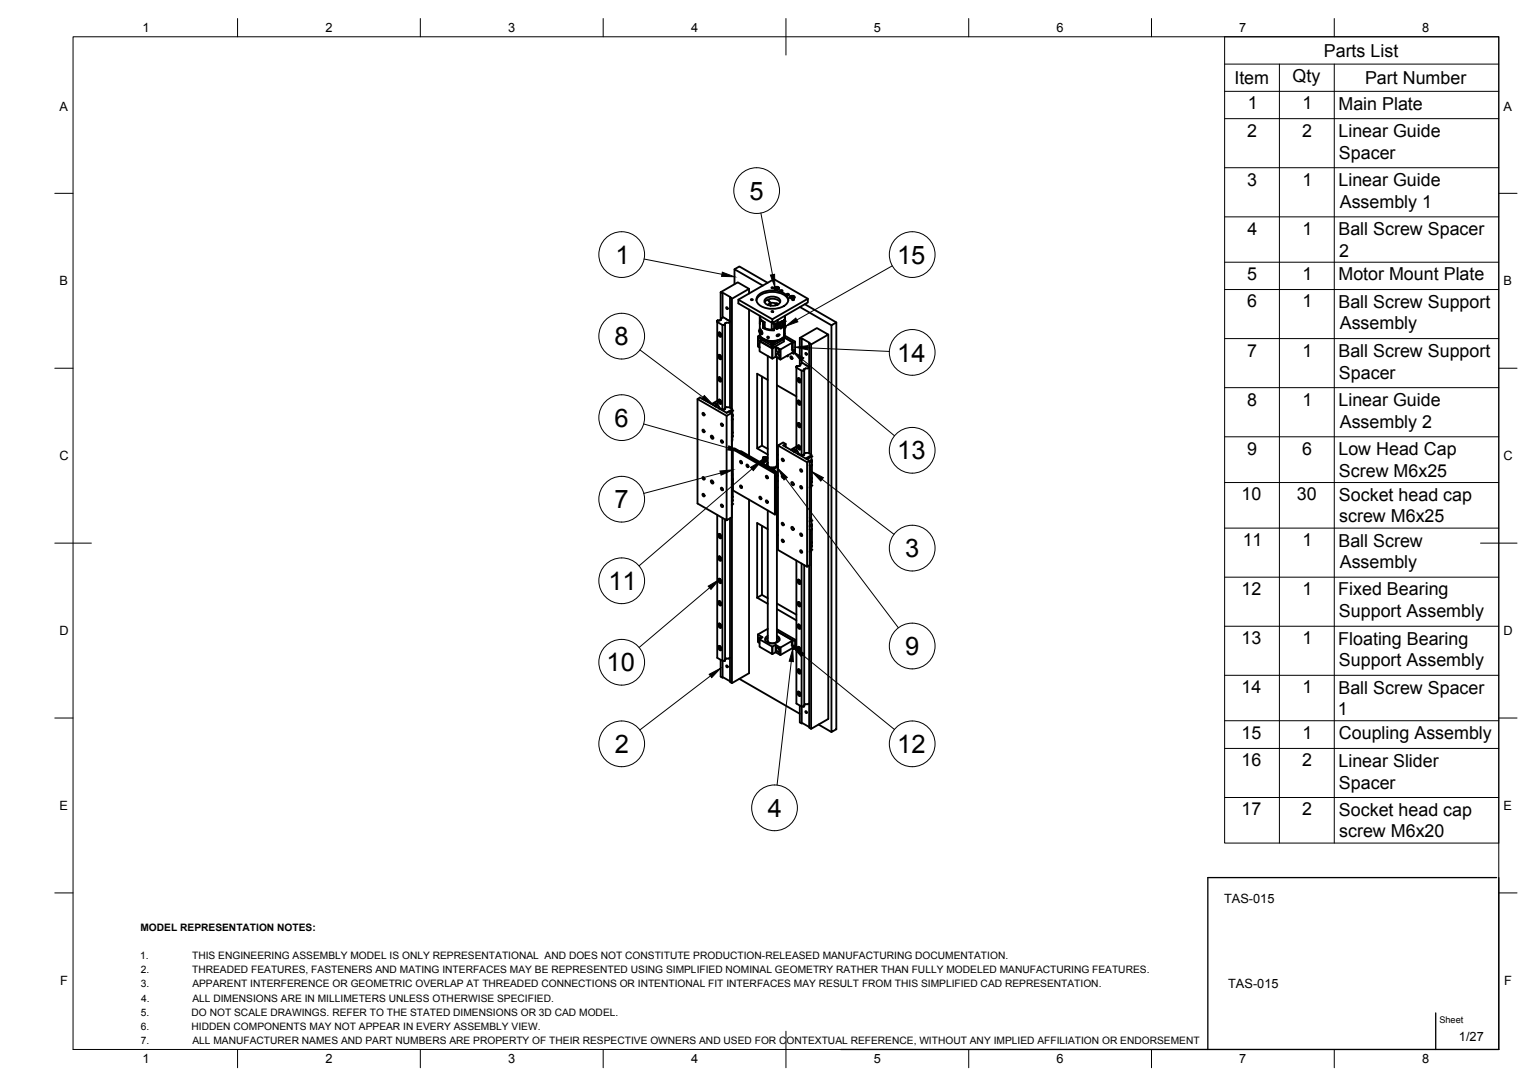
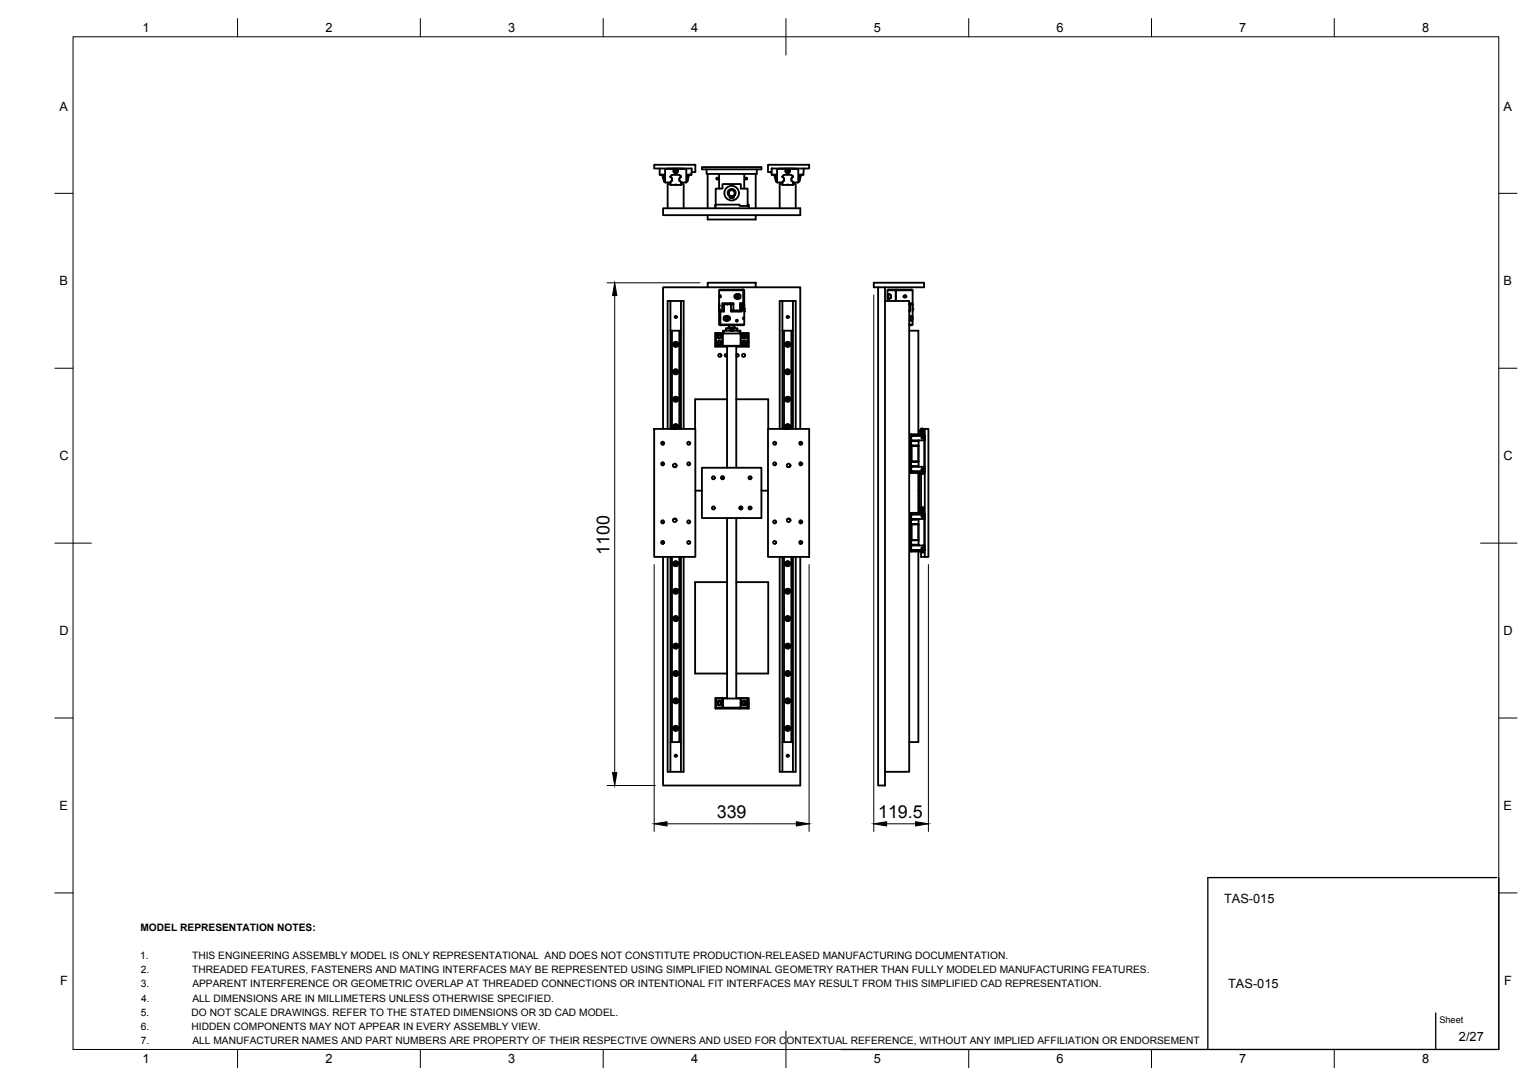
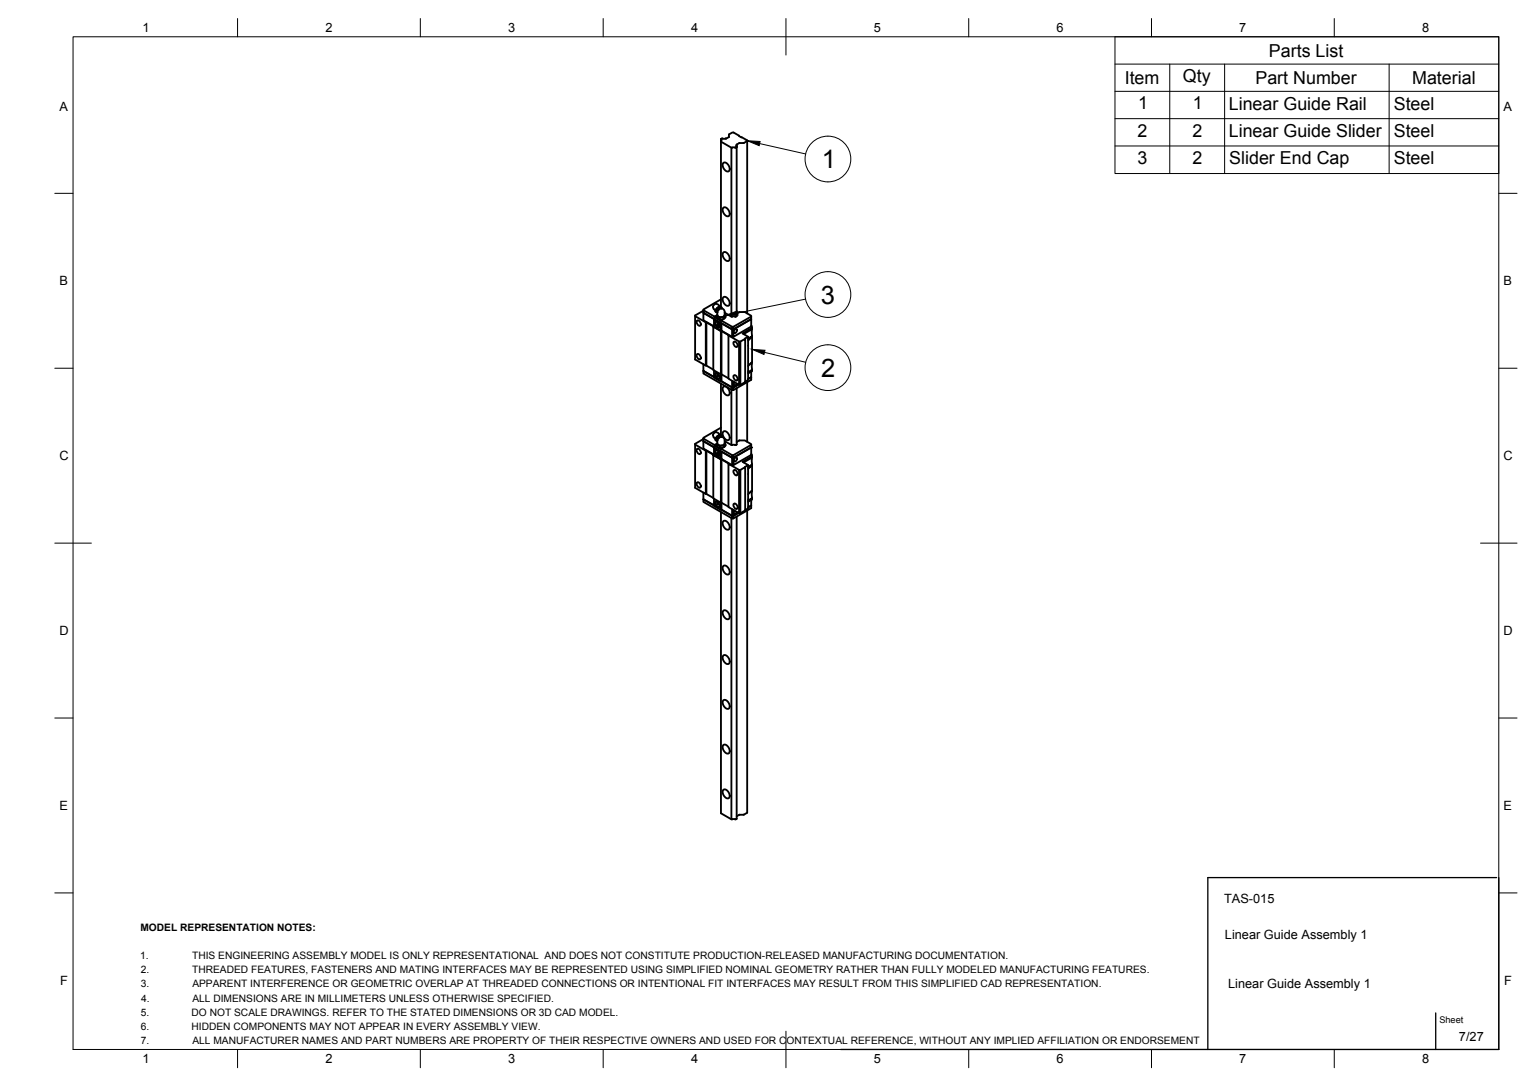
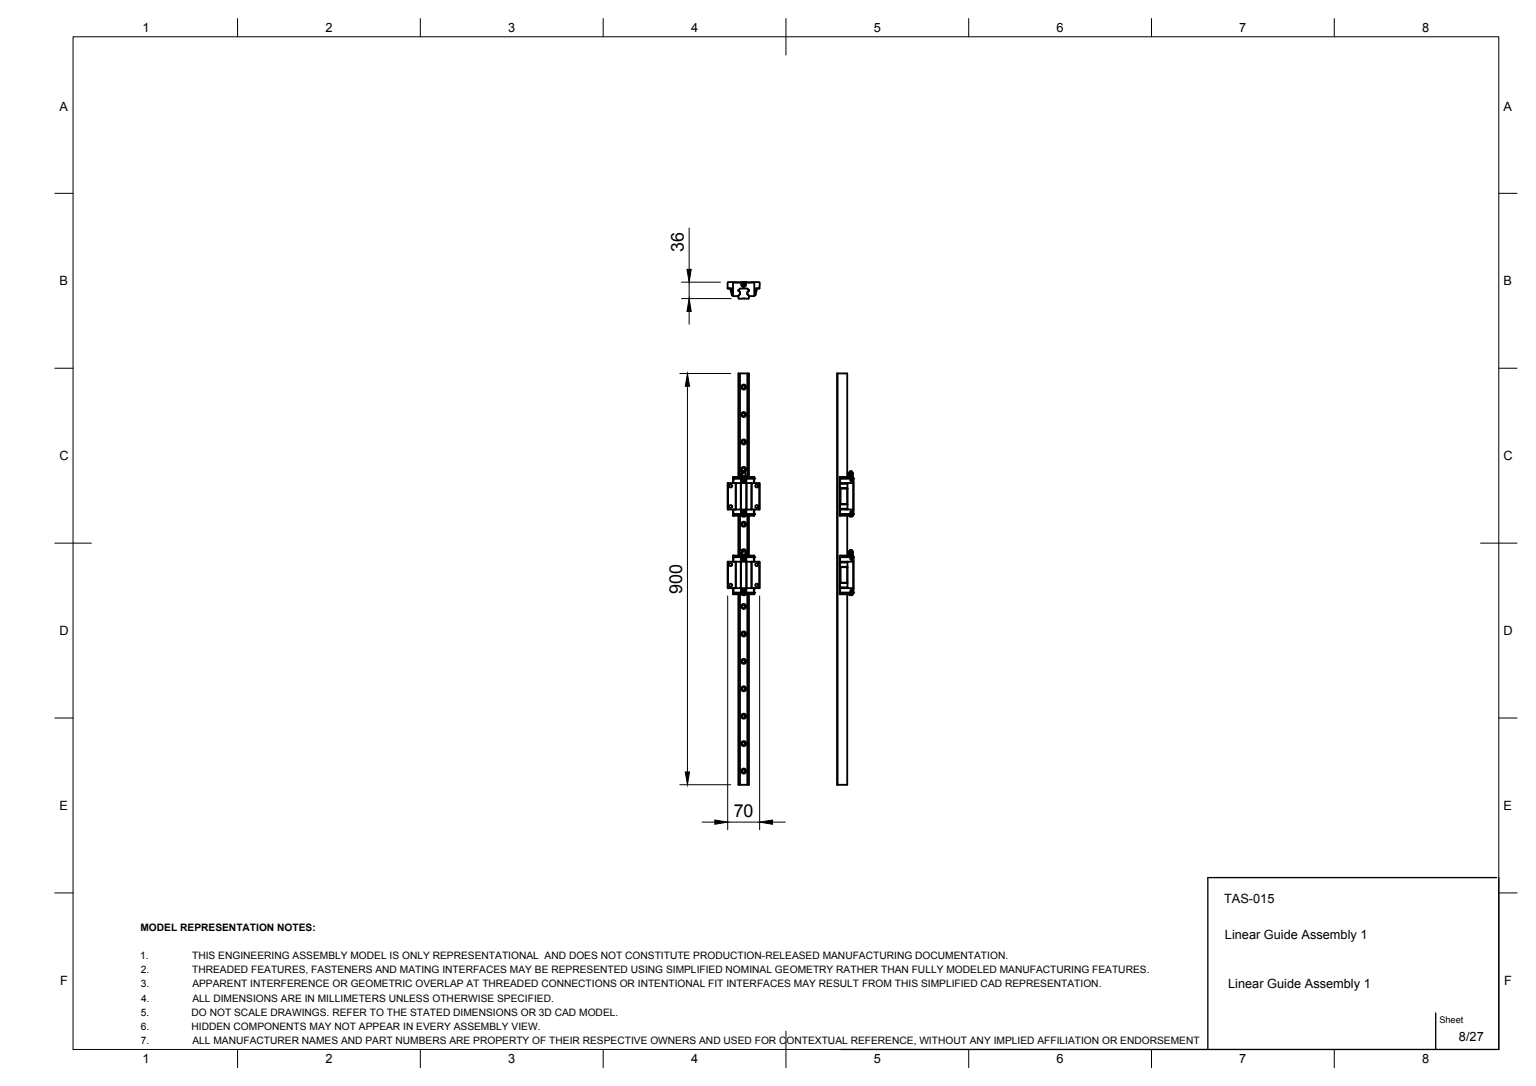
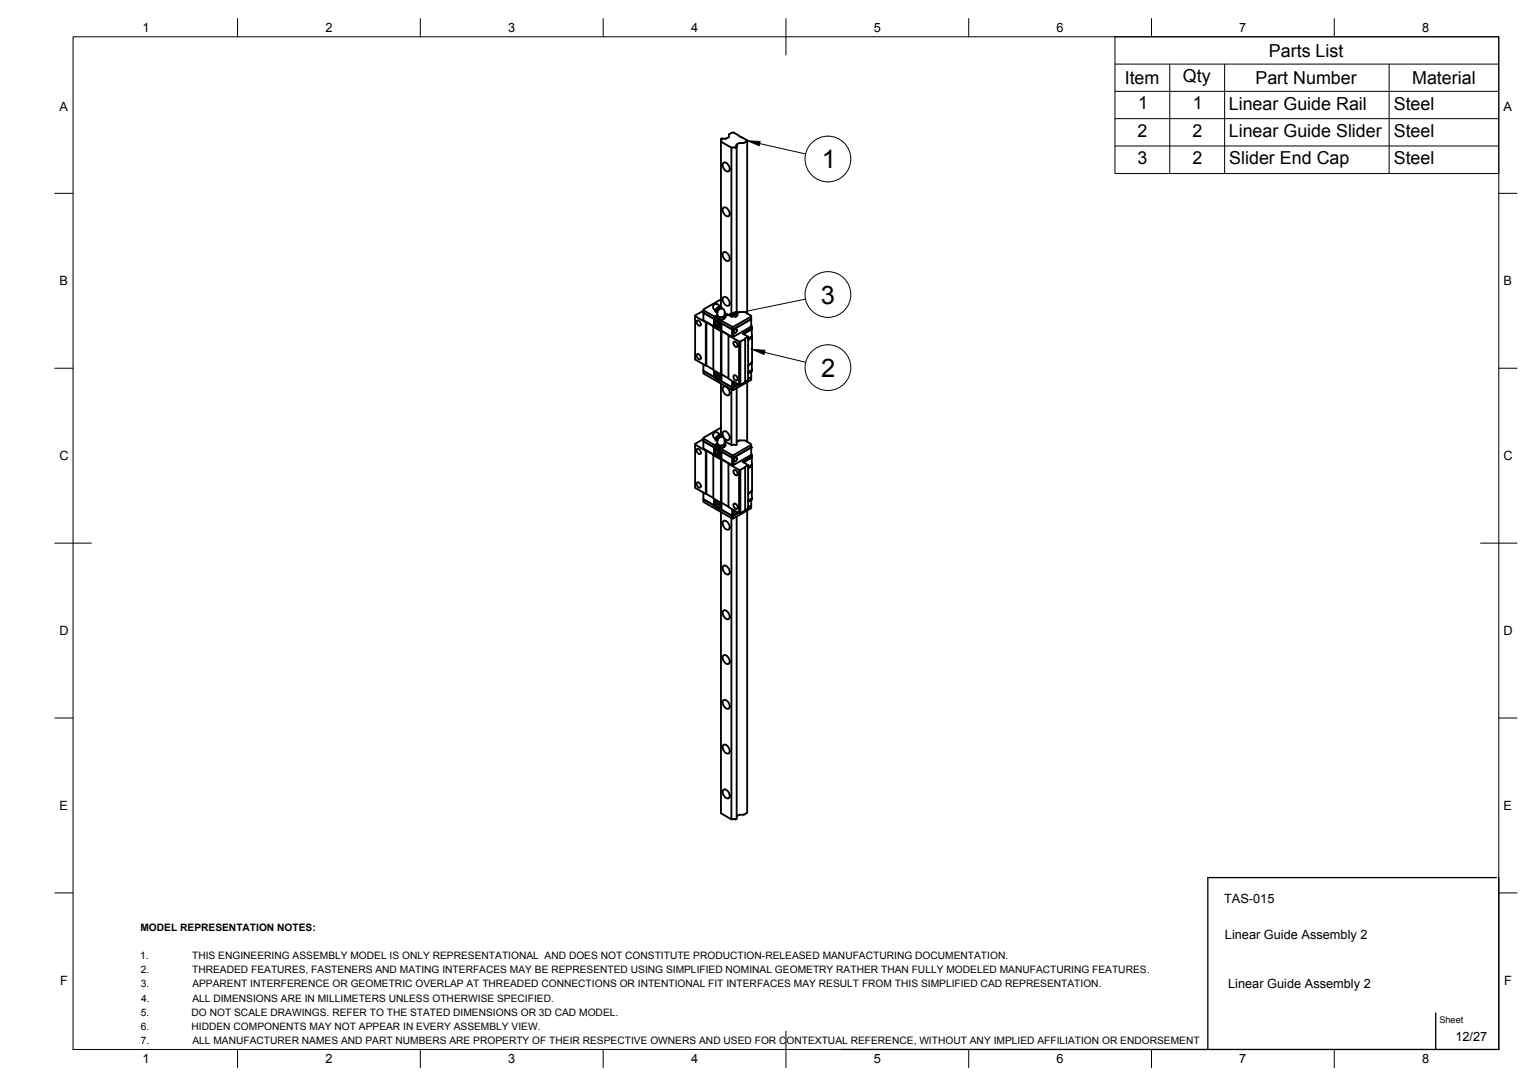
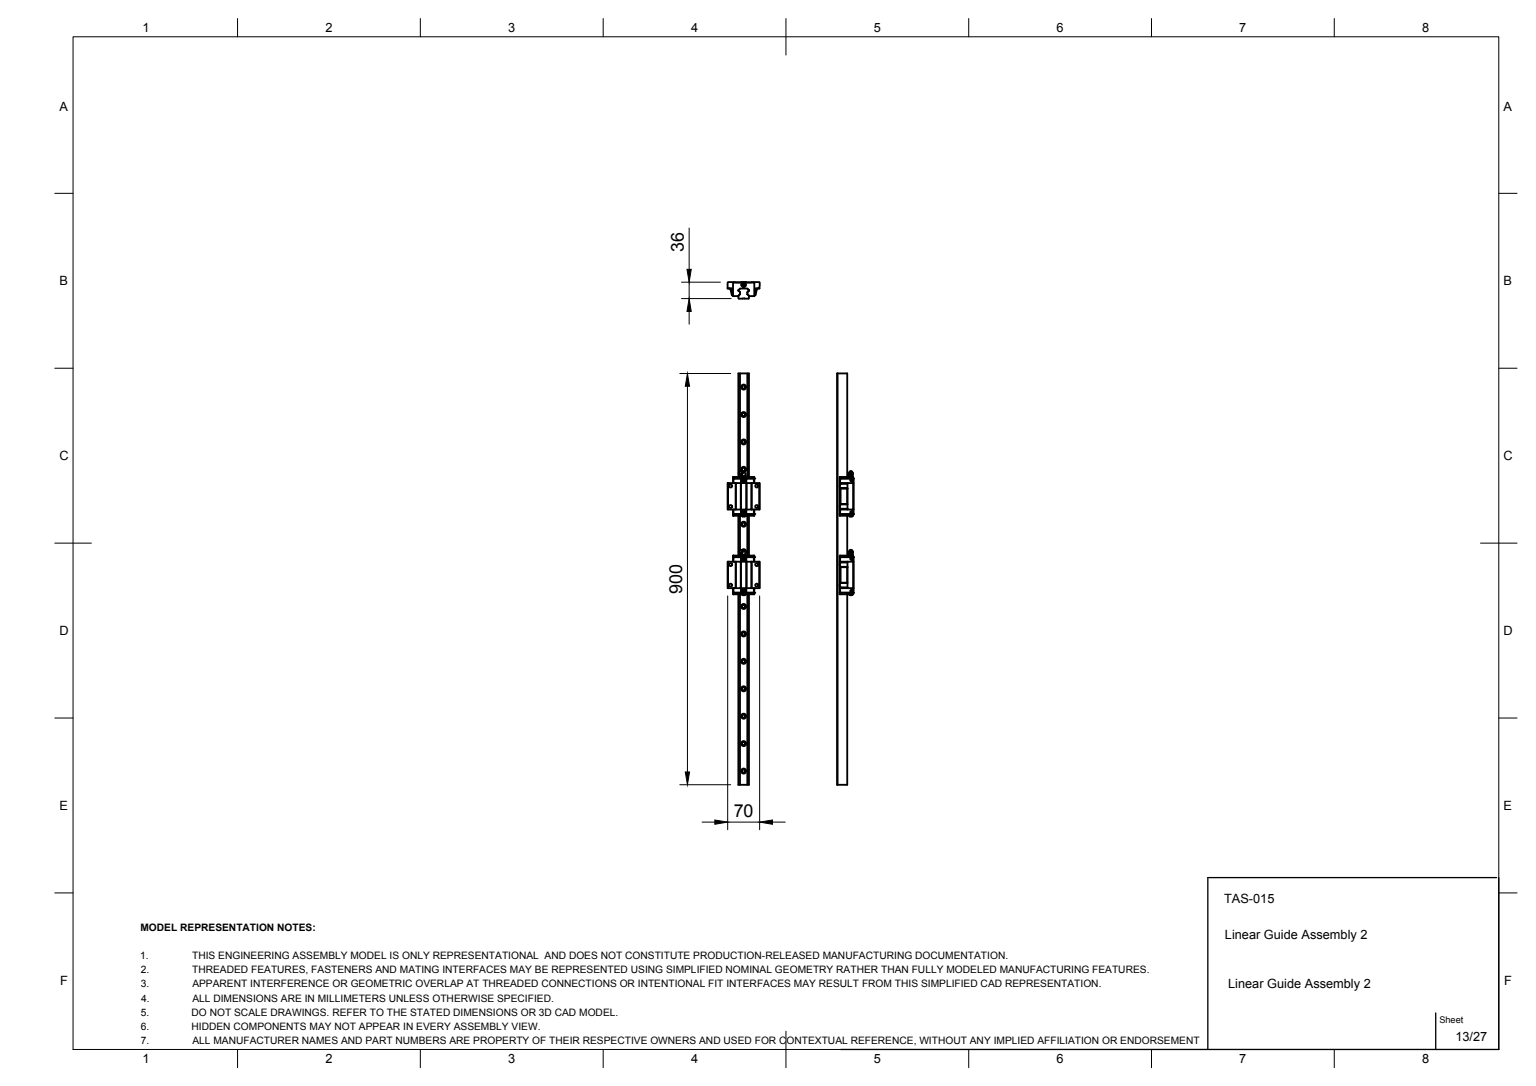
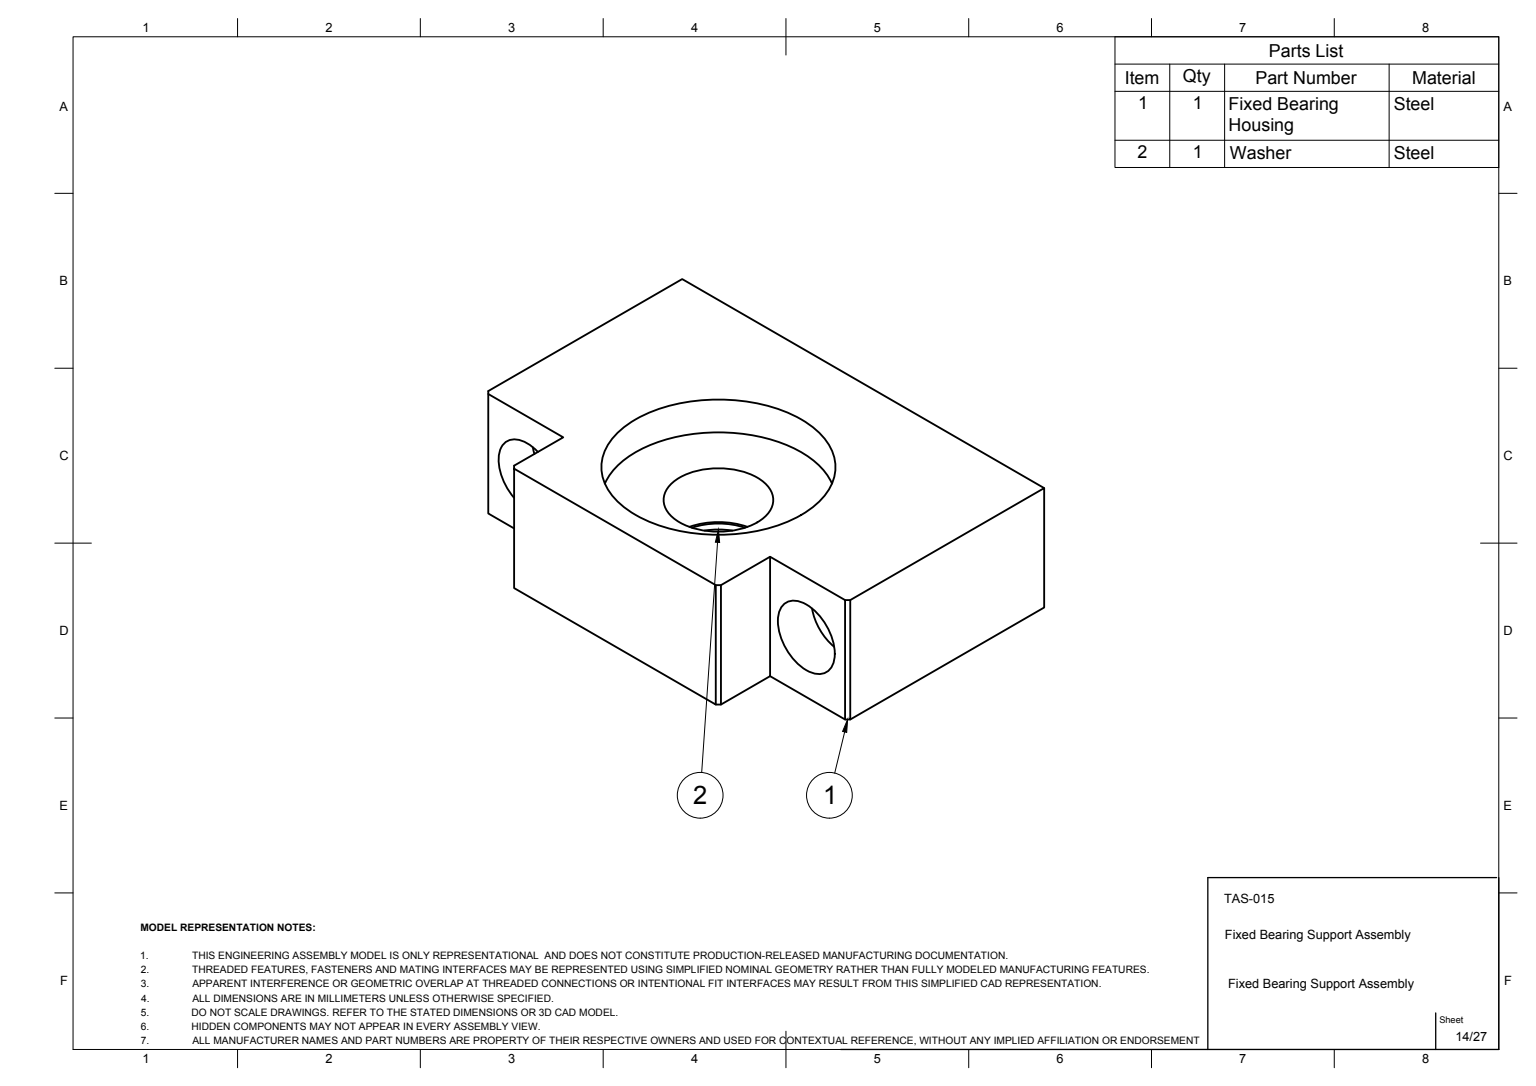
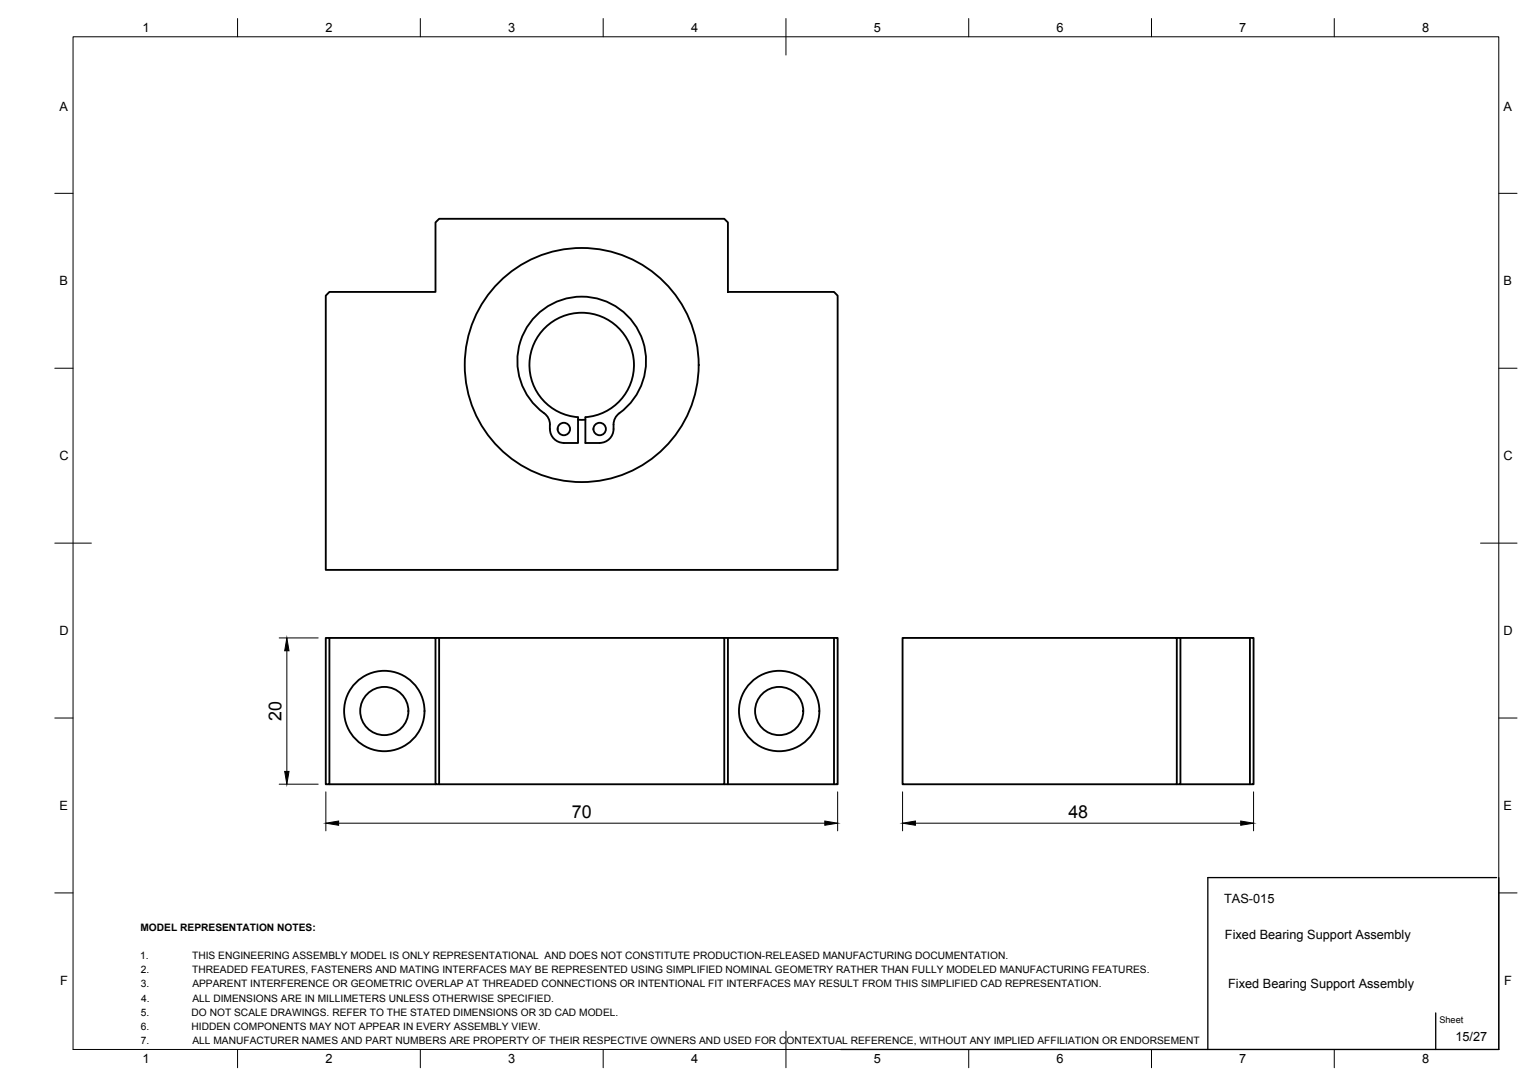
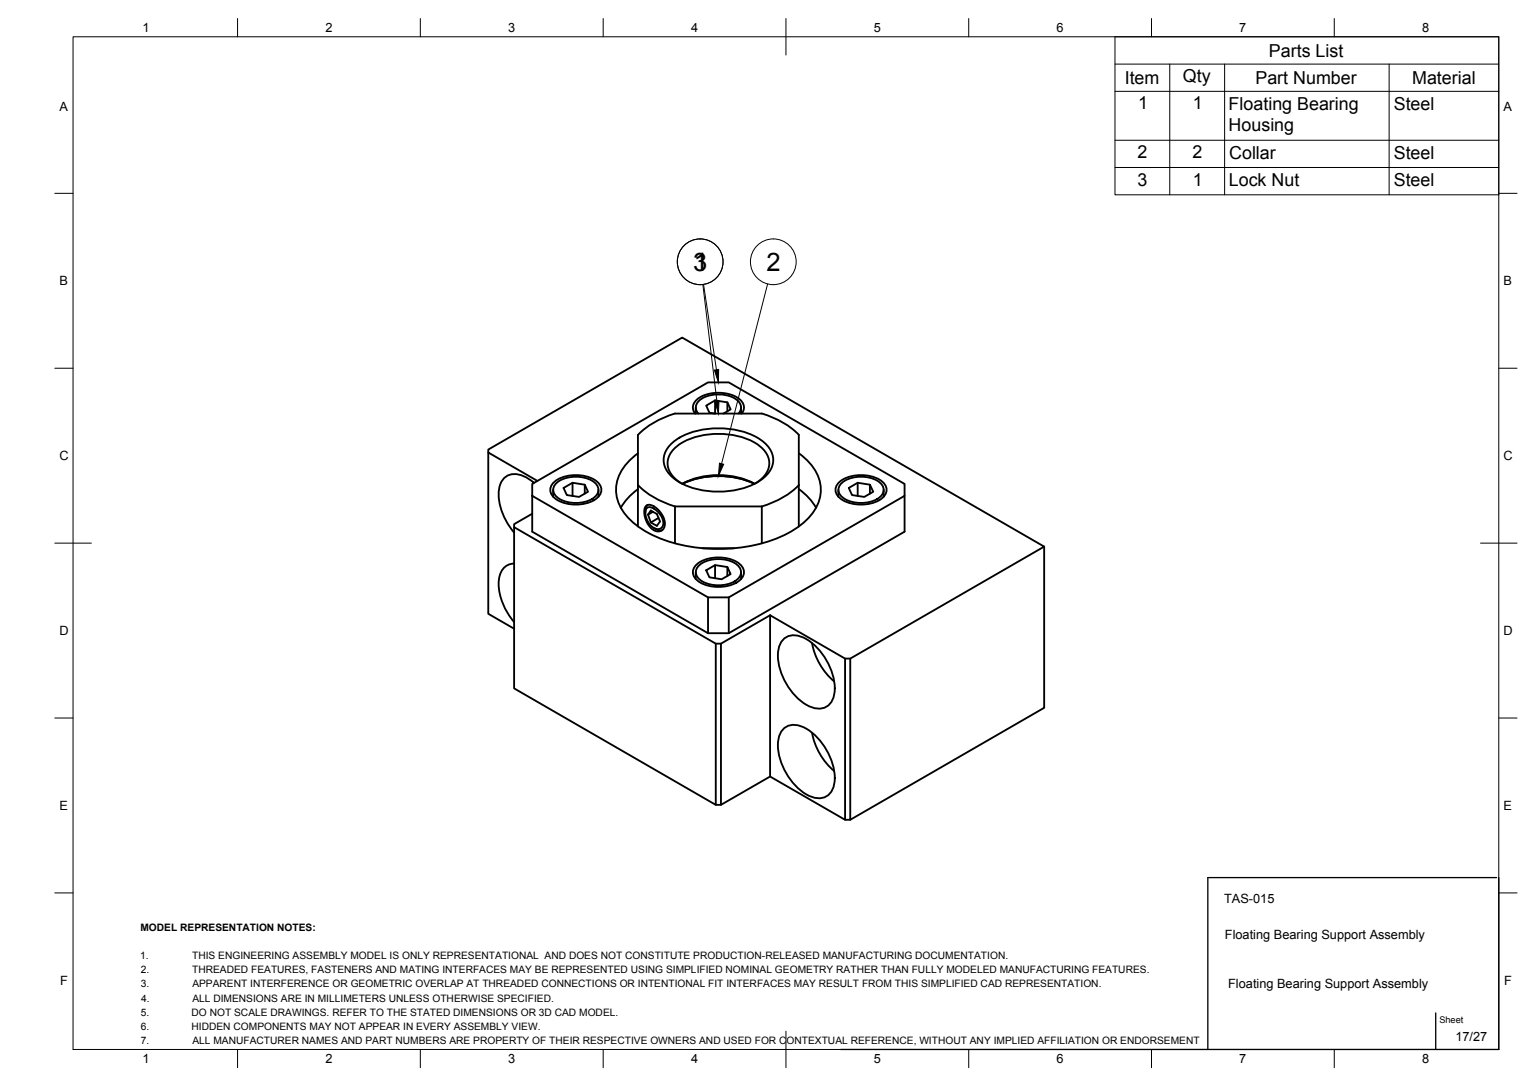
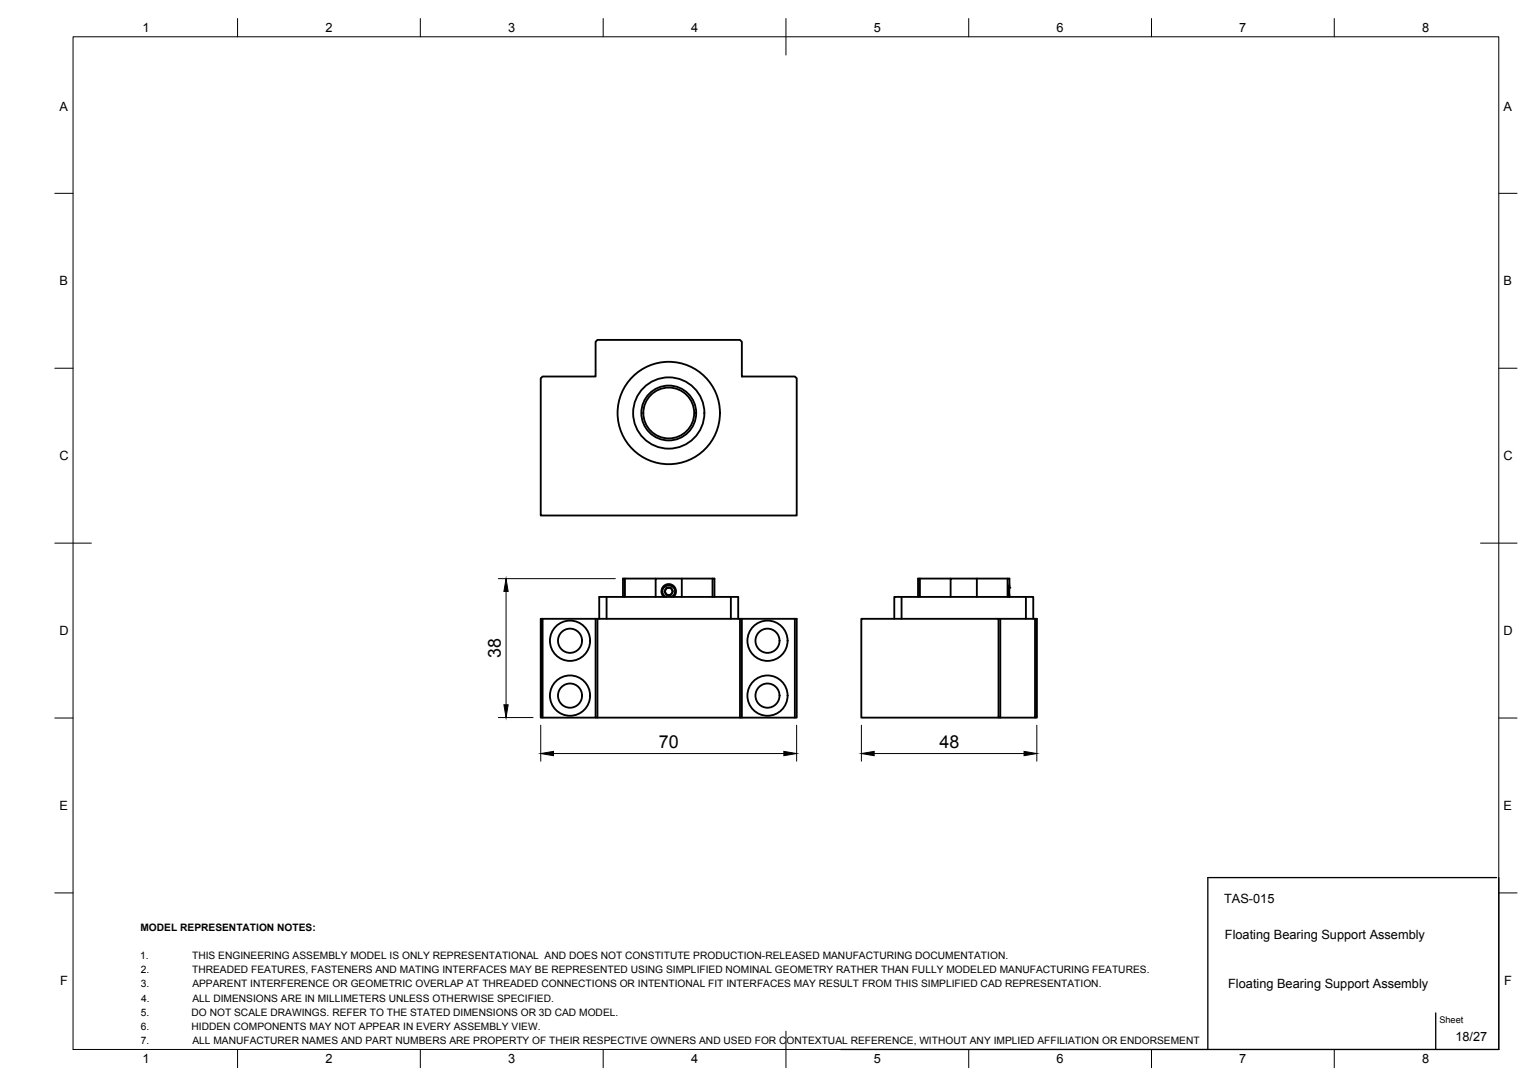
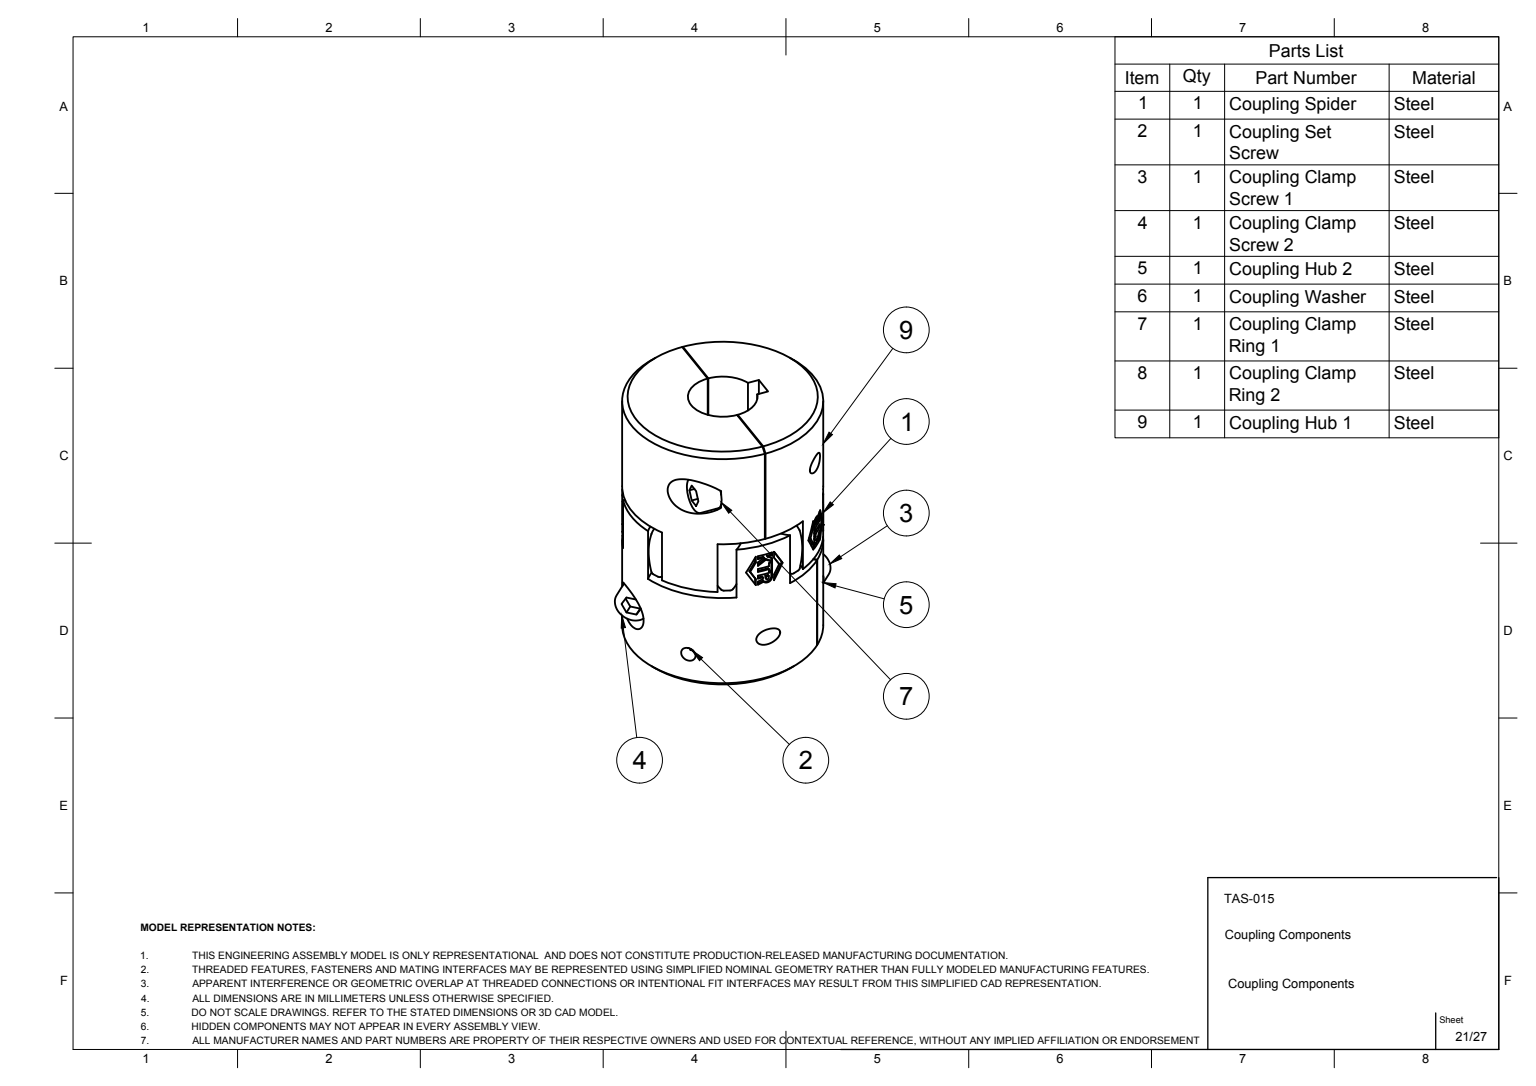
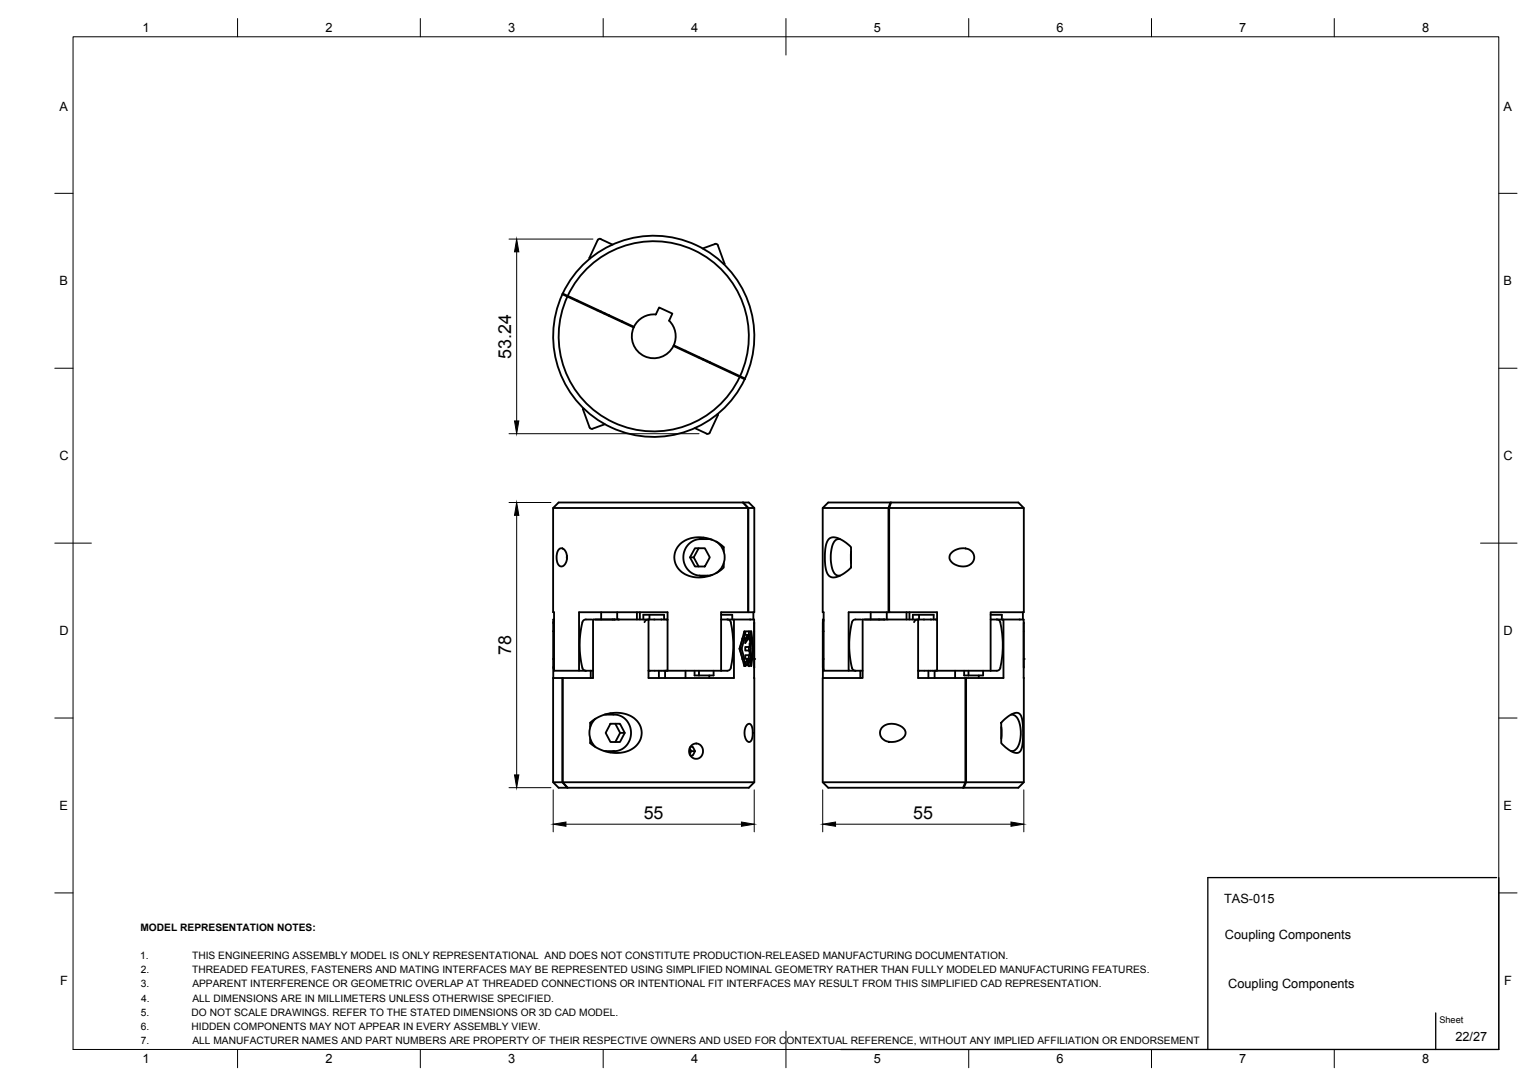
ISO-10303-21;
HEADER;
/* Generated by software containing ST-Developer
 * from STEP Tools, Inc. (www.steptools.com) 
 */

FILE_DESCRIPTION(
/* description */ ('STEP AP214'),
/* implementation_level */ '2;1');

FILE_NAME(
/* name */ 'TAS-015.step',
/* time_stamp */ '2026-11-15T14:49:54-08:00',
/* author */ (''),
/* organization */ (''),
/* preprocessor_version */ 'ST-DEVELOPER v20.2',
/* originating_system */ 'Autodesk Translation Framework v15.17.0.0',
/* authorisation */ '');

FILE_SCHEMA (('AUTOMOTIVE_DESIGN { 1 0 10303 214 3 1 1 }'));
ENDSEC;

DATA;
#10=MECHANICAL_DESIGN_GEOMETRIC_PRESENTATION_REPRESENTATION('',(#1098,#1099,
#1100,#1101,#1102,#1103,#1104,#1105,#1106,#1107,#1108,#1109,#1110,#1111,
#1112,#1113,#1114,#1115,#1116,#1117,#1118,#1119,#1120,#1121,#1122,#1123,
#1124,#1125,#1126,#1127,#1128,#1129,#1130,#1131,#1132),#66721);
#11=B_SPLINE_SURFACE_WITH_KNOTS('',3,3,((#41982,#41983,#41984,#41985,#41986),
(#41987,#41988,#41989,#41990,#41991),(#41992,#41993,#41994,#41995,#41996),
(#41997,#41998,#41999,#42000,#42001),(#42002,#42003,#42004,#42005,#42006),
(#42007,#42008,#42009,#42010,#42011),(#42012,#42013,#42014,#42015,#42016)),
 .UNSPECIFIED.,.F.,.F.,.F.,(4,1,1,1,4),(4,1,4),(0.02704890409976,0.25,0.5,
0.75,0.9277040914243),(0.6266253876044,7.194455259721,13.76279800701),
 .UNSPECIFIED.);
#12=B_SPLINE_SURFACE_WITH_KNOTS('',3,3,((#43036,#43037,#43038,#43039,#43040),
(#43041,#43042,#43043,#43044,#43045),(#43046,#43047,#43048,#43049,#43050),
(#43051,#43052,#43053,#43054,#43055)),.UNSPECIFIED.,.F.,.F.,.F.,(4,4),(4,
1,4),(0.07560247213886,0.9246170074165),(0.97123707704753,7.194455259721,
13.4176757847934),.UNSPECIFIED.);
#13=B_SPLINE_SURFACE_WITH_KNOTS('',3,3,((#43854,#43855,#43856,#43857,#43858),
(#43859,#43860,#43861,#43862,#43863),(#43864,#43865,#43866,#43867,#43868),
(#43869,#43870,#43871,#43872,#43873),(#43874,#43875,#43876,#43877,#43878),
(#43879,#43880,#43881,#43882,#43883),(#43884,#43885,#43886,#43887,#43888)),
 .UNSPECIFIED.,.F.,.F.,.F.,(4,1,1,1,4),(4,1,4),(0.07229619653719,0.25,0.5,
0.75,0.9729510902578),(0.6266257504199,7.194455259721,13.76275812373),
 .UNSPECIFIED.);
#14=B_SPLINE_SURFACE_WITH_KNOTS('',3,3,((#44879,#44880,#44881,#44882,#44883),
(#44884,#44885,#44886,#44887,#44888),(#44889,#44890,#44891,#44892,#44893),
(#44894,#44895,#44896,#44897,#44898),(#44899,#44900,#44901,#44902,#44903),
(#44904,#44905,#44906,#44907,#44908),(#44909,#44910,#44911,#44912,#44913)),
 .UNSPECIFIED.,.F.,.F.,.F.,(4,1,1,1,4),(4,1,4),(0.02704960022791,0.25,0.5,
0.75,0.9276685882704),(0.6266253876465,7.194455259721,13.76279800699),
 .UNSPECIFIED.);
#15=B_SPLINE_SURFACE_WITH_KNOTS('',3,3,((#45852,#45853,#45854,#45855,#45856),
(#45857,#45858,#45859,#45860,#45861),(#45862,#45863,#45864,#45865,#45866),
(#45867,#45868,#45869,#45870,#45871)),.UNSPECIFIED.,.F.,.F.,.F.,(4,4),(4,
1,4),(0.07560247213886,0.9246170074164),(0.971237077045854,7.194455259721,
13.4176757847952),.UNSPECIFIED.);
#16=B_SPLINE_SURFACE_WITH_KNOTS('',3,3,((#46672,#46673,#46674,#46675,#46676),
(#46677,#46678,#46679,#46680,#46681),(#46682,#46683,#46684,#46685,#46686),
(#46687,#46688,#46689,#46690,#46691),(#46692,#46693,#46694,#46695,#46696),
(#46697,#46698,#46699,#46700,#46701),(#46702,#46703,#46704,#46705,#46706)),
 .UNSPECIFIED.,.F.,.F.,.F.,(4,1,1,1,4),(4,1,4),(0.07233141172687,0.25,0.5,
0.75,0.972950399776),(0.6266257504498,7.194455259721,13.76275812375),
 .UNSPECIFIED.);
#17=B_SPLINE_SURFACE_WITH_KNOTS('',3,3,((#47663,#47664,#47665,#47666,#47667),
(#47668,#47669,#47670,#47671,#47672),(#47673,#47674,#47675,#47676,#47677),
(#47678,#47679,#47680,#47681,#47682),(#47683,#47684,#47685,#47686,#47687),
(#47688,#47689,#47690,#47691,#47692),(#47693,#47694,#47695,#47696,#47697)),
 .UNSPECIFIED.,.F.,.F.,.F.,(4,1,1,1,4),(4,1,4),(0.02704894056375,0.25,0.5,
0.75,0.9277022317281),(0.6266253876037,7.194455259721,13.76279800701),
 .UNSPECIFIED.);
#18=B_SPLINE_SURFACE_WITH_KNOTS('',3,3,((#48705,#48706,#48707,#48708,#48709),
(#48710,#48711,#48712,#48713,#48714),(#48715,#48716,#48717,#48718,#48719),
(#48720,#48721,#48722,#48723,#48724)),.UNSPECIFIED.,.F.,.F.,.F.,(4,4),(4,
1,4),(0.07561105541477,0.9246169072522),(0.971199375698935,7.194455259721,
13.4177134902227),.UNSPECIFIED.);
#19=B_SPLINE_SURFACE_WITH_KNOTS('',3,3,((#49555,#49556,#49557,#49558,#49559),
(#49560,#49561,#49562,#49563,#49564),(#49565,#49566,#49567,#49568,#49569),
(#49570,#49571,#49572,#49573,#49574),(#49575,#49576,#49577,#49578,#49579),
(#49580,#49581,#49582,#49583,#49584),(#49585,#49586,#49587,#49588,#49589)),
 .UNSPECIFIED.,.F.,.F.,.F.,(4,1,1,1,4),(4,1,4),(0.07233141172959,0.25,0.5,
0.75,0.9729503997759),(0.6266257504616,7.194455259721,13.76275812376),
 .UNSPECIFIED.);
#20=B_SPLINE_SURFACE_WITH_KNOTS('',3,3,((#50503,#50504,#50505,#50506,#50507),
(#50508,#50509,#50510,#50511,#50512),(#50513,#50514,#50515,#50516,#50517),
(#50518,#50519,#50520,#50521,#50522),(#50523,#50524,#50525,#50526,#50527),
(#50528,#50529,#50530,#50531,#50532),(#50533,#50534,#50535,#50536,#50537)),
 .UNSPECIFIED.,.F.,.F.,.F.,(4,1,1,1,4),(4,1,4),(0.0270489040004,0.25,0.5,
0.75,0.9277040964915),(0.6266253875094,7.194455259721,13.76279800735),
 .UNSPECIFIED.);
#21=B_SPLINE_SURFACE_WITH_KNOTS('',3,3,((#51508,#51509,#51510,#51511,#51512),
(#51513,#51514,#51515,#51516,#51517),(#51518,#51519,#51520,#51521,#51522),
(#51523,#51524,#51525,#51526,#51527)),.UNSPECIFIED.,.F.,.F.,.F.,(4,4),(4,
1,4),(0.07561105541523,0.9246169072518),(0.971199375716696,7.194455259721,
13.4177134861273),.UNSPECIFIED.);
#22=B_SPLINE_SURFACE_WITH_KNOTS('',3,3,((#52356,#52357,#52358,#52359,#52360),
(#52361,#52362,#52363,#52364,#52365),(#52366,#52367,#52368,#52369,#52370),
(#52371,#52372,#52373,#52374,#52375),(#52376,#52377,#52378,#52379,#52380),
(#52381,#52382,#52383,#52384,#52385),(#52386,#52387,#52388,#52389,#52390)),
 .UNSPECIFIED.,.F.,.F.,.F.,(4,1,1,1,4),(4,1,4),(0.07229571648343,0.25,0.5,
0.75,0.9729510996705),(0.6266257503296,7.194455259721,13.76275812362),
 .UNSPECIFIED.);
#23=B_SPLINE_SURFACE_WITH_KNOTS('',3,3,((#53369,#53370,#53371,#53372,#53373),
(#53374,#53375,#53376,#53377,#53378),(#53379,#53380,#53381,#53382,#53383),
(#53384,#53385,#53386,#53387,#53388),(#53389,#53390,#53391,#53392,#53393),
(#53394,#53395,#53396,#53397,#53398),(#53399,#53400,#53401,#53402,#53403)),
 .UNSPECIFIED.,.F.,.F.,.F.,(4,1,1,1,4),(4,1,4),(0.02704960022791,0.25,0.5,
0.75,0.9276685882704),(0.6266253875523,7.194455259721,13.76279800732),
 .UNSPECIFIED.);
#24=B_SPLINE_SURFACE_WITH_KNOTS('',3,3,((#54369,#54370,#54371,#54372,#54373),
(#54374,#54375,#54376,#54377,#54378),(#54379,#54380,#54381,#54382,#54383),
(#54384,#54385,#54386,#54387,#54388)),.UNSPECIFIED.,.F.,.F.,.F.,(4,4),(4,
1,4),(0.07561112179917,0.9246168071327),(0.971161649229297,7.194455259721,
13.4177512126147),.UNSPECIFIED.);
#25=B_SPLINE_SURFACE_WITH_KNOTS('',3,3,((#55289,#55290,#55291,#55292,#55293),
(#55294,#55295,#55296,#55297,#55298),(#55299,#55300,#55301,#55302,#55303),
(#55304,#55305,#55306,#55307,#55308),(#55309,#55310,#55311,#55312,#55313),
(#55314,#55315,#55316,#55317,#55318),(#55319,#55320,#55321,#55322,#55323)),
 .UNSPECIFIED.,.F.,.F.,.F.,(4,1,1,1,4),(4,1,4),(0.07230494309637,0.25,0.5,
0.75,0.9729509187597),(0.626625750321,7.194455259721,13.76275812361),
 .UNSPECIFIED.);
#26=B_SPLINE_SURFACE_WITH_KNOTS('',3,3,((#56290,#56291,#56292,#56293,#56294),
(#56295,#56296,#56297,#56298,#56299),(#56300,#56301,#56302,#56303,#56304),
(#56305,#56306,#56307,#56308,#56309),(#56310,#56311,#56312,#56313,#56314),
(#56315,#56316,#56317,#56318,#56319),(#56320,#56321,#56322,#56323,#56324)),
 .UNSPECIFIED.,.F.,.F.,.F.,(4,1,1,1,4),(4,1,4),(0.02704894454492,0.25,0.5,
0.75,0.927702028685),(0.6266253875099,7.194455259721,13.76279800735),
 .UNSPECIFIED.);
#27=B_SPLINE_SURFACE_WITH_KNOTS('',3,3,((#57264,#57265,#57266,#57267,#57268),
(#57269,#57270,#57271,#57272,#57273),(#57274,#57275,#57276,#57277,#57278),
(#57279,#57280,#57281,#57282,#57283)),.UNSPECIFIED.,.F.,.F.,.F.,(4,4),(4,
1,4),(0.07561112179916,0.9246168071327),(0.971161649224581,7.194455259721,
13.4177512126194),.UNSPECIFIED.);
#28=B_SPLINE_SURFACE_WITH_KNOTS('',3,3,((#58109,#58110,#58111,#58112,#58113),
(#58114,#58115,#58116,#58117,#58118),(#58119,#58120,#58121,#58122,#58123),
(#58124,#58125,#58126,#58127,#58128),(#58129,#58130,#58131,#58132,#58133),
(#58134,#58135,#58136,#58137,#58138),(#58139,#58140,#58141,#58142,#58143)),
 .UNSPECIFIED.,.F.,.F.,.F.,(4,1,1,1,4),(4,1,4),(0.07233141172959,0.25,0.5,
0.75,0.9729503997759),(0.6266257503696,7.194455259721,13.76275812364),
 .UNSPECIFIED.);
#29=B_SPLINE_SURFACE_WITH_KNOTS('',3,3,((#58957,#58958,#58959,#58960,#58961),
(#58962,#58963,#58964,#58965,#58966),(#58967,#58968,#58969,#58970,#58971),
(#58972,#58973,#58974,#58975,#58976),(#58977,#58978,#58979,#58980,#58981),
(#58982,#58983,#58984,#58985,#58986),(#58987,#58988,#58989,#58990,#58991)),
 .UNSPECIFIED.,.F.,.F.,.F.,(4,1,1,1,4),(4,1,4),(0.02704893649799,0.25,0.5,
0.75,0.9277024390857),(0.6266253876044,7.194455259721,13.76279800701),
 .UNSPECIFIED.);
#30=B_SPLINE_SURFACE_WITH_KNOTS('',3,3,((#59443,#59444,#59445,#59446,#59447),
(#59448,#59449,#59450,#59451,#59452),(#59453,#59454,#59455,#59456,#59457),
(#59458,#59459,#59460,#59461,#59462)),.UNSPECIFIED.,.F.,.F.,.F.,(4,4),(4,
1,4),(0.07560233772369,0.9246171082587),(0.971274990731998,7.194455259721,
13.4176378711108),.UNSPECIFIED.);
#31=B_SPLINE_SURFACE_WITH_KNOTS('',3,3,((#60261,#60262,#60263,#60264,#60265),
(#60266,#60267,#60268,#60269,#60270),(#60271,#60272,#60273,#60274,#60275),
(#60276,#60277,#60278,#60279,#60280),(#60281,#60282,#60283,#60284,#60285),
(#60286,#60287,#60288,#60289,#60290),(#60291,#60292,#60293,#60294,#60295)),
 .UNSPECIFIED.,.F.,.F.,.F.,(4,1,1,1,4),(4,1,4),(0.07233141172722,0.25,0.5,
0.75,0.9729503997759),(0.6266257504058,7.194455259721,13.76275812373),
 .UNSPECIFIED.);
#32=B_SPLINE_SURFACE_WITH_KNOTS('',3,3,((#61841,#61842,#61843,#61844,#61845),
(#61846,#61847,#61848,#61849,#61850),(#61851,#61852,#61853,#61854,#61855),
(#61856,#61857,#61858,#61859,#61860),(#61861,#61862,#61863,#61864,#61865),
(#61866,#61867,#61868,#61869,#61870),(#61871,#61872,#61873,#61874,#61875)),
 .UNSPECIFIED.,.F.,.F.,.F.,(4,1,1,1,4),(4,1,4),(0.02704957693913,0.25,0.5,
0.75,0.9276697760189),(0.6266253874895,7.194455259721,13.76279800736),
 .UNSPECIFIED.);
#33=B_SPLINE_SURFACE_WITH_KNOTS('',3,3,((#62817,#62818,#62819,#62820,#62821),
(#62822,#62823,#62824,#62825,#62826),(#62827,#62828,#62829,#62830,#62831),
(#62832,#62833,#62834,#62835,#62836)),.UNSPECIFIED.,.F.,.F.,.F.,(4,4),(4,
1,4),(0.07561118765193,0.9246167076829),(0.971124132828661,7.194455259721,
13.4177887331011),.UNSPECIFIED.);
#34=B_SPLINE_SURFACE_WITH_KNOTS('',3,3,((#63659,#63660,#63661,#63662,#63663),
(#63664,#63665,#63666,#63667,#63668),(#63669,#63670,#63671,#63672,#63673),
(#63674,#63675,#63676,#63677,#63678),(#63679,#63680,#63681,#63682,#63683),
(#63684,#63685,#63686,#63687,#63688),(#63689,#63690,#63691,#63692,#63693)),
 .UNSPECIFIED.,.F.,.F.,.F.,(4,1,1,1,4),(4,1,4),(0.07233021543657,0.25,0.5,
0.75,0.9729504232322),(0.6266257503101,7.194455259721,13.7627581236),
 .UNSPECIFIED.);
#35=SPHERICAL_SURFACE('',#27201,1.2);
#36=SPHERICAL_SURFACE('',#27220,4.);
#37=SPHERICAL_SURFACE('',#27729,1.000000122615);
#38=SPHERICAL_SURFACE('',#27733,1.000005019194);
#39=SPHERICAL_SURFACE('',#27736,1.000005006638);
#40=SPHERICAL_SURFACE('',#27742,1.000000000939);
#41=SPHERICAL_SURFACE('',#27750,1.000000122615);
#42=SPHERICAL_SURFACE('',#27755,1.000005019194);
#43=SPHERICAL_SURFACE('',#27758,1.000005006638);
#44=SPHERICAL_SURFACE('',#27764,1.000000000939);
#45=SPHERICAL_SURFACE('',#27772,1.000000122615);
#46=SPHERICAL_SURFACE('',#27776,1.000005019194);
#47=SPHERICAL_SURFACE('',#27779,1.000005006638);
#48=SPHERICAL_SURFACE('',#27785,1.000000000939);
#49=SPHERICAL_SURFACE('',#27794,1.000000122615);
#50=SPHERICAL_SURFACE('',#27798,1.0000050192);
#51=SPHERICAL_SURFACE('',#27802,1.000005006635);
#52=SPHERICAL_SURFACE('',#27808,1.000000000939);
#53=SPHERICAL_SURFACE('',#27816,1.000000122616);
#54=SPHERICAL_SURFACE('',#27821,1.0000050192);
#55=SPHERICAL_SURFACE('',#27824,1.000005006635);
#56=SPHERICAL_SURFACE('',#27830,1.000000000939);
#57=SPHERICAL_SURFACE('',#27837,1.000000122616);
#58=SPHERICAL_SURFACE('',#27841,1.0000050192);
#59=SPHERICAL_SURFACE('',#27845,1.000005006635);
#60=SPHERICAL_SURFACE('',#27851,1.000000000939);
#61=SPHERICAL_SURFACE('',#27857,1.000000122614);
#62=SPHERICAL_SURFACE('',#27865,1.00000000094);
#63=SPHERICAL_SURFACE('',#27870,1.000005006638);
#64=SPHERICAL_SURFACE('',#27874,1.000005019194);
#65=SPHERICAL_SURFACE('',#27882,1.000000122616);
#66=SPHERICAL_SURFACE('',#27887,1.0000050192);
#67=SPHERICAL_SURFACE('',#27890,1.000005006635);
#68=SPHERICAL_SURFACE('',#27896,1.000000000939);
#69=TOROIDAL_SURFACE('',#27193,4.25,1.21);
#70=TOROIDAL_SURFACE('',#27280,6.20000000000003,0.199999999999989);
#71=TOROIDAL_SURFACE('',#27288,7.7000000000001,0.199999999999989);
#72=TOROIDAL_SURFACE('',#27299,7.7,0.200000000000001);
#73=TOROIDAL_SURFACE('',#27366,17.5,0.5);
#74=TOROIDAL_SURFACE('',#27372,28.,1.);
#75=TOROIDAL_SURFACE('',#27374,28.,1.);
#76=TOROIDAL_SURFACE('',#27380,28.,1.);
#77=TOROIDAL_SURFACE('',#27382,28.,1.);
#78=TOROIDAL_SURFACE('',#27963,4.3999999999,0.6);
#79=TOROIDAL_SURFACE('',#27985,4.3999999999,0.6);
#80=TOROIDAL_SURFACE('',#28228,4.3999999999,0.6);
#81=TOROIDAL_SURFACE('',#28250,4.3999999999,0.6);
#82=(
BOUNDED_CURVE()
B_SPLINE_CURVE(2,(#37654,#37655,#37656),.UNSPECIFIED.,.F.,.F.)
B_SPLINE_CURVE_WITH_KNOTS((3,3),(-1.29356557390797,0.),.UNSPECIFIED.)
CURVE()
GEOMETRIC_REPRESENTATION_ITEM()
RATIONAL_B_SPLINE_CURVE((0.954658532851732,0.77704632554749,1.))
REPRESENTATION_ITEM('')
);
#83=(
BOUNDED_CURVE()
B_SPLINE_CURVE(2,(#39567,#39568,#39569),.UNSPECIFIED.,.F.,.F.)
B_SPLINE_CURVE_WITH_KNOTS((3,3),(-1.38994780338837,-1.00314154055664),
 .UNSPECIFIED.)
CURVE()
GEOMETRIC_REPRESENTATION_ITEM()
RATIONAL_B_SPLINE_CURVE((1.79495951130746,1.93380011269289,1.93380011269289))
REPRESENTATION_ITEM('')
);
#84=(
BOUNDED_CURVE()
B_SPLINE_CURVE(2,(#39570,#39571,#39572),.UNSPECIFIED.,.F.,.F.)
B_SPLINE_CURVE_WITH_KNOTS((3,3),(-1.00619430729118,-0.618602381117838),
 .UNSPECIFIED.)
CURVE()
GEOMETRIC_REPRESENTATION_ITEM()
RATIONAL_B_SPLINE_CURVE((1.93745653739061,1.93745653739061,1.7983534165231))
REPRESENTATION_ITEM('')
);
#85=(
BOUNDED_CURVE()
B_SPLINE_CURVE(2,(#39578,#39579,#39580),.UNSPECIFIED.,.F.,.F.)
B_SPLINE_CURVE_WITH_KNOTS((3,3),(-1.38994780338837,-1.00314154055664),
 .UNSPECIFIED.)
CURVE()
GEOMETRIC_REPRESENTATION_ITEM()
RATIONAL_B_SPLINE_CURVE((1.79495951130745,1.93380011269288,1.93380011269288))
REPRESENTATION_ITEM('')
);
#86=(
BOUNDED_CURVE()
B_SPLINE_CURVE(2,(#39581,#39582,#39583),.UNSPECIFIED.,.F.,.F.)
B_SPLINE_CURVE_WITH_KNOTS((3,3),(-1.00619430729117,-0.618602381117832),
 .UNSPECIFIED.)
CURVE()
GEOMETRIC_REPRESENTATION_ITEM()
RATIONAL_B_SPLINE_CURVE((1.9374565373906,1.9374565373906,1.79835341652309))
REPRESENTATION_ITEM('')
);
#87=(
BOUNDED_CURVE()
B_SPLINE_CURVE(2,(#39705,#39706,#39707),.UNSPECIFIED.,.F.,.F.)
B_SPLINE_CURVE_WITH_KNOTS((3,3),(-1.14357963809553,-0.720457873954785),
 .UNSPECIFIED.)
CURVE()
GEOMETRIC_REPRESENTATION_ITEM()
RATIONAL_B_SPLINE_CURVE((2.10284386262275,2.10284386262275,1.95186646604709))
REPRESENTATION_ITEM('')
);
#88=(
BOUNDED_CURVE()
B_SPLINE_CURVE(2,(#39708,#39709,#39710),.UNSPECIFIED.,.F.,.F.)
B_SPLINE_CURVE_WITH_KNOTS((3,3),(-1.51402948258723,-1.10175646251728),
 .UNSPECIFIED.)
CURVE()
GEOMETRIC_REPRESENTATION_ITEM()
RATIONAL_B_SPLINE_CURVE((1.90498640166842,2.0523376126434,2.0523376126434))
REPRESENTATION_ITEM('')
);
#89=(
BOUNDED_CURVE()
B_SPLINE_CURVE(2,(#39713,#39714,#39715),.UNSPECIFIED.,.F.,.F.)
B_SPLINE_CURVE_WITH_KNOTS((3,3),(-1.00619430729147,-0.618602381118052),
 .UNSPECIFIED.)
CURVE()
GEOMETRIC_REPRESENTATION_ITEM()
RATIONAL_B_SPLINE_CURVE((1.93745653739095,1.93745653739095,1.79835341652342))
REPRESENTATION_ITEM('')
);
#90=(
BOUNDED_CURVE()
B_SPLINE_CURVE(2,(#39716,#39717,#39718),.UNSPECIFIED.,.F.,.F.)
B_SPLINE_CURVE_WITH_KNOTS((3,3),(-1.59428966155348,-1.16547770853232),
 .UNSPECIFIED.)
CURVE()
GEOMETRIC_REPRESENTATION_ITEM()
RATIONAL_B_SPLINE_CURVE((1.97645710138757,2.12933659022722,2.12933659022723))
REPRESENTATION_ITEM('')
);
#91=(
BOUNDED_CURVE()
B_SPLINE_CURVE(2,(#39721,#39722,#39723),.UNSPECIFIED.,.F.,.F.)
B_SPLINE_CURVE_WITH_KNOTS((3,3),(-1.39378623346489,-1.00619430729147),
 .UNSPECIFIED.)
CURVE()
GEOMETRIC_REPRESENTATION_ITEM()
RATIONAL_B_SPLINE_CURVE((1.79835341652342,1.93745653739095,1.93745653739095))
REPRESENTATION_ITEM('')
);
#92=(
BOUNDED_CURVE()
B_SPLINE_CURVE(2,(#39724,#39725,#39726),.UNSPECIFIED.,.F.,.F.)
B_SPLINE_CURVE_WITH_KNOTS((3,3),(-1.00314154055692,-0.616335277725119),
 .UNSPECIFIED.)
CURVE()
GEOMETRIC_REPRESENTATION_ITEM()
RATIONAL_B_SPLINE_CURVE((1.93380011269323,1.93380011269323,1.79495951130777))
REPRESENTATION_ITEM('')
);
#93=(
BOUNDED_CURVE()
B_SPLINE_CURVE(2,(#39729,#39730,#39731),.UNSPECIFIED.,.F.,.F.)
B_SPLINE_CURVE_WITH_KNOTS((3,3),(-1.38994780338873,-1.00314154055692),
 .UNSPECIFIED.)
CURVE()
GEOMETRIC_REPRESENTATION_ITEM()
RATIONAL_B_SPLINE_CURVE((1.79495951130777,1.93380011269323,1.93380011269323))
REPRESENTATION_ITEM('')
);
#94=(
BOUNDED_CURVE()
B_SPLINE_CURVE(2,(#39732,#39733,#39734),.UNSPECIFIED.,.F.,.F.)
B_SPLINE_CURVE_WITH_KNOTS((3,3),(-1.16547770853232,-0.73666575551116),
 .UNSPECIFIED.)
CURVE()
GEOMETRIC_REPRESENTATION_ITEM()
RATIONAL_B_SPLINE_CURVE((2.12933659022723,2.12933659022723,1.97645710138758))
REPRESENTATION_ITEM('')
);
#95=(
BOUNDED_CURVE()
B_SPLINE_CURVE(2,(#39737,#39738,#39739),.UNSPECIFIED.,.F.,.F.)
B_SPLINE_CURVE_WITH_KNOTS((3,3),(-1.56670140223628,-1.14357963809553),
 .UNSPECIFIED.)
CURVE()
GEOMETRIC_REPRESENTATION_ITEM()
RATIONAL_B_SPLINE_CURVE((1.95186646604709,2.10284386262275,2.10284386262275))
REPRESENTATION_ITEM('')
);
#96=(
BOUNDED_CURVE()
B_SPLINE_CURVE(2,(#39740,#39741,#39742),.UNSPECIFIED.,.F.,.F.)
B_SPLINE_CURVE_WITH_KNOTS((3,3),(-1.09872453323964,-0.687236958819027),
 .UNSPECIFIED.)
CURVE()
GEOMETRIC_REPRESENTATION_ITEM()
RATIONAL_B_SPLINE_CURVE((2.04868118794568,2.04868118794568,1.90159249645282))
REPRESENTATION_ITEM('')
);
#97=(
BOUNDED_CURVE()
B_SPLINE_CURVE(2,(#39745,#39746,#39747),.UNSPECIFIED.,.F.,.F.)
B_SPLINE_CURVE_WITH_KNOTS((3,3),(-1.56670140224009,-1.14357963809856),
 .UNSPECIFIED.)
CURVE()
GEOMETRIC_REPRESENTATION_ITEM()
RATIONAL_B_SPLINE_CURVE((1.9518664660505,2.10284386262641,2.10284386262641))
REPRESENTATION_ITEM('')
);
#98=(
BOUNDED_CURVE()
B_SPLINE_CURVE(2,(#39748,#39749,#39750),.UNSPECIFIED.,.F.,.F.)
B_SPLINE_CURVE_WITH_KNOTS((3,3),(-1.10777980342349,-0.69394596557458),
 .UNSPECIFIED.)
CURVE()
GEOMETRIC_REPRESENTATION_ITEM()
RATIONAL_B_SPLINE_CURVE((2.05960365436383,2.05960365436383,1.91173076506448))
REPRESENTATION_ITEM('')
);
#99=(
BOUNDED_CURVE()
B_SPLINE_CURVE(2,(#39753,#39754,#39755),.UNSPECIFIED.,.F.,.F.)
B_SPLINE_CURVE_WITH_KNOTS((3,3),(-1.40141169651805,-1.01225852375907),
 .UNSPECIFIED.)
CURVE()
GEOMETRIC_REPRESENTATION_ITEM()
RATIONAL_B_SPLINE_CURVE((1.80509777991977,1.94472257911162,1.94472257911162))
REPRESENTATION_ITEM('')
);
#100=(
BOUNDED_CURVE()
B_SPLINE_CURVE(2,(#39756,#39757,#39758),.UNSPECIFIED.,.F.,.F.)
B_SPLINE_CURVE_WITH_KNOTS((3,3),(-1.16547770853319,-0.736665755511809),
 .UNSPECIFIED.)
CURVE()
GEOMETRIC_REPRESENTATION_ITEM()
RATIONAL_B_SPLINE_CURVE((2.12933659022829,2.12933659022829,1.97645710138856))
REPRESENTATION_ITEM('')
);
#101=(
BOUNDED_CURVE()
B_SPLINE_CURVE(2,(#39761,#39762,#39763),.UNSPECIFIED.,.F.,.F.)
B_SPLINE_CURVE_WITH_KNOTS((3,3),(-1.40141169651807,-1.01225852375909),
 .UNSPECIFIED.)
CURVE()
GEOMETRIC_REPRESENTATION_ITEM()
RATIONAL_B_SPLINE_CURVE((1.80509777991979,1.94472257911164,1.94472257911164))
REPRESENTATION_ITEM('')
);
#102=(
BOUNDED_CURVE()
B_SPLINE_CURVE(2,(#39764,#39765,#39766),.UNSPECIFIED.,.F.,.F.)
B_SPLINE_CURVE_WITH_KNOTS((3,3),(-1.01225852375907,-0.623105351000092),
 .UNSPECIFIED.)
CURVE()
GEOMETRIC_REPRESENTATION_ITEM()
RATIONAL_B_SPLINE_CURVE((1.94472257911162,1.94472257911162,1.80509777991977))
REPRESENTATION_ITEM('')
);
#103=(
BOUNDED_CURVE()
B_SPLINE_CURVE(2,(#39769,#39770,#39771),.UNSPECIFIED.,.F.,.F.)
B_SPLINE_CURVE_WITH_KNOTS((3,3),(-1.59428966155458,-1.16547770853319),
 .UNSPECIFIED.)
CURVE()
GEOMETRIC_REPRESENTATION_ITEM()
RATIONAL_B_SPLINE_CURVE((1.97645710138856,2.12933659022828,2.12933659022828))
REPRESENTATION_ITEM('')
);
#104=(
BOUNDED_CURVE()
B_SPLINE_CURVE(2,(#39772,#39773,#39774),.UNSPECIFIED.,.F.,.F.)
B_SPLINE_CURVE_WITH_KNOTS((3,3),(-1.01225852375909,-0.623105351000104),
 .UNSPECIFIED.)
CURVE()
GEOMETRIC_REPRESENTATION_ITEM()
RATIONAL_B_SPLINE_CURVE((1.94472257911164,1.94472257911164,1.80509777991979))
REPRESENTATION_ITEM('')
);
#105=(
BOUNDED_CURVE()
B_SPLINE_CURVE(2,(#39777,#39778,#39779),.UNSPECIFIED.,.F.,.F.)
B_SPLINE_CURVE_WITH_KNOTS((3,3),(-1.52161364127241,-1.1077798034235),
 .UNSPECIFIED.)
CURVE()
GEOMETRIC_REPRESENTATION_ITEM()
RATIONAL_B_SPLINE_CURVE((1.91173076506449,2.05960365436384,2.05960365436384))
REPRESENTATION_ITEM('')
);
#106=(
BOUNDED_CURVE()
B_SPLINE_CURVE(2,(#39780,#39781,#39782),.UNSPECIFIED.,.F.,.F.)
B_SPLINE_CURVE_WITH_KNOTS((3,3),(-1.14357963809856,-0.720457873957025),
 .UNSPECIFIED.)
CURVE()
GEOMETRIC_REPRESENTATION_ITEM()
RATIONAL_B_SPLINE_CURVE((2.10284386262641,2.10284386262641,1.95186646605049))
REPRESENTATION_ITEM('')
);
#107=(
BOUNDED_CURVE()
B_SPLINE_CURVE(2,(#39908,#39909,#39910),.UNSPECIFIED.,.F.,.F.)
B_SPLINE_CURVE_WITH_KNOTS((3,3),(-0.517918190908586,-0.283395256102357),
 .UNSPECIFIED.)
CURVE()
GEOMETRIC_REPRESENTATION_ITEM()
RATIONAL_B_SPLINE_CURVE((1.11558191760503,1.10062774735407,1.07551718013297))
REPRESENTATION_ITEM('')
);
#108=(
BOUNDED_CURVE()
B_SPLINE_CURVE(2,(#39913,#39914,#39915),.UNSPECIFIED.,.F.,.F.)
B_SPLINE_CURVE_WITH_KNOTS((3,3),(-1.44305924653611,-1.2085363117164),
 .UNSPECIFIED.)
CURVE()
GEOMETRIC_REPRESENTATION_ITEM()
RATIONAL_B_SPLINE_CURVE((1.0755171801302,1.10062774735336,1.1155819176052))
REPRESENTATION_ITEM('')
);
#109=B_SPLINE_CURVE_WITH_KNOTS('',3,(#37621,#37622,#37623,#37624,#37625,
#37626,#37627,#37628,#37629,#37630),.UNSPECIFIED.,.F.,.F.,(4,2,2,2,4),(-0.991617660219933,
-0.988360888345703,-0.882558915285875,-0.776756942226048,-0.773500170351817),
 .UNSPECIFIED.);
#110=B_SPLINE_CURVE_WITH_KNOTS('',3,(#37632,#37633,#37634,#37635,#37636,
#37637,#37638,#37639,#37640,#37641),.UNSPECIFIED.,.F.,.F.,(4,2,2,2,4),(-0.991617660219933,
-0.988360888345703,-0.882558915285875,-0.776756942226048,-0.773500170351817),
 .UNSPECIFIED.);
#111=B_SPLINE_CURVE_WITH_KNOTS('',3,(#37643,#37644,#37645,#37646,#37647,
#37648,#37649,#37650,#37651,#37652),.UNSPECIFIED.,.F.,.F.,(4,2,2,2,4),(-0.991617660219934,
-0.988360888345704,-0.882558915285876,-0.776756942226048,-0.773500170351818),
 .UNSPECIFIED.);
#112=B_SPLINE_CURVE_WITH_KNOTS('',3,(#37661,#37662,#37663,#37664,#37665,
#37666,#37667,#37668,#37669,#37670),.UNSPECIFIED.,.F.,.F.,(4,2,2,2,4),(0.773500170351818,
0.776756942226048,0.882558915285876,0.988360888345703,0.991617660219934),
 .UNSPECIFIED.);
#113=B_SPLINE_CURVE_WITH_KNOTS('',3,(#37672,#37673,#37674,#37675,#37676,
#37677,#37678,#37679,#37680,#37681),.UNSPECIFIED.,.F.,.F.,(4,2,2,2,4),(0.773500170351817,
0.776756942226048,0.882558915285875,0.988360888345703,0.991617660219933),
 .UNSPECIFIED.);
#114=B_SPLINE_CURVE_WITH_KNOTS('',3,(#37682,#37683,#37684,#37685,#37686,
#37687,#37688,#37689,#37690,#37691),.UNSPECIFIED.,.F.,.F.,(4,2,2,2,4),(0.773500170351818,
0.776756942226048,0.882558915285876,0.988360888345704,0.991617660219934),
 .UNSPECIFIED.);
#115=B_SPLINE_CURVE_WITH_KNOTS('',3,(#39589,#39590,#39591,#39592,#39593,
#39594,#39595,#39596,#39597,#39598),.UNSPECIFIED.,.F.,.F.,(4,2,2,2,4),(0.112312904835896,
0.113244103065848,0.226488206131697,0.343893756973101,0.461299307814506),
 .UNSPECIFIED.);
#116=B_SPLINE_CURVE_WITH_KNOTS('',3,(#39602,#39603,#39604,#39605,#39606,
#39607,#39608,#39609,#39610,#39611),.UNSPECIFIED.,.F.,.F.,(4,2,2,2,4),(0.461299307814506,
0.57870485865591,0.696110409497315,0.809354512563163,0.810285710793116),
 .UNSPECIFIED.);
#117=B_SPLINE_CURVE_WITH_KNOTS('',3,(#39818,#39819,#39820,#39821,#39822,
#39823,#39824,#39825,#39826,#39827,#39828,#39829,#39830,#39831,#39832,#39833,
#39834,#39835),.UNSPECIFIED.,.F.,.F.,(4,2,2,2,2,2,2,2,4),(0.607760117460578,
0.683747753705319,0.759735389950059,0.835687783070469,0.911640176190879,
0.987592569311288,1.0635449624317,1.13953259867644,1.21552023492118),
 .UNSPECIFIED.);
#118=B_SPLINE_CURVE_WITH_KNOTS('',3,(#39937,#39938,#39939,#39940,#39941,
#39942,#39943,#39944,#39945,#39946,#39947,#39948,#39949,#39950,#39951,#39952,
#39953,#39954,#39955,#39956,#39957,#39958,#39959,#39960,#39961,#39962,#39963,
#39964,#39965,#39966,#39967,#39968,#39969,#39970),.UNSPECIFIED.,.T.,.F.,
(4,2,2,2,2,2,2,2,2,2,2,2,2,2,2,2,4),(0.,0.0926562327783873,0.185312465556775,
0.277968535864378,0.370624606171981,0.463280676479585,0.555936746787188,
0.648592979565575,0.741249212343963,0.83390544512235,0.926561677900738,
1.01921774820834,1.11187381851594,1.20452988882355,1.29718595913115,1.38984219190954,
1.48249842468793),.UNSPECIFIED.);
#119=B_SPLINE_CURVE_WITH_KNOTS('',3,(#39973,#39974,#39975,#39976,#39977,
#39978,#39979,#39980,#39981,#39982,#39983,#39984,#39985,#39986,#39987,#39988,
#39989,#39990,#39991,#39992,#39993,#39994,#39995,#39996,#39997,#39998,#39999,
#40000,#40001,#40002,#40003,#40004,#40005,#40006),.UNSPECIFIED.,.T.,.F.,
(4,2,2,2,2,2,2,2,2,2,2,2,2,2,2,2,4),(0.,0.0930265888637791,0.186053177727558,
0.279067626609053,0.372082075490548,0.465096524372043,0.558110973253538,
0.651137562117317,0.744164150981096,0.837190739844876,0.930217328708655,
1.02323177759015,1.11624622647164,1.20926067535314,1.30227512423463,1.39530171309841,
1.48832830196219),.UNSPECIFIED.);
#120=B_SPLINE_CURVE_WITH_KNOTS('',3,(#40094,#40095,#40096,#40097,#40098,
#40099,#40100,#40101,#40102,#40103),.UNSPECIFIED.,.F.,.F.,(4,2,2,2,4),(-0.786889893332756,
-0.754960430904454,-0.714729481242358,-0.661694768386944,-0.593637938221159),
 .UNSPECIFIED.);
#121=B_SPLINE_CURVE_WITH_KNOTS('',3,(#40106,#40107,#40108,#40109,#40110,
#40111,#40112,#40113,#40114,#40115),.UNSPECIFIED.,.F.,.F.,(4,2,2,2,4),(-0.193251955111595,
-0.125195124945811,-0.0721604120903979,-0.0319294624283026,-2.77555756156289E-17),
 .UNSPECIFIED.);
#122=B_SPLINE_CURVE_WITH_KNOTS('',3,(#40118,#40119,#40120,#40121,#40122,
#40123,#40124,#40125,#40126,#40127),.UNSPECIFIED.,.F.,.F.,(4,2,2,2,4),(-0.193251955111592,
-0.125195124945809,-0.0721604120903967,-0.0319294624283021,0.),
 .UNSPECIFIED.);
#123=B_SPLINE_CURVE_WITH_KNOTS('',3,(#40129,#40130,#40131,#40132,#40133,
#40134,#40135,#40136,#40137,#40138),.UNSPECIFIED.,.F.,.F.,(4,2,2,2,4),(-0.786889893332756,
-0.754960430904454,-0.714729481242359,-0.661694768386946,-0.593637938221162),
 .UNSPECIFIED.);
#124=B_SPLINE_CURVE_WITH_KNOTS('',3,(#40154,#40155,#40156,#40157,#40158,
#40159,#40160,#40161,#40162,#40163),.UNSPECIFIED.,.F.,.F.,(4,2,2,2,4),(-0.193251955111594,
-0.125195124945831,-0.072160412090434,-0.0319294624283508,-5.83144643684363E-14),
 .UNSPECIFIED.);
#125=B_SPLINE_CURVE_WITH_KNOTS('',3,(#40166,#40167,#40168,#40169,#40170,
#40171,#40172,#40173,#40174,#40175),.UNSPECIFIED.,.F.,.F.,(4,2,2,2,4),(-0.786889893332936,
-0.754960430904604,-0.714729481242472,-0.661694768387011,-0.593637938221165),
 .UNSPECIFIED.);
#126=B_SPLINE_CURVE_WITH_KNOTS('',3,(#40178,#40179,#40180,#40181,#40182,
#40183,#40184,#40185,#40186,#40187),.UNSPECIFIED.,.F.,.F.,(4,2,2,2,4),(-0.786889893332757,
-0.754960430904455,-0.71472948124236,-0.661694768386948,-0.593637938221165),
 .UNSPECIFIED.);
#127=B_SPLINE_CURVE_WITH_KNOTS('',3,(#40189,#40190,#40191,#40192,#40193,
#40194,#40195,#40196,#40197,#40198),.UNSPECIFIED.,.F.,.F.,(4,2,2,2,4),(-0.193251955111592,
-0.125195124945673,-0.0721604120901549,-0.0319294624279794,3.86274345842708E-13),
 .UNSPECIFIED.);
#128=B_SPLINE_CURVE_WITH_KNOTS('',3,(#40857,#40858,#40859,#40860,#40861,
#40862,#40863,#40864,#40865,#40866,#40867,#40868,#40869,#40870,#40871,#40872,
#40873,#40874),.UNSPECIFIED.,.F.,.F.,(4,2,2,2,2,2,2,2,4),(-0.905722607976354,
-0.830246578316982,-0.754770548657611,-0.679292810320923,-0.603815071984236,
-0.528337333647548,-0.45285959531086,-0.377383565651489,-0.301907535992118),
 .UNSPECIFIED.);
#129=B_SPLINE_CURVE_WITH_KNOTS('',3,(#40878,#40879,#40880,#40881,#40882,
#40883,#40884,#40885,#40886,#40887,#40888,#40889,#40890,#40891,#40892,#40893,
#40894,#40895,#40896),.UNSPECIFIED.,.F.,.F.,(4,2,2,2,3,2,2,2,4),(-0.301907535992118,
-0.226431506332747,-0.150955476673376,-0.0754777383366878,0.,0.0754777383366878,
0.150955476673376,0.226431506332747,0.301907535992118),.UNSPECIFIED.);
#130=B_SPLINE_CURVE_WITH_KNOTS('',3,(#40901,#40902,#40903,#40904,#40905,
#40906,#40907,#40908,#40909,#40910,#40911,#40912,#40913,#40914,#40915,#40916,
#40917,#40918),.UNSPECIFIED.,.F.,.F.,(4,2,2,2,2,2,2,2,4),(1.26929433930301,
1.33221818753319,1.39514203576337,1.45914762146349,1.52315320716361,1.58715879286373,
1.65116437856384,1.71408822679403,1.77701207502421),.UNSPECIFIED.);
#131=B_SPLINE_CURVE_WITH_KNOTS('',3,(#40919,#40920,#40921,#40922,#40923,
#40924,#40925,#40926,#40927,#40928,#40929,#40930,#40931,#40932,#40933,#40934,
#40935,#40936,#40937),.UNSPECIFIED.,.F.,.F.,(4,2,2,2,3,2,2,2,4),(0.761576603581804,
0.824500451811986,0.887424300042168,0.951429885742286,1.0154354714424,1.07944105714252,
1.14344664284264,1.20637049107282,1.26929433930301),.UNSPECIFIED.);
#132=B_SPLINE_CURVE_WITH_KNOTS('',3,(#40950,#40951,#40952,#40953,#40954,
#40955,#40956,#40957,#40958,#40959,#40960,#40961,#40962,#40963,#40964,#40965,
#40966,#40967),.UNSPECIFIED.,.F.,.F.,(4,2,2,2,2,2,2,2,4),(0.303203013616562,
0.378994323042483,0.454785632468405,0.530595829850764,0.606406027233124,
0.682216224615484,0.758026421997844,0.833817731423765,0.909609040849686),
 .UNSPECIFIED.);
#133=B_SPLINE_CURVE_WITH_KNOTS('',3,(#40968,#40969,#40970,#40971,#40972,
#40973,#40974,#40975,#40976,#40977,#40978,#40979,#40980,#40981,#40982,#40983,
#40984,#40985,#40986),.UNSPECIFIED.,.F.,.F.,(4,2,2,2,3,2,2,2,4),(-0.303203013616562,
-0.227411704190641,-0.151620394764719,-0.0758101973823597,0.,0.0758101973823597,
0.151620394764719,0.227411704190641,0.303203013616562),.UNSPECIFIED.);
#134=B_SPLINE_CURVE_WITH_KNOTS('',3,(#41289,#41290,#41291,#41292,#41293,
#41294,#41295,#41296,#41297,#41298,#41299,#41300,#41301,#41302,#41303,#41304,
#41305,#41306,#41307,#41308,#41309,#41310,#41311,#41312,#41313),
 .UNSPECIFIED.,.F.,.F.,(4,3,3,3,3,3,3,3,4),(9.24769724780462E-8,0.181995241036136,
0.253432963792377,0.436116740020438,0.5,0.680286934730948,0.806407517387765,
0.983702854489084,0.999931275933686),.UNSPECIFIED.);
#135=B_SPLINE_CURVE_WITH_KNOTS('',3,(#41315,#41316,#41317,#41318,#41319,
#41320,#41321,#41322),.UNSPECIFIED.,.F.,.F.,(4,2,2,4),(-0.00419299133317873,
0.,0.077185673586945,0.146698242999108),.UNSPECIFIED.);
#136=B_SPLINE_CURVE_WITH_KNOTS('',3,(#41323,#41324,#41325,#41326,#41327,
#41328,#41329,#41330,#41331,#41332,#41333,#41334,#41335,#41336,#41337,#41338,
#41339,#41340,#41341,#41342,#41343,#41344,#41345,#41346,#41347,#41348,#41349,
#41350,#41351,#41352,#41353,#41354,#41355,#41356,#41357,#41358,#41359,#41360,
#41361,#41362,#41363,#41364,#41365,#41366,#41367,#41368,#41369,#41370,#41371,
#41372,#41373,#41374,#41375,#41376,#41377,#41378,#41379,#41380),
 .UNSPECIFIED.,.F.,.F.,(4,3,3,3,3,3,3,3,3,3,3,3,3,3,3,3,3,3,3,4),(4.16556781324293E-6,
0.0545549619977905,0.125044525011968,0.198839838903777,0.203311262230742,
0.250000000000011,0.329872235461808,0.393021743570836,0.437500000000021,
0.468750000000022,0.484375000000022,0.492187500000022,0.498252272700136,
0.500000000000022,0.587854638271154,0.686590869203439,0.758727477162275,
0.861163120425338,0.935778689900579,0.999972466661225),.UNSPECIFIED.);
#137=B_SPLINE_CURVE_WITH_KNOTS('',3,(#41426,#41427,#41428,#41429,#41430,
#41431,#41432,#41433,#41434,#41435,#41436,#41437,#41438,#41439,#41440,#41441,
#41442,#41443,#41444,#41445,#41446,#41447,#41448,#41449,#41450,#41451,#41452,
#41453,#41454,#41455,#41456,#41457,#41458,#41459,#41460,#41461,#41462,#41463,
#41464,#41465,#41466,#41467,#41468,#41469,#41470,#41471,#41472,#41473,#41474,
#41475,#41476,#41477,#41478,#41479,#41480,#41481,#41482,#41483,#41484,#41485,
#41486,#41487,#41488,#41489,#41490,#41491,#41492,#41493,#41494,#41495,#41496,
#41497,#41498),.UNSPECIFIED.,.F.,.F.,(4,3,3,3,3,3,3,3,3,3,3,3,3,3,3,3,3,
3,3,3,3,3,3,3,4),(1.45421582652742E-9,0.0431191288977147,0.0863267801336832,
0.129382372680128,0.1428571428571,0.153643687206596,0.204633364771825,0.255730828842296,
0.2857142857143,0.306392920688462,0.370923133763148,0.4285714285714,0.459411527501898,
0.526892611023658,0.5714285714286,0.61248828595501,0.677675114413515,0.7142857142857,
0.765391735319569,0.819871243515933,0.8571428571429,0.900979351776543,0.918140216543459,
0.961789699495013,0.999999262769871),.UNSPECIFIED.);
#138=B_SPLINE_CURVE_WITH_KNOTS('',3,(#41501,#41502,#41503,#41504,#41505,
#41506,#41507,#41508,#41509,#41510,#41511,#41512,#41513,#41514,#41515,#41516,
#41517,#41518,#41519,#41520,#41521,#41522,#41523,#41524,#41525,#41526,#41527,
#41528,#41529,#41530,#41531,#41532,#41533,#41534,#41535,#41536,#41537,#41538,
#41539,#41540,#41541,#41542,#41543,#41544,#41545,#41546,#41547,#41548,#41549,
#41550,#41551,#41552,#41553,#41554,#41555,#41556,#41557,#41558,#41559,#41560,
#41561,#41562,#41563,#41564,#41565,#41566,#41567,#41568,#41569,#41570,#41571,
#41572,#41573),.UNSPECIFIED.,.F.,.F.,(4,3,3,3,3,3,3,3,3,3,3,3,3,3,3,3,3,
3,3,3,3,3,3,3,4),(0.,0.0558892508712823,0.112669232828285,0.156953133493156,
0.215051931585836,0.249999999999996,0.30931624195629,0.324310166689452,
0.385390344530509,0.437499999999994,0.468749999999994,0.484374999999995,
0.492187499999994,0.498949344576874,0.499999999999994,0.504582992163155,
0.573408026089892,0.641343139258655,0.680145622776148,0.749999999999997,
0.815926535907529,0.847891707736826,0.914669445287438,0.980716713244497,
1.),.UNSPECIFIED.);
#139=B_SPLINE_CURVE_WITH_KNOTS('',3,(#41672,#41673,#41674,#41675,#41676,
#41677,#41678,#41679,#41680,#41681,#41682,#41683,#41684,#41685,#41686,#41687,
#41688,#41689,#41690,#41691,#41692,#41693,#41694,#41695,#41696,#41697,#41698,
#41699,#41700,#41701,#41702,#41703,#41704,#41705,#41706,#41707,#41708,#41709,
#41710,#41711,#41712,#41713,#41714,#41715,#41716,#41717,#41718,#41719,#41720,
#41721,#41722,#41723,#41724,#41725,#41726,#41727,#41728,#41729,#41730,#41731,
#41732,#41733,#41734,#41735,#41736,#41737,#41738,#41739,#41740,#41741,#41742,
#41743,#41744,#41745,#41746,#41747,#41748,#41749,#41750,#41751,#41752,#41753,
#41754,#41755,#41756,#41757,#41758,#41759,#41760,#41761,#41762,#41763,#41764,
#41765,#41766,#41767,#41768,#41769,#41770,#41771,#41772,#41773,#41774,#41775,
#41776,#41777,#41778,#41779,#41780,#41781,#41782,#41783,#41784,#41785,#41786,
#41787,#41788,#41789,#41790,#41791,#41792,#41793,#41794,#41795,#41796,#41797,
#41798,#41799,#41800,#41801,#41802,#41803,#41804,#41805,#41806,#41807,#41808,
#41809,#41810,#41811,#41812,#41813,#41814,#41815,#41816,#41817,#41818,#41819,
#41820,#41821,#41822,#41823,#41824,#41825,#41826,#41827,#41828,#41829,#41830,
#41831,#41832,#41833,#41834,#41835,#41836,#41837),.UNSPECIFIED.,.F.,.F.,
(4,3,3,3,3,3,3,3,3,3,3,3,3,3,3,3,3,3,3,3,3,3,3,3,3,3,3,3,3,3,3,3,3,3,3,
3,3,3,3,3,3,3,3,3,3,3,3,3,3,3,3,3,3,3,3,4),(8.91960532295663E-8,0.0341912247086381,
0.0625000000000045,0.0800358633121934,0.0937500000000066,0.109375000000008,
0.117187500000008,0.121093750000008,0.123046875000008,0.125000000000009,
0.156917166494981,0.187500000000006,0.218750000000004,0.234375000000004,
0.237569461420448,0.242187500000003,0.246093750000003,0.248046875000003,
0.250000000000003,0.29085498421434,0.312500000000001,0.328958102746394,
0.343750000000001,0.359375,0.3671875,0.37109375,0.373046875,0.375,0.425233690755064,
0.437499999999999,0.468749999999999,0.484374999999998,0.492187499999998,
0.496093749999998,0.499999999999998,0.520148610503687,0.572572263765387,
0.616888106029241,0.624999999999998,0.651356261923537,0.678280550361872,
0.687499999999997,0.709145029414828,0.749999999999997,0.781249999999997,
0.789062499999997,0.796874999999997,0.799058374611912,0.812499999999997,
0.858403727307891,0.874999999999998,0.885484813980563,0.932677545234238,
0.980789386086282,0.985729992648815,1.),.UNSPECIFIED.);
#140=B_SPLINE_CURVE_WITH_KNOTS('',3,(#41840,#41841,#41842,#41843,#41844,
#41845,#41846,#41847,#41848,#41849,#41850,#41851,#41852,#41853,#41854,#41855,
#41856,#41857,#41858,#41859,#41860,#41861,#41862,#41863,#41864,#41865,#41866,
#41867,#41868,#41869,#41870,#41871,#41872,#41873,#41874,#41875,#41876,#41877,
#41878,#41879,#41880,#41881,#41882,#41883,#41884,#41885,#41886,#41887,#41888,
#41889,#41890,#41891,#41892,#41893,#41894,#41895,#41896,#41897,#41898,#41899,
#41900,#41901,#41902,#41903,#41904,#41905,#41906,#41907,#41908,#41909,#41910,
#41911,#41912,#41913,#41914,#41915,#41916,#41917,#41918,#41919,#41920,#41921,
#41922,#41923,#41924,#41925,#41926,#41927,#41928,#41929,#41930,#41931,#41932,
#41933,#41934,#41935,#41936,#41937,#41938,#41939,#41940,#41941,#41942,#41943,
#41944,#41945,#41946,#41947,#41948,#41949,#41950,#41951,#41952,#41953,#41954,
#41955,#41956,#41957,#41958,#41959,#41960,#41961,#41962,#41963,#41964,#41965,
#41966,#41967,#41968,#41969,#41970,#41971,#41972,#41973,#41974,#41975,#41976,
#41977,#41978,#41979,#41980,#41981),.UNSPECIFIED.,.F.,.F.,(4,3,3,3,3,3,
3,3,3,3,3,3,3,3,3,3,3,3,3,3,3,3,3,3,3,3,3,3,3,3,3,3,3,3,3,3,3,3,3,3,3,3,
3,3,3,3,3,4),(2.34638080134641E-7,0.0315958273278338,0.0628964684736565,
0.0937122522464384,0.104172084247666,0.125000000000001,0.15483717259373,
0.184674345187458,0.213175665860292,0.218750000000002,0.234375000000002,
0.242187500000002,0.246093750000002,0.248046875000002,0.250000000000002,
0.257790219373145,0.29564225982583,0.334483268009838,0.354335017264441,
0.392683323993403,0.431399052907306,0.470482126073725,0.482380370753286,
0.484375,0.496585862215116,0.5,0.540377620125422,0.580372331205939,0.609458164571178,
0.649168975008536,0.687499999999999,0.700833597540945,0.718749999999998,
0.734374999999998,0.742187499999998,0.746093749999998,0.748046874999998,
0.749999999999998,0.769092149884525,0.798967231624578,0.82884231336463,
0.858577220360793,0.874999999999999,0.896782429934653,0.927914366070493,
0.95958256675185,0.98564178257925,1.),.UNSPECIFIED.);
#141=B_SPLINE_CURVE_WITH_KNOTS('',3,(#42018,#42019,#42020,#42021,#42022,
#42023,#42024,#42025,#42026,#42027,#42028,#42029,#42030,#42031,#42032,#42033,
#42034,#42035,#42036,#42037,#42038,#42039,#42040,#42041,#42042,#42043,#42044,
#42045,#42046,#42047,#42048,#42049,#42050,#42051,#42052,#42053,#42054,#42055,
#42056,#42057,#42058,#42059,#42060,#42061,#42062,#42063,#42064,#42065,#42066,
#42067,#42068,#42069,#42070,#42071,#42072,#42073,#42074,#42075,#42076,#42077,
#42078),.UNSPECIFIED.,.F.,.F.,(4,3,3,3,3,3,3,3,3,3,3,3,3,3,3,3,3,3,3,3,
4),(3.81437103769371E-8,0.0594692300663259,0.119461345109324,0.180335245486518,
0.228233348289148,0.249999999999999,0.312499999999999,0.375,0.420629724919854,
0.466480844646722,0.5,0.532982688237145,0.595584389353294,0.657507323728288,
0.718468634500906,0.75,0.809830753855516,0.831293930438418,0.890887175430362,
0.949594406087391,1.),.UNSPECIFIED.);
#142=B_SPLINE_CURVE_WITH_KNOTS('',3,(#42079,#42080,#42081,#42082,#42083,
#42084,#42085,#42086,#42087,#42088,#42089,#42090,#42091,#42092,#42093,#42094,
#42095,#42096,#42097,#42098,#42099,#42100,#42101,#42102,#42103,#42104,#42105,
#42106,#42107,#42108,#42109,#42110,#42111,#42112,#42113,#42114,#42115,#42116,
#42117,#42118,#42119,#42120,#42121,#42122,#42123,#42124,#42125,#42126,#42127,
#42128,#42129,#42130,#42131,#42132,#42133,#42134,#42135,#42136),
 .UNSPECIFIED.,.F.,.F.,(4,3,3,3,3,3,3,3,3,3,3,3,3,3,3,3,3,3,3,4),(0.,0.0702349095256629,
0.13620442752083,0.197545800075418,0.25,0.30836677615071,0.365838196629605,
0.422901067133475,0.479527712569993,0.5,0.500089402413344,0.55569689606091,
0.61174830735272,0.66815419823378,0.725240325901832,0.75,0.8125,0.876775284237813,
0.947108494211004,1.),.UNSPECIFIED.);
#143=B_SPLINE_CURVE_WITH_KNOTS('',3,(#42182,#42183,#42184,#42185,#42186,
#42187,#42188,#42189,#42190,#42191,#42192,#42193,#42194,#42195,#42196,#42197,
#42198,#42199,#42200,#42201,#42202,#42203,#42204,#42205,#42206,#42207,#42208,
#42209,#42210,#42211,#42212,#42213,#42214,#42215,#42216,#42217,#42218,#42219,
#42220,#42221,#42222,#42223,#42224,#42225,#42226,#42227,#42228,#42229,#42230,
#42231,#42232,#42233,#42234,#42235,#42236,#42237,#42238,#42239),
 .UNSPECIFIED.,.F.,.F.,(4,3,3,3,3,3,3,3,3,3,3,3,3,3,3,3,3,3,3,4),(0.,0.0625,
0.123429278282135,0.183419387197853,0.242355422377173,0.25,0.30804097321092,
0.365338384048261,0.422299346255784,0.479067052552964,0.535783677854112,
0.592776690073264,0.649990216849972,0.707861099650818,0.75,0.80890331665661,
0.86915409584812,0.930297294952518,0.992906805699324,1.),.UNSPECIFIED.);
#144=B_SPLINE_CURVE_WITH_KNOTS('',3,(#42240,#42241,#42242,#42243,#42244,
#42245,#42246,#42247,#42248,#42249,#42250,#42251,#42252,#42253,#42254,#42255,
#42256,#42257,#42258,#42259,#42260,#42261,#42262,#42263,#42264,#42265,#42266,
#42267,#42268,#42269,#42270,#42271,#42272,#42273,#42274,#42275,#42276,#42277,
#42278,#42279,#42280,#42281,#42282,#42283,#42284,#42285,#42286,#42287,#42288,
#42289,#42290,#42291,#42292,#42293,#42294,#42295,#42296,#42297,#42298,#42299,
#42300,#42301,#42302,#42303,#42304,#42305,#42306,#42307,#42308,#42309,#42310,
#42311,#42312,#42313,#42314,#42315,#42316,#42317,#42318,#42319,#42320,#42321,
#42322,#42323,#42324,#42325,#42326,#42327,#42328,#42329,#42330,#42331,#42332,
#42333,#42334,#42335,#42336),.UNSPECIFIED.,.F.,.F.,(4,3,3,3,3,3,3,3,3,3,
3,3,3,3,3,3,3,3,3,3,3,3,3,3,3,3,3,3,3,3,3,3,4),(0.,0.00532220101307443,
0.0890067021312148,0.125000000000003,0.164995757695198,0.187500000000004,
0.218750000000005,0.234375000000005,0.242187500000005,0.246093750000005,
0.248046875000005,0.250000000000005,0.31582733556036,0.332758332189703,
0.397828850996205,0.462484106543816,0.499894434528747,0.500000000000007,
0.564413907449876,0.625000000000007,0.667038424876444,0.687500000000008,
0.718750000000008,0.734375000000008,0.742187500000008,0.746093750000008,
0.748046875000008,0.750000000000008,0.83044354525046,0.834793539095448,
0.91763781052554,0.994492135647195,1.),.UNSPECIFIED.);
#145=B_SPLINE_CURVE_WITH_KNOTS('',3,(#42379,#42380,#42381,#42382,#42383,
#42384,#42385,#42386,#42387,#42388,#42389,#42390,#42391,#42392,#42393,#42394,
#42395,#42396,#42397,#42398,#42399,#42400,#42401,#42402,#42403,#42404,#42405,
#42406,#42407,#42408,#42409),.UNSPECIFIED.,.F.,.F.,(4,3,3,3,3,3,3,3,3,3,
4),(0.,0.125,0.1875,0.218749999999999,0.234374999999999,0.2421875,0.250000000000002,
0.375000000000002,0.500000000000003,0.750000000000001,1.),.UNSPECIFIED.);
#146=B_SPLINE_CURVE_WITH_KNOTS('',3,(#42410,#42411,#42412,#42413,#42414,
#42415,#42416,#42417,#42418,#42419,#42420,#42421,#42422,#42423,#42424,#42425,
#42426,#42427,#42428,#42429,#42430,#42431,#42432,#42433,#42434),
 .UNSPECIFIED.,.F.,.F.,(4,3,3,3,3,3,3,3,4),(0.,0.177267179225085,0.212270675218487,
0.392511246506684,0.5,0.6825796579365,0.768811549889082,0.950690004118258,
0.999999216908986),.UNSPECIFIED.);
#147=B_SPLINE_CURVE_WITH_KNOTS('',3,(#42435,#42436,#42437,#42438,#42439,
#42440,#42441,#42442,#42443,#42444,#42445,#42446,#42447,#42448,#42449,#42450,
#42451,#42452,#42453,#42454,#42455,#42456,#42457,#42458,#42459,#42460,#42461,
#42462,#42463,#42464,#42465,#42466,#42467,#42468,#42469,#42470,#42471,#42472,
#42473,#42474,#42475,#42476,#42477,#42478,#42479,#42480,#42481,#42482,#42483,
#42484,#42485,#42486,#42487,#42488,#42489,#42490,#42491,#42492,#42493,#42494,
#42495),.UNSPECIFIED.,.F.,.F.,(4,3,3,3,3,3,3,3,3,3,3,3,3,3,3,3,3,3,3,3,
4),(1.62994004756316E-10,0.0701192575230677,0.172402183913519,0.247519373739165,
0.250000000000014,0.348340704489105,0.418430075331828,0.437500000000026,
0.468750000000027,0.484375000000028,0.492187500000028,0.497906193415308,
0.500000000000029,0.583530827624541,0.615517371368563,0.695249493382949,
0.750000000000014,0.803653832952724,0.877332170663887,0.95101050837505,
0.999999999995795),.UNSPECIFIED.);
#148=B_SPLINE_CURVE_WITH_KNOTS('',3,(#42538,#42539,#42540,#42541,#42542,
#42543,#42544,#42545,#42546,#42547,#42548,#42549,#42550,#42551,#42552,#42553,
#42554,#42555,#42556,#42557,#42558,#42559,#42560,#42561,#42562,#42563,#42564,
#42565,#42566,#42567,#42568,#42569,#42570,#42571,#42572,#42573,#42574,#42575,
#42576,#42577,#42578,#42579,#42580,#42581,#42582,#42583,#42584,#42585,#42586,
#42587,#42588,#42589,#42590,#42591,#42592,#42593,#42594,#42595,#42596,#42597,
#42598,#42599,#42600,#42601,#42602,#42603,#42604,#42605,#42606,#42607,#42608,
#42609,#42610,#42611,#42612,#42613,#42614,#42615,#42616,#42617,#42618,#42619,
#42620,#42621,#42622,#42623,#42624,#42625,#42626,#42627,#42628),
 .UNSPECIFIED.,.F.,.F.,(4,3,3,3,3,3,3,3,3,3,3,3,3,3,3,3,3,3,3,3,3,3,3,3,
3,3,3,3,3,3,4),(1.98871961878171E-7,0.0470903044064453,0.0950885766096769,
0.109526530581052,0.125000000000003,0.176685447285025,0.187500000000004,
0.195574875474865,0.203125000000005,0.218750000000006,0.250000000000007,
0.270621367580011,0.334103671117463,0.398264749549881,0.430414452825836,
0.437500000000011,0.468750000000012,0.484375000000012,0.492187500000012,
0.498034135032468,0.500000000000012,0.55992471255586,0.600124996024313,
0.65847531809809,0.715889408777046,0.764251055329571,0.821850438300925,
0.878616573497263,0.918179749391936,0.970963256196437,1.),.UNSPECIFIED.);
#149=B_SPLINE_CURVE_WITH_KNOTS('',3,(#42669,#42670,#42671,#42672,#42673,
#42674,#42675,#42676,#42677,#42678,#42679,#42680,#42681,#42682,#42683,#42684,
#42685,#42686,#42687,#42688,#42689,#42690,#42691,#42692,#42693,#42694,#42695,
#42696,#42697,#42698,#42699,#42700,#42701,#42702,#42703,#42704,#42705,#42706,
#42707,#42708,#42709,#42710,#42711,#42712,#42713,#42714,#42715,#42716,#42717,
#42718,#42719,#42720,#42721,#42722,#42723,#42724,#42725,#42726),
 .UNSPECIFIED.,.F.,.F.,(4,3,3,3,3,3,3,3,3,3,3,3,3,3,3,3,3,3,3,4),(0.,0.0625,
0.123439847866003,0.183439966319605,0.242385271483663,0.25,0.308039825256485,
0.365336094435668,0.422295901803994,0.47906242754066,0.535777838573044,
0.59276959415212,0.649981840047596,0.707851458465103,0.75,0.808901973781704,
0.869151463537593,0.930293405763861,0.992901748291823,1.),.UNSPECIFIED.);
#150=B_SPLINE_CURVE_WITH_KNOTS('',3,(#42728,#42729,#42730,#42731,#42732,
#42733,#42734,#42735,#42736,#42737,#42738,#42739,#42740,#42741,#42742,#42743,
#42744,#42745,#42746,#42747,#42748,#42749),.UNSPECIFIED.,.F.,.F.,(4,3,3,
3,3,3,3,4),(1.63034965610995E-6,0.120934083274333,0.310467041637166,0.5,
0.679851456363595,0.706412177213256,0.883436908989188,0.99999999999965),
 .UNSPECIFIED.);
#151=B_SPLINE_CURVE_WITH_KNOTS('',3,(#42751,#42752,#42753,#42754,#42755,
#42756,#42757,#42758,#42759,#42760,#42761),.UNSPECIFIED.,.F.,.F.,(4,1,2,
2,2,4),(0.,0.125000000000001,0.187500000000001,0.250000000000001,0.5,1.),
 .UNSPECIFIED.);
#152=B_SPLINE_CURVE_WITH_KNOTS('',3,(#42762,#42763,#42764,#42765,#42766,
#42767,#42768,#42769,#42770,#42771,#42772,#42773,#42774,#42775,#42776,#42777,
#42778,#42779,#42780,#42781,#42782,#42783,#42784,#42785,#42786,#42787,#42788,
#42789,#42790,#42791,#42792,#42793,#42794,#42795,#42796,#42797,#42798,#42799,
#42800,#42801,#42802,#42803,#42804,#42805,#42806,#42807,#42808,#42809,#42810,
#42811,#42812,#42813,#42814,#42815,#42816),.UNSPECIFIED.,.F.,.F.,(4,3,3,
3,3,3,3,3,3,3,3,3,3,3,3,3,3,3,4),(0.,0.0654579176760958,0.124936894080836,
0.195216251626205,0.250000000000005,0.306913806087027,0.375000000000006,
0.437500000000007,0.468750000000008,0.484375000000007,0.492187500000006,
0.498304645828867,0.500000000000006,0.531997326816961,0.633294552820071,
0.713452118082794,0.819819671501897,0.902138566641423,1.),.UNSPECIFIED.);
#153=B_SPLINE_CURVE_WITH_KNOTS('',3,(#42858,#42859,#42860,#42861,#42862,
#42863,#42864,#42865,#42866,#42867,#42868,#42869,#42870,#42871,#42872,#42873,
#42874,#42875,#42876,#42877,#42878,#42879,#42880,#42881,#42882,#42883,#42884,
#42885,#42886,#42887,#42888,#42889,#42890,#42891,#42892,#42893,#42894,#42895,
#42896,#42897,#42898,#42899,#42900,#42901,#42902,#42903,#42904,#42905,#42906,
#42907,#42908,#42909,#42910,#42911,#42912,#42913,#42914,#42915,#42916,#42917,
#42918,#42919,#42920,#42921,#42922,#42923,#42924,#42925,#42926,#42927,#42928,
#42929,#42930,#42931,#42932,#42933,#42934,#42935,#42936,#42937,#42938,#42939,
#42940,#42941,#42942,#42943,#42944,#42945),.UNSPECIFIED.,.F.,.F.,(4,3,3,
3,3,3,3,3,3,3,3,3,3,3,3,3,3,3,3,3,3,3,3,3,3,3,3,3,3,4),(1.06363783600673E-11,
0.0527820457982438,0.0818205403105205,0.13847230199092,0.195944376723133,
0.235749539973447,0.293011705111073,0.351192940284653,0.399875412946191,
0.437500000000032,0.468750000000034,0.484375000000035,0.492187500000036,
0.496093750000037,0.499508598162751,0.500000000000037,0.565860966296461,
0.629575210849187,0.693959314619374,0.725751295243402,0.78125000000002,
0.790730874186265,0.796875000000019,0.812500000000018,0.869043431531303,
0.875000000000012,0.884835807418444,0.938700912490986,0.993360836141555,
0.999999777750321),.UNSPECIFIED.);
#154=B_SPLINE_CURVE_WITH_KNOTS('',3,(#42948,#42949,#42950,#42951,#42952,
#42953,#42954,#42955,#42956,#42957,#42958,#42959,#42960,#42961,#42962,#42963,
#42964,#42965,#42966,#42967,#42968,#42969,#42970,#42971,#42972,#42973,#42974,
#42975,#42976,#42977,#42978,#42979,#42980,#42981,#42982,#42983,#42984,#42985,
#42986,#42987,#42988,#42989,#42990,#42991,#42992,#42993,#42994,#42995,#42996,
#42997,#42998,#42999,#43000,#43001,#43002,#43003,#43004,#43005),
 .UNSPECIFIED.,.F.,.F.,(4,3,3,3,3,3,3,3,3,3,3,3,3,3,3,3,3,3,3,4),(1.08539660247806E-11,
0.0585629649075452,0.117996402253644,0.168707850187142,0.228541404633181,
0.250000000000001,0.312500000000001,0.375,0.421054239194796,0.467108478389592,
0.5,0.563532901979659,0.626399534598786,0.688223254771881,0.75,0.771768828134012,
0.832605865340398,0.892881427639851,0.952306983535057,0.999999961863696),
 .UNSPECIFIED.);
#155=B_SPLINE_CURVE_WITH_KNOTS('',3,(#43056,#43057,#43058,#43059,#43060,
#43061,#43062,#43063,#43064,#43065,#43066,#43067,#43068,#43069,#43070,#43071,
#43072,#43073,#43074,#43075,#43076,#43077,#43078,#43079,#43080,#43081,#43082,
#43083,#43084,#43085,#43086,#43087,#43088,#43089,#43090,#43091,#43092,#43093,
#43094,#43095,#43096,#43097,#43098,#43099,#43100,#43101,#43102,#43103,#43104,
#43105,#43106,#43107,#43108,#43109,#43110,#43111,#43112,#43113,#43114,#43115,
#43116,#43117,#43118,#43119,#43120,#43121,#43122,#43123,#43124,#43125,#43126,
#43127,#43128,#43129,#43130,#43131,#43132,#43133,#43134,#43135,#43136,#43137,
#43138,#43139,#43140,#43141,#43142,#43143,#43144,#43145,#43146,#43147,#43148,
#43149,#43150,#43151,#43152,#43153,#43154,#43155,#43156,#43157,#43158,#43159,
#43160,#43161,#43162,#43163,#43164,#43165,#43166,#43167,#43168,#43169,#43170,
#43171,#43172,#43173,#43174,#43175,#43176,#43177,#43178,#43179,#43180,#43181,
#43182,#43183,#43184,#43185,#43186,#43187,#43188,#43189,#43190,#43191,#43192,
#43193,#43194,#43195,#43196,#43197,#43198,#43199,#43200,#43201,#43202,#43203,
#43204,#43205,#43206,#43207,#43208,#43209,#43210,#43211,#43212,#43213,#43214,
#43215,#43216,#43217,#43218,#43219,#43220,#43221,#43222,#43223,#43224,#43225,
#43226,#43227,#43228,#43229,#43230,#43231,#43232,#43233,#43234,#43235,#43236,
#43237,#43238,#43239,#43240,#43241,#43242,#43243,#43244,#43245,#43246,#43247,
#43248,#43249,#43250,#43251,#43252,#43253,#43254,#43255,#43256,#43257,#43258,
#43259,#43260,#43261,#43262,#43263,#43264,#43265,#43266,#43267,#43268,#43269),
 .UNSPECIFIED.,.F.,.F.,(4,3,3,3,3,3,3,3,3,3,3,3,3,3,3,3,3,3,3,3,3,3,3,3,
3,3,3,3,3,3,3,3,3,3,3,3,3,3,3,3,3,3,3,3,3,3,3,3,3,3,3,3,3,3,3,3,3,3,3,3,
3,3,3,3,3,3,3,3,3,3,3,4),(1.2412779566191E-7,0.0158915622078175,0.0300286939597752,
0.0432212519303281,0.0555779177000604,0.0624999999999985,0.0703124999999984,
0.0712890624999984,0.0722656249999983,0.0742187499999983,0.0781249999999982,
0.0928060999306038,0.0937499999999979,0.107515814939851,0.109374999999998,
0.117187499999998,0.121093749999997,0.123046874999997,0.124023437499998,
0.124999999999998,0.14566277553096,0.156249999999996,0.171874999999996,
0.179687499999995,0.186597992196647,0.187499999999995,0.218749999999993,
0.234374999999993,0.242187499999992,0.249023437499992,0.249999999999992,
0.273932641657877,0.297753405180433,0.312499999999987,0.336671055421645,
0.343749999999985,0.359374999999983,0.367187499999983,0.371093749999982,
0.373046874999982,0.374023437499982,0.374999999999982,0.40243511856254,
0.437499999999977,0.468749999999975,0.484374999999973,0.492187499999973,
0.496093749999972,0.498046874999972,0.499023437499972,0.499511718749972,
0.499999999999972,0.531460035353748,0.563796477714746,0.598894275607205,
0.624999999999975,0.661169639291458,0.687499999999976,0.712240746432469,
0.718749999999977,0.734374999999977,0.742187499999977,0.746093749999978,
0.748046874999978,0.749023437499978,0.749999999999978,0.795746766320124,
0.840593249693797,0.884608194904253,0.928337958215087,0.971865961827789,
1.),.UNSPECIFIED.);
#156=B_SPLINE_CURVE_WITH_KNOTS('',3,(#43352,#43353,#43354,#43355,#43356,
#43357,#43358,#43359,#43360,#43361,#43362,#43363,#43364,#43365,#43366,#43367,
#43368,#43369,#43370,#43371,#43372,#43373,#43374,#43375,#43376,#43377,#43378,
#43379,#43380,#43381,#43382,#43383,#43384,#43385,#43386,#43387,#43388,#43389,
#43390,#43391,#43392,#43393,#43394,#43395,#43396,#43397,#43398,#43399,#43400,
#43401,#43402,#43403,#43404,#43405,#43406,#43407,#43408,#43409,#43410,#43411,
#43412,#43413,#43414,#43415,#43416,#43417,#43418,#43419,#43420,#43421,#43422,
#43423,#43424,#43425,#43426,#43427,#43428,#43429,#43430,#43431,#43432,#43433,
#43434,#43435,#43436,#43437,#43438,#43439,#43440,#43441,#43442,#43443,#43444,
#43445,#43446,#43447,#43448,#43449,#43450,#43451,#43452,#43453,#43454,#43455,
#43456,#43457,#43458,#43459,#43460,#43461,#43462,#43463,#43464,#43465,#43466,
#43467,#43468,#43469,#43470,#43471,#43472,#43473,#43474,#43475,#43476,#43477,
#43478,#43479,#43480,#43481,#43482,#43483,#43484,#43485,#43486,#43487,#43488,
#43489,#43490,#43491,#43492,#43493,#43494,#43495,#43496,#43497,#43498,#43499,
#43500,#43501,#43502,#43503,#43504,#43505,#43506,#43507,#43508),
 .UNSPECIFIED.,.F.,.F.,(4,3,3,3,3,3,3,3,3,3,3,3,3,3,3,3,3,3,3,3,3,3,3,3,
3,3,3,3,3,3,3,3,3,3,3,3,3,3,3,3,3,3,3,3,3,3,3,3,3,3,3,3,4),(1.72726539323858E-7,
0.0434573072252328,0.0863338334529781,0.0932169511728678,0.125000000000006,
0.165840004054606,0.177273506760352,0.18750000000001,0.218750000000011,
0.234375000000012,0.242187500000012,0.246093750000012,0.249511718750012,
0.250000000000012,0.260113688380183,0.284905128547609,0.309602232522142,
0.312500000000013,0.33693232508302,0.343750000000013,0.359375000000013,
0.359741527395825,0.367187500000013,0.371093750000013,0.373046875000013,
0.374023437500013,0.375000000000013,0.427162056479387,0.437500000000012,
0.446539057397644,0.468750000000012,0.484375000000012,0.492187500000012,
0.499058238757587,0.500000000000012,0.529372232586504,0.59548856329429,
0.601624357332882,0.62500000000001,0.666786326506838,0.68750000000001,0.718750000000009,
0.726754195536815,0.734375000000009,0.746093750000009,0.750000000000009,
0.777564712781969,0.821930060067123,0.864143824382507,0.906141087264632,
0.949726024687935,0.995918324447688,0.999999956001254),.UNSPECIFIED.);
#157=B_SPLINE_CURVE_WITH_KNOTS('',3,(#43553,#43554,#43555,#43556,#43557,
#43558,#43559,#43560,#43561,#43562,#43563,#43564,#43565,#43566,#43567,#43568,
#43569,#43570,#43571,#43572,#43573,#43574,#43575,#43576,#43577,#43578,#43579,
#43580,#43581,#43582,#43583),.UNSPECIFIED.,.F.,.F.,(4,3,3,3,3,3,3,3,3,3,
4),(0.,0.125000000000005,0.187500000000009,0.21875000000001,0.234375000000012,
0.242187500000012,0.250000000000013,0.37500000000001,0.500000000000008,
0.750000000000004,1.),.UNSPECIFIED.);
#158=B_SPLINE_CURVE_WITH_KNOTS('',3,(#43585,#43586,#43587,#43588,#43589,
#43590,#43591,#43592,#43593,#43594,#43595,#43596,#43597,#43598,#43599,#43600,
#43601,#43602,#43603,#43604,#43605,#43606),.UNSPECIFIED.,.F.,.F.,(4,3,3,
3,3,3,3,4),(0.,0.177097286425541,0.275749261875936,0.455644460001368,0.5,
0.682208683855311,0.858274270782353,0.999997472804992),.UNSPECIFIED.);
#159=B_SPLINE_CURVE_WITH_KNOTS('',3,(#43609,#43610,#43611,#43612,#43613,
#43614,#43615,#43616,#43617,#43618,#43619,#43620,#43621,#43622,#43623,#43624,
#43625,#43626,#43627,#43628,#43629,#43630,#43631,#43632,#43633,#43634,#43635,
#43636,#43637,#43638,#43639,#43640,#43641,#43642,#43643,#43644,#43645,#43646,
#43647,#43648,#43649,#43650,#43651,#43652,#43653,#43654,#43655,#43656,#43657,
#43658,#43659,#43660,#43661,#43662,#43663,#43664,#43665,#43666,#43667,#43668,
#43669),.UNSPECIFIED.,.F.,.F.,(4,3,3,3,3,3,3,3,3,3,3,3,3,3,3,3,3,3,3,3,
4),(4.81164541590028E-11,0.0921587474837998,0.199886082229405,0.25000000000007,
0.280572618510311,0.383373795510249,0.437500000000123,0.46235563760934,
0.468750000000132,0.484375000000136,0.492187500000137,0.497992580687344,
0.500000000000139,0.58065428471115,0.656974692236562,0.686606290161625,
0.750000000000069,0.819755783565435,0.869885555531241,0.934942777765621,
1.),.UNSPECIFIED.);
#160=B_SPLINE_CURVE_WITH_KNOTS('',3,(#43714,#43715,#43716,#43717,#43718,
#43719,#43720,#43721,#43722,#43723,#43724,#43725,#43726,#43727,#43728,#43729,
#43730,#43731,#43732,#43733,#43734,#43735,#43736,#43737,#43738,#43739,#43740,
#43741,#43742,#43743,#43744,#43745,#43746,#43747,#43748,#43749,#43750,#43751,
#43752,#43753,#43754,#43755,#43756,#43757,#43758,#43759,#43760,#43761,#43762,
#43763,#43764,#43765,#43766,#43767,#43768,#43769,#43770,#43771,#43772,#43773,
#43774,#43775,#43776,#43777,#43778,#43779,#43780,#43781,#43782,#43783),
 .UNSPECIFIED.,.F.,.F.,(4,3,3,3,3,3,3,3,3,3,3,3,3,3,3,3,3,3,3,3,3,3,3,4),
(0.,0.0436825138500011,0.0764108556936313,0.12024489353654,0.125,0.179962631311872,
0.223835206461935,0.25,0.32005987930766,0.371520384359274,0.375,0.470560141195038,
0.5,0.519394716784299,0.625,0.667284314982272,0.741666952850946,0.75,0.808039667335501,
0.814941774796512,0.875,0.919746522907813,0.962448186336766,0.999999720265828),
 .UNSPECIFIED.);
#161=B_SPLINE_CURVE_WITH_KNOTS('',3,(#43784,#43785,#43786,#43787,#43788,
#43789,#43790,#43791,#43792,#43793,#43794,#43795,#43796,#43797,#43798,#43799,
#43800,#43801,#43802,#43803,#43804,#43805,#43806,#43807,#43808,#43809,#43810,
#43811,#43812,#43813,#43814,#43815,#43816,#43817,#43818,#43819,#43820,#43821,
#43822,#43823,#43824,#43825,#43826,#43827,#43828,#43829,#43830,#43831,#43832,
#43833,#43834,#43835,#43836,#43837,#43838,#43839,#43840,#43841,#43842,#43843,
#43844,#43845,#43846,#43847,#43848,#43849,#43850,#43851,#43852,#43853),
 .UNSPECIFIED.,.F.,.F.,(4,3,3,3,3,3,3,3,3,3,3,3,3,3,3,3,3,3,3,3,3,3,3,4),
(0.,0.0642449794749212,0.129222656061305,0.139648728602552,0.203363627428338,
0.249999999999998,0.300656431288555,0.369078215644276,0.437499999999997,
0.468749999999997,0.469711746121642,0.484374999999997,0.495155037334243,
0.499999999999997,0.563334769370525,0.625630857709008,0.644014771287496,
0.704246977442631,0.749999999999999,0.80787964620637,0.868482376177339,
0.928163403676397,0.961962296535731,0.99999999244352),.UNSPECIFIED.);
#162=B_SPLINE_CURVE_WITH_KNOTS('',3,(#43889,#43890,#43891,#43892,#43893,
#43894,#43895,#43896,#43897,#43898,#43899,#43900,#43901,#43902,#43903,#43904,
#43905,#43906,#43907,#43908,#43909,#43910,#43911,#43912,#43913,#43914,#43915,
#43916,#43917,#43918,#43919,#43920,#43921,#43922,#43923,#43924,#43925,#43926,
#43927,#43928,#43929,#43930,#43931,#43932,#43933,#43934,#43935,#43936,#43937,
#43938,#43939,#43940,#43941,#43942,#43943,#43944,#43945,#43946),
 .UNSPECIFIED.,.F.,.F.,(4,3,3,3,3,3,3,3,3,3,3,3,3,3,3,3,3,3,3,4),(4.71111344520772E-12,
0.0702702444833502,0.136263297817551,0.197619286303806,0.25,0.306673607267195,
0.362575654085062,0.418136880841742,0.473343199707359,0.5,0.500025791695673,
0.555648512148746,0.611709252031375,0.668121083567431,0.725208108345234,
0.75,0.8125,0.876728896060771,0.946991441238258,1.),.UNSPECIFIED.);
#163=B_SPLINE_CURVE_WITH_KNOTS('',3,(#43991,#43992,#43993,#43994,#43995,
#43996,#43997,#43998,#43999,#44000,#44001,#44002,#44003,#44004,#44005,#44006,
#44007,#44008,#44009,#44010,#44011,#44012,#44013,#44014,#44015,#44016,#44017,
#44018,#44019,#44020,#44021,#44022,#44023,#44024,#44025,#44026,#44027,#44028,
#44029,#44030,#44031,#44032,#44033,#44034,#44035,#44036,#44037,#44038,#44039,
#44040,#44041,#44042,#44043,#44044,#44045,#44046,#44047,#44048,#44049,#44050,
#44051,#44052,#44053,#44054,#44055,#44056,#44057,#44058,#44059,#44060,#44061,
#44062,#44063,#44064,#44065,#44066,#44067,#44068,#44069,#44070,#44071,#44072,
#44073,#44074,#44075,#44076,#44077,#44078,#44079,#44080,#44081,#44082,#44083,
#44084,#44085,#44086,#44087),.UNSPECIFIED.,.F.,.F.,(4,3,3,3,3,3,3,3,3,3,
3,3,3,3,3,3,3,3,3,3,3,3,3,3,3,3,3,3,3,3,3,3,4),(0.,0.00594665339781489,
0.0895009799070571,0.125,0.165331914099726,0.1875,0.218750000000001,0.234375000000001,
0.242187500000001,0.246093750000001,0.248046875000001,0.250000000000001,
0.316494860292734,0.33296054544575,0.39869139222638,0.463982918532056,0.499997299161403,
0.499999999999997,0.564240267140175,0.624999999999996,0.667039051318783,
0.687499999999995,0.718749999999995,0.734374999999994,0.742187499999994,
0.746093749999994,0.748046874999994,0.749999999999994,0.830398363043457,
0.834658925664481,0.917512726931569,0.994047937985235,1.),.UNSPECIFIED.);
#164=B_SPLINE_CURVE_WITH_KNOTS('',3,(#44130,#44131,#44132,#44133,#44134,
#44135,#44136,#44137,#44138,#44139,#44140,#44141,#44142,#44143,#44144,#44145,
#44146,#44147,#44148,#44149,#44150,#44151,#44152,#44153,#44154,#44155,#44156,
#44157,#44158,#44159,#44160,#44161,#44162,#44163,#44164,#44165,#44166,#44167,
#44168,#44169,#44170,#44171,#44172,#44173,#44174,#44175,#44176,#44177,#44178,
#44179,#44180,#44181,#44182,#44183,#44184,#44185,#44186,#44187),
 .UNSPECIFIED.,.F.,.F.,(4,3,3,3,3,3,3,3,3,3,3,3,3,3,3,3,3,3,3,4),(2.22959895026036E-11,
0.062500000016722,0.123437489174482,0.18343535644588,0.242378550489876,
0.25,0.308039612199808,0.365335670799369,0.422295269265173,0.47906158737644,
0.535776791619929,0.592768342853833,0.649980384318985,0.707849804328303,
0.75,0.808900802778059,0.869149031444851,0.930289647710724,0.99289660835092,
1.),.UNSPECIFIED.);
#165=B_SPLINE_CURVE_WITH_KNOTS('',3,(#44189,#44190,#44191,#44192,#44193,
#44194,#44195,#44196,#44197,#44198,#44199,#44200,#44201,#44202,#44203,#44204,
#44205,#44206,#44207,#44208,#44209,#44210),.UNSPECIFIED.,.F.,.F.,(4,3,3,
3,3,3,3,4),(1.50414810706118E-6,0.142631091283063,0.3248384812943,0.5,0.679893770870687,
0.7249391298164,0.902038302978679,1.),.UNSPECIFIED.);
#166=B_SPLINE_CURVE_WITH_KNOTS('',3,(#44212,#44213,#44214,#44215,#44216,
#44217,#44218,#44219,#44220,#44221,#44222),.UNSPECIFIED.,.F.,.F.,(4,1,2,
2,2,4),(0.,0.125000000000001,0.187500000000001,0.250000000000002,0.500000000000002,
1.),.UNSPECIFIED.);
#167=B_SPLINE_CURVE_WITH_KNOTS('',3,(#44223,#44224,#44225,#44226,#44227,
#44228,#44229,#44230,#44231,#44232,#44233,#44234,#44235,#44236,#44237,#44238,
#44239,#44240,#44241,#44242,#44243,#44244,#44245,#44246,#44247,#44248,#44249,
#44250,#44251,#44252,#44253,#44254,#44255,#44256,#44257,#44258,#44259,#44260,
#44261,#44262,#44263,#44264,#44265,#44266,#44267,#44268,#44269,#44270,#44271,
#44272,#44273,#44274,#44275,#44276,#44277),.UNSPECIFIED.,.F.,.F.,(4,3,3,
3,3,3,3,3,3,3,3,3,3,3,3,3,3,3,4),(0.,0.0650994509143261,0.130198901828652,
0.199793623724663,0.249999999999971,0.31347395756223,0.374999999999955,
0.437499999999947,0.468749999999944,0.484374999999942,0.492187499999943,
0.498312113079734,0.499999999999943,0.537870474179042,0.639813169747279,
0.719670993878168,0.826636066600404,0.908057815773878,0.999999999950719),
 .UNSPECIFIED.);
#168=B_SPLINE_CURVE_WITH_KNOTS('',3,(#44323,#44324,#44325,#44326,#44327,
#44328,#44329,#44330,#44331,#44332,#44333,#44334,#44335,#44336,#44337,#44338,
#44339,#44340,#44341,#44342,#44343,#44344,#44345,#44346,#44347,#44348,#44349,
#44350,#44351,#44352,#44353,#44354,#44355,#44356,#44357,#44358,#44359,#44360,
#44361,#44362,#44363,#44364,#44365,#44366,#44367,#44368,#44369,#44370,#44371,
#44372,#44373,#44374,#44375,#44376,#44377,#44378,#44379,#44380,#44381,#44382,
#44383,#44384,#44385,#44386,#44387,#44388,#44389,#44390,#44391,#44392,#44393,
#44394,#44395),.UNSPECIFIED.,.F.,.F.,(4,3,3,3,3,3,3,3,3,3,3,3,3,3,3,3,3,
3,3,3,3,3,3,3,4),(1.45412474122944E-9,0.0431191288920647,0.0863267801229386,
0.129382372664879,0.1428571428571,0.153643687206222,0.204633364768752,0.255730828837679,
0.2857142857143,0.30639292068803,0.370923133797652,0.4285714285714,0.459411527501627,
0.526892611231432,0.5714285714286,0.612488285952903,0.677675115314794,0.7142857142857,
0.765391735325212,0.819871244956775,0.8571428571429,0.900979355292703,0.918140216524895,
0.961789700094182,1.),.UNSPECIFIED.);
#169=B_SPLINE_CURVE_WITH_KNOTS('',3,(#44398,#44399,#44400,#44401,#44402,
#44403,#44404,#44405,#44406,#44407,#44408,#44409,#44410,#44411,#44412,#44413,
#44414,#44415,#44416,#44417,#44418,#44419,#44420,#44421,#44422,#44423,#44424,
#44425,#44426,#44427,#44428,#44429,#44430,#44431,#44432,#44433,#44434,#44435,
#44436,#44437,#44438,#44439,#44440,#44441,#44442,#44443,#44444,#44445,#44446,
#44447,#44448,#44449,#44450,#44451,#44452,#44453,#44454,#44455,#44456,#44457,
#44458,#44459,#44460,#44461,#44462,#44463,#44464,#44465,#44466,#44467,#44468,
#44469,#44470),.UNSPECIFIED.,.F.,.F.,(4,3,3,3,3,3,3,3,3,3,3,3,3,3,3,3,3,
3,3,3,3,3,3,3,4),(0.,0.0558892468671691,0.112669224393364,0.156953102315014,
0.215051895881817,0.249999999999986,0.309316236751042,0.32431009672252,
0.38539026908212,0.437499999999976,0.468749999999975,0.484374999999974,
0.492187499999974,0.49894938686157,0.499999999999974,0.504582882651568,
0.573407791512473,0.641342774132795,0.68014561739347,0.749999999999987,
0.815926296753662,0.847891736141458,0.914669262374538,0.980716193528038,
1.),.UNSPECIFIED.);
#170=B_SPLINE_CURVE_WITH_KNOTS('',3,(#44569,#44570,#44571,#44572,#44573,
#44574,#44575,#44576,#44577,#44578,#44579,#44580,#44581,#44582,#44583,#44584,
#44585,#44586,#44587,#44588,#44589,#44590,#44591,#44592,#44593,#44594,#44595,
#44596,#44597,#44598,#44599,#44600,#44601,#44602,#44603,#44604,#44605,#44606,
#44607,#44608,#44609,#44610,#44611,#44612,#44613,#44614,#44615,#44616,#44617,
#44618,#44619,#44620,#44621,#44622,#44623,#44624,#44625,#44626,#44627,#44628,
#44629,#44630,#44631,#44632,#44633,#44634,#44635,#44636,#44637,#44638,#44639,
#44640,#44641,#44642,#44643,#44644,#44645,#44646,#44647,#44648,#44649,#44650,
#44651,#44652,#44653,#44654,#44655,#44656,#44657,#44658,#44659,#44660,#44661,
#44662,#44663,#44664,#44665,#44666,#44667,#44668,#44669,#44670,#44671,#44672,
#44673,#44674,#44675,#44676,#44677,#44678,#44679,#44680,#44681,#44682,#44683,
#44684,#44685,#44686,#44687,#44688,#44689,#44690,#44691,#44692,#44693,#44694,
#44695,#44696,#44697,#44698,#44699,#44700,#44701,#44702,#44703,#44704,#44705,
#44706,#44707,#44708,#44709,#44710,#44711,#44712,#44713,#44714,#44715,#44716,
#44717,#44718,#44719,#44720,#44721,#44722,#44723,#44724,#44725,#44726,#44727,
#44728,#44729,#44730,#44731,#44732,#44733,#44734),.UNSPECIFIED.,.F.,.F.,
(4,3,3,3,3,3,3,3,3,3,3,3,3,3,3,3,3,3,3,3,3,3,3,3,3,3,3,3,3,3,3,3,3,3,3,
3,3,3,3,3,3,3,3,3,3,3,3,3,3,3,3,3,3,3,3,4),(8.91959169339166E-8,0.034191224757925,
0.0624999999999919,0.0800358633020966,0.0937499999999878,0.109374999999986,
0.117187499999985,0.121093749999984,0.123046874999984,0.124999999999984,
0.15691716645829,0.187499999999983,0.218749999999983,0.234374999999983,
0.2375694614058,0.242187499999983,0.246093749999983,0.248046874999983,0.249999999999983,
0.290854984415917,0.312499999999984,0.328958102706763,0.343749999999985,
0.359374999999985,0.367187499999986,0.371093749999986,0.373046874999986,
0.374999999999986,0.425233690794145,0.437499999999987,0.468749999999988,
0.484374999999988,0.492187499999988,0.496093749999988,0.499999999999989,
0.520148610554065,0.572572264461685,0.616888106095276,0.624999999999991,
0.651356262019081,0.678280550572746,0.687499999999993,0.709145029379915,
0.749999999999994,0.781249999999995,0.789062499999995,0.796874999999995,
0.799058374602463,0.812499999999995,0.858403727209328,0.874999999999997,
0.885484813929701,0.932677545181923,0.980789386022011,0.985729992633788,
1.),.UNSPECIFIED.);
#171=B_SPLINE_CURVE_WITH_KNOTS('',3,(#44737,#44738,#44739,#44740,#44741,
#44742,#44743,#44744,#44745,#44746,#44747,#44748,#44749,#44750,#44751,#44752,
#44753,#44754,#44755,#44756,#44757,#44758,#44759,#44760,#44761,#44762,#44763,
#44764,#44765,#44766,#44767,#44768,#44769,#44770,#44771,#44772,#44773,#44774,
#44775,#44776,#44777,#44778,#44779,#44780,#44781,#44782,#44783,#44784,#44785,
#44786,#44787,#44788,#44789,#44790,#44791,#44792,#44793,#44794,#44795,#44796,
#44797,#44798,#44799,#44800,#44801,#44802,#44803,#44804,#44805,#44806,#44807,
#44808,#44809,#44810,#44811,#44812,#44813,#44814,#44815,#44816,#44817,#44818,
#44819,#44820,#44821,#44822,#44823,#44824,#44825,#44826,#44827,#44828,#44829,
#44830,#44831,#44832,#44833,#44834,#44835,#44836,#44837,#44838,#44839,#44840,
#44841,#44842,#44843,#44844,#44845,#44846,#44847,#44848,#44849,#44850,#44851,
#44852,#44853,#44854,#44855,#44856,#44857,#44858,#44859,#44860,#44861,#44862,
#44863,#44864,#44865,#44866,#44867,#44868,#44869,#44870,#44871,#44872,#44873,
#44874,#44875,#44876,#44877,#44878),.UNSPECIFIED.,.F.,.F.,(4,3,3,3,3,3,
3,3,3,3,3,3,3,3,3,3,3,3,3,3,3,3,3,3,3,3,3,3,3,3,3,3,3,3,3,3,3,3,3,3,3,3,
3,3,3,3,3,4),(2.34637977869052E-7,0.0315958280909132,0.0628964699770943,
0.0937122544741528,0.104172082727763,0.124999999999996,0.154837172127899,
0.184674344255801,0.213175665615131,0.218749999999993,0.234374999999993,
0.242187499999993,0.246093749999993,0.248046874999992,0.249999999999992,
0.257790219441197,0.295642260513954,0.33448326935675,0.35433501791698,0.392683325318844,
0.431399054924811,0.47048212880613,0.482380370998591,0.484374999999998,
0.496585862827081,0.499999999999998,0.540377620589275,0.580372332112356,
0.609458164164579,0.649168974998843,0.687500000000002,0.700833597323562,
0.718750000000003,0.734375000000003,0.742187500000004,0.746093750000004,
0.748046875000004,0.750000000000004,0.769092149904531,0.798967231669278,
0.828842313434025,0.858577220457806,0.875000000000002,0.896782430031144,
0.927914366240707,0.959582566990659,0.985641782611402,1.),.UNSPECIFIED.);
#172=B_SPLINE_CURVE_WITH_KNOTS('',3,(#44915,#44916,#44917,#44918,#44919,
#44920,#44921,#44922,#44923,#44924,#44925,#44926,#44927,#44928,#44929,#44930,
#44931,#44932,#44933,#44934,#44935,#44936,#44937,#44938,#44939,#44940,#44941,
#44942,#44943,#44944,#44945,#44946,#44947,#44948,#44949,#44950,#44951,#44952,
#44953,#44954,#44955,#44956,#44957,#44958,#44959,#44960,#44961,#44962,#44963,
#44964,#44965,#44966,#44967,#44968,#44969,#44970,#44971,#44972,#44973,#44974,
#44975),.UNSPECIFIED.,.F.,.F.,(4,3,3,3,3,3,3,3,3,3,3,3,3,3,3,3,3,3,3,3,
4),(3.81436882533441E-8,0.0594692292641814,0.119461343227841,0.180335241910882,
0.228233302192543,0.25,0.3125,0.375,0.420627292107485,0.46647604053592,
0.499999999999999,0.532982596178094,0.595584220707157,0.657507075875902,
0.718468302664308,0.75,0.809830575581488,0.831293958244676,0.890887062348566,
0.949594080453884,1.),.UNSPECIFIED.);
#173=B_SPLINE_CURVE_WITH_KNOTS('',3,(#44976,#44977,#44978,#44979,#44980,
#44981,#44982,#44983,#44984,#44985,#44986,#44987,#44988,#44989,#44990,#44991,
#44992,#44993,#44994,#44995,#44996,#44997,#44998,#44999,#45000,#45001,#45002,
#45003,#45004,#45005,#45006,#45007,#45008,#45009,#45010,#45011,#45012,#45013,
#45014,#45015,#45016,#45017,#45018,#45019,#45020,#45021,#45022,#45023,#45024,
#45025,#45026,#45027,#45028,#45029,#45030,#45031,#45032,#45033),
 .UNSPECIFIED.,.F.,.F.,(4,3,3,3,3,3,3,3,3,3,3,3,3,3,3,3,3,3,3,4),(0.,0.0707847140878596,
0.137148906725362,0.198769341270042,0.25,0.307617645699735,0.364360102685869,
0.4207050229385,0.476620929621341,0.499999807619985,0.5,0.555639372550431,
0.61176570697656,0.668272077500309,0.725497591406648,0.75,0.8125,0.877170019129078,
0.948088467729899,1.),.UNSPECIFIED.);
#174=B_SPLINE_CURVE_WITH_KNOTS('',3,(#45072,#45073,#45074,#45075,#45076,
#45077,#45078,#45079,#45080,#45081,#45082,#45083,#45084,#45085,#45086,#45087,
#45088,#45089,#45090,#45091,#45092,#45093,#45094,#45095,#45096,#45097,#45098,
#45099,#45100,#45101,#45102,#45103,#45104,#45105,#45106,#45107,#45108,#45109,
#45110,#45111,#45112,#45113,#45114,#45115,#45116,#45117,#45118,#45119,#45120,
#45121,#45122,#45123,#45124,#45125,#45126,#45127,#45128,#45129,#45130,#45131,
#45132,#45133,#45134,#45135,#45136,#45137,#45138,#45139,#45140,#45141,#45142,
#45143,#45144,#45145,#45146,#45147,#45148,#45149,#45150,#45151,#45152,#45153),
 .UNSPECIFIED.,.F.,.F.,(4,3,3,3,3,3,3,3,3,3,3,3,3,3,3,3,3,3,3,3,3,3,3,3,
3,3,3,4),(0.,0.0730383845014315,0.124999999999999,0.126434974013761,0.187499999999999,
0.218749999999999,0.234374999999999,0.242187499999999,0.248228963404092,
0.249999999999999,0.312644125642674,0.385286363662978,0.457286745548691,
0.499988468763114,0.499999999999998,0.570610476397242,0.624999999999998,
0.687338261753051,0.687499999999998,0.718749999999998,0.734374999999998,
0.742187499999998,0.748270407592068,0.749999999999998,0.819257343725233,
0.873533773999793,0.945731297648729,1.),.UNSPECIFIED.);
#175=B_SPLINE_CURVE_WITH_KNOTS('',3,(#45192,#45193,#45194,#45195,#45196,
#45197,#45198,#45199,#45200,#45201,#45202,#45203,#45204,#45205,#45206,#45207,
#45208,#45209,#45210,#45211,#45212,#45213,#45214,#45215,#45216,#45217,#45218,
#45219,#45220,#45221,#45222),.UNSPECIFIED.,.F.,.F.,(4,3,3,3,3,3,3,3,3,3,
4),(0.,0.125000000000001,0.187500000000002,0.218750000000002,0.234375000000002,
0.242187500000002,0.250000000000001,0.375000000000001,0.5,0.75,1.),
 .UNSPECIFIED.);
#176=B_SPLINE_CURVE_WITH_KNOTS('',3,(#45223,#45224,#45225,#45226,#45227,
#45228,#45229,#45230,#45231,#45232,#45233,#45234,#45235,#45236,#45237,#45238,
#45239,#45240,#45241,#45242,#45243,#45244),.UNSPECIFIED.,.F.,.F.,(4,3,3,
3,3,3,3,4),(4.84241338254634E-12,0.177024513735652,0.292989133330021,0.472837100420863,
0.5,0.689142380603627,0.878284761207255,0.999997308141097),
 .UNSPECIFIED.);
#177=B_SPLINE_CURVE_WITH_KNOTS('',3,(#45245,#45246,#45247,#45248,#45249,
#45250,#45251,#45252,#45253,#45254,#45255,#45256,#45257,#45258,#45259,#45260,
#45261,#45262,#45263,#45264,#45265,#45266,#45267,#45268,#45269,#45270,#45271,
#45272,#45273,#45274,#45275,#45276,#45277,#45278,#45279,#45280,#45281,#45282,
#45283,#45284,#45285,#45286,#45287,#45288,#45289,#45290,#45291,#45292,#45293,
#45294,#45295,#45296,#45297,#45298,#45299,#45300,#45301,#45302,#45303,#45304,
#45305),.UNSPECIFIED.,.F.,.F.,(4,3,3,3,3,3,3,3,3,3,3,3,3,3,3,3,3,3,3,3,
4),(0.,0.0976856411360946,0.205020683798958,0.250000000000005,0.286357315729757,
0.375000000000006,0.437500000000007,0.467815787221745,0.468750000000008,
0.484375000000009,0.49218750000001,0.497983320418243,0.500000000000011,
0.581183162052572,0.657948135236424,0.692880007830916,0.750000000000006,
0.820238740720444,0.874892108161841,0.940309020316848,0.999999999888383),
 .UNSPECIFIED.);
#178=B_SPLINE_CURVE_WITH_KNOTS('',3,(#45348,#45349,#45350,#45351,#45352,
#45353,#45354,#45355,#45356,#45357,#45358,#45359,#45360,#45361,#45362,#45363,
#45364,#45365,#45366,#45367,#45368,#45369,#45370,#45371,#45372,#45373,#45374,
#45375,#45376,#45377,#45378,#45379,#45380,#45381,#45382,#45383,#45384,#45385,
#45386,#45387,#45388,#45389,#45390,#45391,#45392,#45393,#45394,#45395,#45396,
#45397,#45398,#45399,#45400,#45401,#45402,#45403,#45404,#45405,#45406,#45407,
#45408,#45409,#45410,#45411,#45412,#45413,#45414,#45415,#45416,#45417,#45418,
#45419,#45420,#45421,#45422,#45423,#45424,#45425,#45426,#45427,#45428,#45429,
#45430,#45431,#45432,#45433,#45434,#45435,#45436,#45437,#45438),
 .UNSPECIFIED.,.F.,.F.,(4,3,3,3,3,3,3,3,3,3,3,3,3,3,3,3,3,3,3,3,3,3,3,3,
3,3,3,3,3,3,4),(1.98906711270074E-7,0.0470898341245432,0.0950876494948429,
0.1095264169096,0.125000000000007,0.176684966067105,0.187500000000011,0.195574834408008,
0.203125000000011,0.218750000000012,0.250000000000014,0.27062137095328,
0.33410369741832,0.398264798166895,0.430414456184177,0.437500000000022,
0.468750000000023,0.484375000000023,0.492187500000023,0.498034134485692,
0.500000000000023,0.55992471700438,0.600124993316173,0.658475320026033,
0.715889417182772,0.764251050351263,0.821850438516385,0.878616579115469,
0.918179745628572,0.970963257604969,1.),.UNSPECIFIED.);
#179=B_SPLINE_CURVE_WITH_KNOTS('',3,(#45479,#45480,#45481,#45482,#45483,
#45484,#45485,#45486,#45487,#45488,#45489,#45490,#45491,#45492,#45493,#45494,
#45495,#45496,#45497,#45498,#45499,#45500,#45501,#45502,#45503,#45504,#45505,
#45506,#45507,#45508,#45509,#45510,#45511,#45512,#45513,#45514,#45515,#45516,
#45517,#45518,#45519,#45520,#45521,#45522,#45523,#45524,#45525,#45526,#45527,
#45528,#45529,#45530,#45531,#45532,#45533,#45534,#45535,#45536),
 .UNSPECIFIED.,.F.,.F.,(4,3,3,3,3,3,3,3,3,3,3,3,3,3,3,3,3,3,3,4),(0.,0.0625,
0.123439752661815,0.183439781150676,0.24238500236667,0.25,0.308039822981183,
0.365336089933782,0.422295895259794,0.479062419223563,0.535777828796871,
0.592769583389136,0.649981828485573,0.707851446289196,0.75,0.808901159247775,
0.869149758611648,0.930290761113668,0.992898128268879,0.999999999982197),
 .UNSPECIFIED.);
#180=B_SPLINE_CURVE_WITH_KNOTS('',3,(#45538,#45539,#45540,#45541,#45542,
#45543,#45544,#45545,#45546,#45547,#45548,#45549,#45550,#45551,#45552,#45553,
#45554,#45555,#45556,#45557,#45558,#45559,#45560,#45561,#45562),
 .UNSPECIFIED.,.F.,.F.,(4,3,3,3,3,3,3,3,4),(4.25096523957949E-6,0.113054396572424,
0.286551692876521,0.3333333333333,0.588518474908942,0.6666666666667,0.699795484080798,
0.8687115644679,1.),.UNSPECIFIED.);
#181=B_SPLINE_CURVE_WITH_KNOTS('',3,(#45564,#45565,#45566,#45567,#45568,
#45569,#45570,#45571),.UNSPECIFIED.,.F.,.F.,(4,2,2,4),(-0.13616939866078,
-0.132213942079058,-0.0631200687627756,-1.0304878651527E-6),
 .UNSPECIFIED.);
#182=B_SPLINE_CURVE_WITH_KNOTS('',3,(#45572,#45573,#45574,#45575,#45576,
#45577,#45578,#45579,#45580,#45581,#45582,#45583,#45584,#45585,#45586,#45587,
#45588,#45589,#45590,#45591,#45592,#45593,#45594,#45595,#45596,#45597,#45598,
#45599,#45600,#45601,#45602,#45603,#45604,#45605,#45606,#45607,#45608,#45609,
#45610,#45611,#45612,#45613,#45614,#45615,#45616,#45617,#45618,#45619,#45620,
#45621,#45622,#45623,#45624,#45625,#45626,#45627,#45628,#45629,#45630,#45631,
#45632),.UNSPECIFIED.,.F.,.F.,(4,3,3,3,3,3,3,3,3,3,3,3,3,3,3,3,3,3,3,3,
4),(0.,0.0668222533452538,0.087636582994685,0.15721165197603,0.23020818876474,
0.25000000000003,0.275402007440453,0.35162875929872,0.431503649816666,0.437500000000052,
0.468750000000056,0.484375000000057,0.492187500000057,0.49890918886054,
0.500000000000057,0.504259889031405,0.612227588888961,0.697520590118762,
0.811484576508768,0.895767648762923,1.),.UNSPECIFIED.);
#183=B_SPLINE_CURVE_WITH_KNOTS('',3,(#45674,#45675,#45676,#45677,#45678,
#45679,#45680,#45681,#45682,#45683,#45684,#45685,#45686,#45687,#45688,#45689,
#45690,#45691,#45692,#45693,#45694,#45695,#45696,#45697,#45698,#45699,#45700,
#45701,#45702,#45703,#45704,#45705,#45706,#45707,#45708,#45709,#45710,#45711,
#45712,#45713,#45714,#45715,#45716,#45717,#45718,#45719,#45720,#45721,#45722,
#45723,#45724,#45725,#45726,#45727,#45728,#45729,#45730,#45731,#45732,#45733,
#45734,#45735,#45736,#45737,#45738,#45739,#45740,#45741,#45742,#45743,#45744,
#45745,#45746,#45747,#45748,#45749,#45750,#45751,#45752,#45753,#45754,#45755,
#45756,#45757,#45758,#45759,#45760,#45761),.UNSPECIFIED.,.F.,.F.,(4,3,3,
3,3,3,3,3,3,3,3,3,3,3,3,3,3,3,3,3,3,3,3,3,3,3,3,3,3,4),(0.,0.0527820478293045,
0.0818205404607765,0.138472304327033,0.195944381325339,0.235749541322639,
0.293011700541857,0.351192937824961,0.399875414183099,0.437499999999972,
0.46874999999997,0.484374999999969,0.492187499999969,0.496093749999968,
0.499508598312834,0.499999999999968,0.565860967008055,0.629575216253443,
0.693959324596289,0.725751295992003,0.781249999999986,0.790730946880879,
0.796874999999988,0.812499999999989,0.869044149651082,0.874999999999992,
0.884835922785512,0.938701683102266,0.993362240378366,0.999999777713918),
 .UNSPECIFIED.);
#184=B_SPLINE_CURVE_WITH_KNOTS('',3,(#45764,#45765,#45766,#45767,#45768,
#45769,#45770,#45771,#45772,#45773,#45774,#45775,#45776,#45777,#45778,#45779,
#45780,#45781,#45782,#45783,#45784,#45785,#45786,#45787,#45788,#45789,#45790,
#45791,#45792,#45793,#45794,#45795,#45796,#45797,#45798,#45799,#45800,#45801,
#45802,#45803,#45804,#45805,#45806,#45807,#45808,#45809,#45810,#45811,#45812,
#45813,#45814,#45815,#45816,#45817,#45818,#45819,#45820,#45821),
 .UNSPECIFIED.,.F.,.F.,(4,3,3,3,3,3,3,3,3,3,3,3,3,3,3,3,3,3,3,4),(1.54018677598839E-11,
0.0585628929030956,0.117996269618339,0.168707840865122,0.228541332439228,
0.25,0.3125,0.375,0.421054279485964,0.467108558971928,0.5,0.563532900722117,
0.626399532373606,0.688223252003269,0.75,0.771768860363025,0.832605896968812,
0.892881458907284,0.952307014882936,0.999999961863681),.UNSPECIFIED.);
#185=B_SPLINE_CURVE_WITH_KNOTS('',3,(#45872,#45873,#45874,#45875,#45876,
#45877,#45878,#45879,#45880,#45881,#45882,#45883,#45884,#45885,#45886,#45887,
#45888,#45889,#45890,#45891,#45892,#45893,#45894,#45895,#45896,#45897,#45898,
#45899,#45900,#45901,#45902,#45903,#45904,#45905,#45906,#45907,#45908,#45909,
#45910,#45911,#45912,#45913,#45914,#45915,#45916,#45917,#45918,#45919,#45920,
#45921,#45922,#45923,#45924,#45925,#45926,#45927,#45928,#45929,#45930,#45931,
#45932,#45933,#45934,#45935,#45936,#45937,#45938,#45939,#45940,#45941,#45942,
#45943,#45944,#45945,#45946,#45947,#45948,#45949,#45950,#45951,#45952,#45953,
#45954,#45955,#45956,#45957,#45958,#45959,#45960,#45961,#45962,#45963,#45964,
#45965,#45966,#45967,#45968,#45969,#45970,#45971,#45972,#45973,#45974,#45975,
#45976,#45977,#45978,#45979,#45980,#45981,#45982,#45983,#45984,#45985,#45986,
#45987,#45988,#45989,#45990,#45991,#45992,#45993,#45994,#45995,#45996,#45997,
#45998,#45999,#46000,#46001,#46002,#46003,#46004,#46005,#46006,#46007,#46008,
#46009,#46010,#46011,#46012,#46013,#46014,#46015,#46016,#46017,#46018,#46019,
#46020,#46021,#46022,#46023,#46024,#46025,#46026,#46027,#46028,#46029,#46030,
#46031,#46032,#46033,#46034,#46035,#46036,#46037,#46038,#46039,#46040,#46041,
#46042,#46043,#46044,#46045,#46046,#46047,#46048,#46049,#46050,#46051,#46052,
#46053,#46054,#46055,#46056,#46057,#46058,#46059,#46060,#46061,#46062,#46063,
#46064,#46065,#46066,#46067,#46068,#46069,#46070,#46071,#46072,#46073,#46074,
#46075,#46076,#46077,#46078,#46079,#46080,#46081,#46082,#46083,#46084,#46085),
 .UNSPECIFIED.,.F.,.F.,(4,3,3,3,3,3,3,3,3,3,3,3,3,3,3,3,3,3,3,3,3,3,3,3,
3,3,3,3,3,3,3,3,3,3,3,3,3,3,3,3,3,3,3,3,3,3,3,3,3,3,3,3,3,3,3,3,3,3,3,3,
3,3,3,3,3,3,3,3,3,3,3,4),(1.24128043371927E-7,0.015891562160926,0.0300286940322461,
0.0432212521704566,0.05557791814208,0.0625000000000095,0.0703125000000105,
0.0712890625000107,0.0722656250000108,0.0742187500000111,0.0781250000000118,
0.0928053510640078,0.0937500000000149,0.107516496092903,0.109375000000018,
0.117187500000019,0.12109375000002,0.12304687500002,0.124023437500021,0.125000000000021,
0.145662774835165,0.156250000000027,0.17187500000003,0.179687500000032,
0.186597991532914,0.187500000000034,0.21875000000004,0.234375000000043,
0.242187500000045,0.249023437500046,0.250000000000046,0.273932641896201,
0.297753405674291,0.312500000000052,0.336671055712276,0.343750000000055,
0.359375000000056,0.367187500000057,0.371093750000057,0.373046875000057,
0.374023437500057,0.375000000000057,0.402435118120539,0.437500000000063,
0.468750000000065,0.484375000000066,0.492187500000067,0.496093750000067,
0.498046875000068,0.499023437500068,0.499511718750068,0.500000000000068,
0.531460033117952,0.563796472906449,0.598894267150548,0.625000000000055,
0.661169640469963,0.687500000000049,0.712240745703438,0.718750000000046,
0.734375000000044,0.742187500000043,0.746093750000043,0.748046875000043,
0.749023437500043,0.750000000000043,0.795746761194119,0.840593239925973,
0.884608181145608,0.928337940845234,0.971865941438119,1.),.UNSPECIFIED.);
#186=B_SPLINE_CURVE_WITH_KNOTS('',3,(#46168,#46169,#46170,#46171,#46172,
#46173,#46174,#46175,#46176,#46177,#46178,#46179,#46180,#46181,#46182,#46183,
#46184,#46185,#46186,#46187,#46188,#46189,#46190,#46191,#46192,#46193,#46194,
#46195,#46196,#46197,#46198,#46199,#46200,#46201,#46202,#46203,#46204,#46205,
#46206,#46207,#46208,#46209,#46210,#46211,#46212,#46213,#46214,#46215,#46216,
#46217,#46218,#46219,#46220,#46221,#46222,#46223,#46224,#46225,#46226,#46227,
#46228,#46229,#46230,#46231,#46232,#46233,#46234,#46235,#46236,#46237,#46238,
#46239,#46240,#46241,#46242,#46243,#46244,#46245,#46246,#46247,#46248,#46249,
#46250,#46251,#46252,#46253,#46254,#46255,#46256,#46257,#46258,#46259,#46260,
#46261,#46262,#46263,#46264,#46265,#46266,#46267,#46268,#46269,#46270,#46271,
#46272,#46273,#46274,#46275,#46276,#46277,#46278,#46279,#46280,#46281,#46282,
#46283,#46284,#46285,#46286,#46287,#46288,#46289,#46290,#46291,#46292,#46293,
#46294,#46295,#46296,#46297,#46298,#46299,#46300,#46301,#46302,#46303,#46304,
#46305,#46306,#46307,#46308,#46309,#46310,#46311,#46312,#46313,#46314,#46315,
#46316,#46317,#46318,#46319,#46320,#46321,#46322,#46323,#46324),
 .UNSPECIFIED.,.F.,.F.,(4,3,3,3,3,3,3,3,3,3,3,3,3,3,3,3,3,3,3,3,3,3,3,3,
3,3,3,3,3,3,3,3,3,3,3,3,3,3,3,3,3,3,3,3,3,3,3,3,3,3,3,3,4),(1.72726522874983E-7,
0.0434573072685472,0.0863338335472871,0.0932169511630213,0.12499999999998,
0.165840004073318,0.177273506753014,0.18749999999997,0.218749999999965,
0.234374999999962,0.242187499999961,0.246093749999961,0.24951171874996,
0.24999999999996,0.260113690588123,0.284905125085302,0.309602223495068,
0.312499999999967,0.336932319725918,0.34374999999997,0.359374999999972,
0.359741529143133,0.367187499999972,0.371093749999973,0.373046874999973,
0.374023437499973,0.374999999999973,0.427161963218175,0.437499999999976,
0.446539047580839,0.468749999999977,0.484374999999978,0.492187499999978,
0.49905822671156,0.499999999999979,0.529372232587649,0.595488563256059,
0.601624357332451,0.624999999999984,0.666786326505097,0.687499999999987,
0.718749999999988,0.726754195533532,0.734374999999989,0.746093749999989,
0.74999999999999,0.777564712519763,0.821930059504363,0.864143823680217,
0.906141086582859,0.94972602421565,0.995918324433868,0.999999956010986),
 .UNSPECIFIED.);
#187=B_SPLINE_CURVE_WITH_KNOTS('',3,(#46365,#46366,#46367,#46368,#46369,
#46370,#46371,#46372,#46373,#46374,#46375,#46376,#46377,#46378,#46379,#46380,
#46381,#46382,#46383,#46384,#46385,#46386,#46387,#46388,#46389,#46390,#46391,
#46392,#46393,#46394,#46395),.UNSPECIFIED.,.F.,.F.,(4,3,3,3,3,3,3,3,3,3,
4),(0.,0.125000000000005,0.187500000000008,0.218750000000008,0.234375000000008,
0.242187500000007,0.250000000000007,0.375000000000007,0.500000000000006,
0.750000000000003,1.),.UNSPECIFIED.);
#188=B_SPLINE_CURVE_WITH_KNOTS('',3,(#46397,#46398,#46399,#46400,#46401,
#46402,#46403,#46404,#46405,#46406,#46407,#46408,#46409,#46410,#46411,#46412,
#46413,#46414,#46415,#46416,#46417,#46418,#46419,#46420,#46421),
 .UNSPECIFIED.,.F.,.F.,(4,3,3,3,3,3,3,3,4),(6.00778538742285E-12,0.168745739560462,
0.282139878481535,0.3333333333333,0.590532057928784,0.6666666666667,0.840266058577053,
0.865637391095598,0.999997478430659),.UNSPECIFIED.);
#189=B_SPLINE_CURVE_WITH_KNOTS('',3,(#46424,#46425,#46426,#46427,#46428,
#46429,#46430,#46431,#46432,#46433,#46434,#46435,#46436,#46437,#46438,#46439,
#46440,#46441,#46442,#46443,#46444,#46445,#46446,#46447,#46448,#46449,#46450,
#46451,#46452,#46453,#46454,#46455,#46456,#46457,#46458,#46459,#46460,#46461,
#46462,#46463,#46464,#46465,#46466,#46467,#46468,#46469,#46470,#46471,#46472,
#46473,#46474,#46475,#46476,#46477,#46478,#46479,#46480,#46481,#46482,#46483,
#46484,#46485,#46486,#46487),.UNSPECIFIED.,.F.,.F.,(4,3,3,3,3,3,3,3,3,3,
3,3,3,3,3,3,3,3,3,3,3,4),(0.,0.0982799701893736,0.213482755431675,0.250000000000042,
0.295950559396774,0.375000000000063,0.437500000000075,0.468750000000081,
0.484375000000084,0.488569176919273,0.492187500000084,0.498693625937138,
0.500000000000084,0.581892466489566,0.659367760809361,0.71516477614781,
0.750000000000042,0.822980248697091,0.892544871534579,0.904183472300278,
0.970836803729396,1.),.UNSPECIFIED.);
#190=B_SPLINE_CURVE_WITH_KNOTS('',3,(#46532,#46533,#46534,#46535,#46536,
#46537,#46538,#46539,#46540,#46541,#46542,#46543,#46544,#46545,#46546,#46547,
#46548,#46549,#46550,#46551,#46552,#46553,#46554,#46555,#46556,#46557,#46558,
#46559,#46560,#46561,#46562,#46563,#46564,#46565,#46566,#46567,#46568,#46569,
#46570,#46571,#46572,#46573,#46574,#46575,#46576,#46577,#46578,#46579,#46580,
#46581,#46582,#46583,#46584,#46585,#46586,#46587,#46588,#46589,#46590,#46591,
#46592,#46593,#46594,#46595,#46596,#46597,#46598,#46599,#46600,#46601),
 .UNSPECIFIED.,.F.,.F.,(4,3,3,3,3,3,3,3,3,3,3,3,3,3,3,3,3,3,3,3,3,3,3,4),
(0.,0.0435516393491532,0.076471965080317,0.120148484350007,0.125,0.178495710860988,
0.223908387543282,0.25,0.318709089634349,0.371577560495655,0.375,0.469052171169697,
0.5,0.519438375467887,0.625,0.667314602754769,0.741711825535796,0.75,0.808035501625466,
0.814958553106824,0.875,0.91974261032604,0.962451614850442,0.999999720291478),
 .UNSPECIFIED.);
#191=B_SPLINE_CURVE_WITH_KNOTS('',3,(#46602,#46603,#46604,#46605,#46606,
#46607,#46608,#46609,#46610,#46611,#46612,#46613,#46614,#46615,#46616,#46617,
#46618,#46619,#46620,#46621,#46622,#46623,#46624,#46625,#46626,#46627,#46628,
#46629,#46630,#46631,#46632,#46633,#46634,#46635,#46636,#46637,#46638,#46639,
#46640,#46641,#46642,#46643,#46644,#46645,#46646,#46647,#46648,#46649,#46650,
#46651,#46652,#46653,#46654,#46655,#46656,#46657,#46658,#46659,#46660,#46661,
#46662,#46663,#46664,#46665,#46666,#46667,#46668,#46669,#46670,#46671),
 .UNSPECIFIED.,.F.,.F.,(4,3,3,3,3,3,3,3,3,3,3,3,3,3,3,3,3,3,3,3,3,3,3,4),
(0.,0.0642448454708453,0.129222404838902,0.139648705363206,0.20336349094211,
0.25,0.30065642377295,0.369078211886475,0.437500000000001,0.468750000000001,
0.469711808549797,0.484375000000001,0.495155161137369,0.5,0.563334814263254,
0.625630949976613,0.644014791014155,0.704247046610669,0.75,0.807879635213996,
0.868482419985881,0.928163504115579,0.9619622907836,0.999999992443124),
 .UNSPECIFIED.);
#192=B_SPLINE_CURVE_WITH_KNOTS('',3,(#46707,#46708,#46709,#46710,#46711,
#46712,#46713,#46714,#46715,#46716,#46717,#46718,#46719,#46720,#46721,#46722,
#46723,#46724,#46725,#46726,#46727,#46728,#46729,#46730,#46731,#46732,#46733,
#46734,#46735,#46736,#46737,#46738,#46739,#46740,#46741,#46742,#46743,#46744,
#46745,#46746,#46747,#46748,#46749,#46750,#46751,#46752,#46753,#46754,#46755,
#46756,#46757,#46758,#46759,#46760,#46761,#46762,#46763,#46764),
 .UNSPECIFIED.,.F.,.F.,(4,3,3,3,3,3,3,3,3,3,3,3,3,3,3,3,3,3,3,4),(1.01449595492675E-11,
0.0705966753463834,0.136832386883981,0.198363721951571,0.25,0.306585362611179,
0.362372014726767,0.417803058925887,0.472856063303982,0.499998113896311,
0.5,0.555653427215775,0.611786177000757,0.668294513633687,0.725515077026516,
0.75,0.8125,0.876968707688738,0.94757495842845,1.),.UNSPECIFIED.);
#193=B_SPLINE_CURVE_WITH_KNOTS('',3,(#46801,#46802,#46803,#46804,#46805,
#46806,#46807,#46808,#46809,#46810,#46811,#46812,#46813,#46814,#46815,#46816,
#46817,#46818,#46819,#46820,#46821,#46822,#46823,#46824,#46825,#46826,#46827,
#46828,#46829,#46830,#46831,#46832,#46833,#46834,#46835,#46836,#46837,#46838,
#46839,#46840,#46841,#46842,#46843,#46844,#46845,#46846,#46847,#46848,#46849,
#46850,#46851,#46852,#46853,#46854,#46855,#46856,#46857,#46858,#46859,#46860,
#46861,#46862,#46863,#46864,#46865,#46866,#46867,#46868,#46869,#46870),
 .UNSPECIFIED.,.F.,.F.,(4,3,3,3,3,3,3,3,3,3,3,3,3,3,3,3,3,3,3,3,3,3,3,4),
(0.,0.080844790934893,0.125,0.133450088539653,0.1875,0.21875,0.235735057515083,
0.25,0.318589046603858,0.38951330554323,0.461228032467734,0.5,0.500070526558878,
0.569716537362397,0.625,0.681559788616792,0.6875,0.71875,0.735656425285893,
0.75,0.825645197998783,0.866690726110233,0.943548522664466,1.),
 .UNSPECIFIED.);
#194=B_SPLINE_CURVE_WITH_KNOTS('',3,(#46909,#46910,#46911,#46912,#46913,
#46914,#46915,#46916,#46917,#46918,#46919,#46920,#46921,#46922,#46923,#46924,
#46925,#46926,#46927,#46928,#46929,#46930,#46931,#46932,#46933,#46934,#46935,
#46936,#46937,#46938,#46939,#46940,#46941,#46942,#46943,#46944,#46945,#46946,
#46947,#46948,#46949,#46950,#46951,#46952,#46953,#46954,#46955,#46956,#46957,
#46958,#46959,#46960,#46961,#46962,#46963,#46964,#46965,#46966),
 .UNSPECIFIED.,.F.,.F.,(4,3,3,3,3,3,3,3,3,3,3,3,3,3,3,3,3,3,3,4),(2.82054536219499E-11,
0.0625000000211541,0.123435816746246,0.183432146452882,0.242373947342859,
0.25,0.308039798384561,0.365336042404427,0.422295827820954,0.479062336025,
0.535777734589141,0.592769485322273,0.649981729622503,0.707851349801787,
0.75,0.80890213970272,0.869151808551022,0.93029395044618,0.992902535032498,
1.),.UNSPECIFIED.);
#195=B_SPLINE_CURVE_WITH_KNOTS('',3,(#46968,#46969,#46970,#46971,#46972,
#46973,#46974,#46975,#46976,#46977,#46978,#46979,#46980,#46981,#46982,#46983,
#46984,#46985,#46986,#46987,#46988,#46989,#46990,#46991,#46992),
 .UNSPECIFIED.,.F.,.F.,(4,3,3,3,3,3,3,3,4),(1.26985457340339E-6,0.173312592767027,
0.210273395635445,0.3333333333333,0.613202238647455,0.6666666666667,0.775173469127502,
0.943222799720604,0.999999999999632),.UNSPECIFIED.);
#196=B_SPLINE_CURVE_WITH_KNOTS('',3,(#46994,#46995,#46996,#46997,#46998,
#46999,#47000,#47001,#47002,#47003,#47004,#47005,#47006),.UNSPECIFIED.,
 .F.,.F.,(4,3,3,3,4),(0.,0.187500000000003,0.250000000000004,0.500000000000003,
1.),.UNSPECIFIED.);
#197=B_SPLINE_CURVE_WITH_KNOTS('',3,(#47007,#47008,#47009,#47010,#47011,
#47012,#47013,#47014,#47015,#47016,#47017,#47018,#47019,#47020,#47021,#47022,
#47023,#47024,#47025,#47026,#47027,#47028,#47029,#47030,#47031,#47032,#47033,
#47034,#47035,#47036,#47037,#47038,#47039,#47040,#47041,#47042,#47043,#47044,
#47045,#47046,#47047,#47048,#47049,#47050,#47051,#47052,#47053,#47054,#47055,
#47056,#47057,#47058,#47059,#47060,#47061),.UNSPECIFIED.,.F.,.F.,(4,3,3,
3,3,3,3,3,3,3,3,3,3,3,3,3,3,3,4),(0.,0.0638950390766455,0.126878094455892,
0.195427827297906,0.249999999999974,0.317220939245595,0.392664016611647,
0.437499999999954,0.46874999999995,0.484374999999948,0.492187499999948,
0.498924460179924,0.499999999999948,0.53547877547165,0.642764494845113,
0.725136941874545,0.836917893499071,0.92006383085474,0.999999999858759),
 .UNSPECIFIED.);
#198=B_SPLINE_CURVE_WITH_KNOTS('',3,(#47107,#47108,#47109,#47110,#47111,
#47112,#47113,#47114,#47115,#47116,#47117,#47118,#47119,#47120,#47121,#47122,
#47123,#47124,#47125,#47126,#47127,#47128,#47129,#47130,#47131,#47132,#47133,
#47134,#47135,#47136,#47137,#47138,#47139,#47140,#47141,#47142,#47143,#47144,
#47145,#47146,#47147,#47148,#47149,#47150,#47151,#47152,#47153,#47154,#47155,
#47156,#47157,#47158,#47159,#47160,#47161,#47162,#47163,#47164,#47165,#47166,
#47167,#47168,#47169,#47170,#47171,#47172,#47173,#47174,#47175,#47176,#47177,
#47178,#47179),.UNSPECIFIED.,.F.,.F.,(4,3,3,3,3,3,3,3,3,3,3,3,3,3,3,3,3,
3,3,3,3,3,3,3,4),(1.45401629951061E-9,0.0431123239999773,0.0863131632793753,
0.129361943345478,0.1428571428571,0.153622120796769,0.204599117366318,0.255683865453928,
0.2857142857143,0.306349836570465,0.370801351683843,0.4285714285714,0.459346573254742,
0.526502052474814,0.5714285714286,0.6124033147054,0.676566373102767,0.7142857142857,
0.765276986306117,0.818291690290777,0.8571428571429,0.900814093153431,0.918051250558587,
0.961570051922101,1.),.UNSPECIFIED.);
#199=B_SPLINE_CURVE_WITH_KNOTS('',3,(#47182,#47183,#47184,#47185,#47186,
#47187,#47188,#47189,#47190,#47191,#47192,#47193,#47194,#47195,#47196,#47197,
#47198,#47199,#47200,#47201,#47202,#47203,#47204,#47205,#47206,#47207,#47208,
#47209,#47210,#47211,#47212,#47213,#47214,#47215,#47216,#47217,#47218,#47219,
#47220,#47221,#47222,#47223,#47224,#47225,#47226,#47227,#47228,#47229,#47230,
#47231,#47232,#47233,#47234,#47235,#47236,#47237,#47238,#47239,#47240,#47241,
#47242,#47243,#47244,#47245,#47246,#47247,#47248,#47249,#47250,#47251,#47252,
#47253,#47254),.UNSPECIFIED.,.F.,.F.,(4,3,3,3,3,3,3,3,3,3,3,3,3,3,3,3,3,
3,3,3,3,3,3,3,4),(0.,0.0558892484596122,0.112669228063845,0.156953132120896,
0.215051927917948,0.249999999999994,0.309316239775135,0.324310165349072,
0.385390341081382,0.437499999999991,0.468749999999991,0.484374999999991,
0.49218749999999,0.498949344757548,0.499999999999989,0.504582992961993,
0.573408021618643,0.641343129323671,0.680145625695793,0.749999999999995,
0.815926496427531,0.847891711430229,0.914669420517686,0.980716617979016,
1.),.UNSPECIFIED.);
#200=B_SPLINE_CURVE_WITH_KNOTS('',3,(#47353,#47354,#47355,#47356,#47357,
#47358,#47359,#47360,#47361,#47362,#47363,#47364,#47365,#47366,#47367,#47368,
#47369,#47370,#47371,#47372,#47373,#47374,#47375,#47376,#47377,#47378,#47379,
#47380,#47381,#47382,#47383,#47384,#47385,#47386,#47387,#47388,#47389,#47390,
#47391,#47392,#47393,#47394,#47395,#47396,#47397,#47398,#47399,#47400,#47401,
#47402,#47403,#47404,#47405,#47406,#47407,#47408,#47409,#47410,#47411,#47412,
#47413,#47414,#47415,#47416,#47417,#47418,#47419,#47420,#47421,#47422,#47423,
#47424,#47425,#47426,#47427,#47428,#47429,#47430,#47431,#47432,#47433,#47434,
#47435,#47436,#47437,#47438,#47439,#47440,#47441,#47442,#47443,#47444,#47445,
#47446,#47447,#47448,#47449,#47450,#47451,#47452,#47453,#47454,#47455,#47456,
#47457,#47458,#47459,#47460,#47461,#47462,#47463,#47464,#47465,#47466,#47467,
#47468,#47469,#47470,#47471,#47472,#47473,#47474,#47475,#47476,#47477,#47478,
#47479,#47480,#47481,#47482,#47483,#47484,#47485,#47486,#47487,#47488,#47489,
#47490,#47491,#47492,#47493,#47494,#47495,#47496,#47497,#47498,#47499,#47500,
#47501,#47502,#47503,#47504,#47505,#47506,#47507,#47508,#47509,#47510,#47511,
#47512,#47513,#47514,#47515,#47516,#47517,#47518),.UNSPECIFIED.,.F.,.F.,
(4,3,3,3,3,3,3,3,3,3,3,3,3,3,3,3,3,3,3,3,3,3,3,3,3,3,3,3,3,3,3,3,3,3,3,
3,3,3,3,3,3,3,3,3,3,3,3,3,3,3,3,3,3,3,3,4),(8.91796408023666E-8,0.0341889233158358,
0.0625000000000036,0.0800235801138546,0.0937500000000054,0.109375000000006,
0.117187500000007,0.121093750000007,0.123046875000007,0.125000000000007,
0.156896093638754,0.187500000000008,0.218750000000008,0.234375000000008,
0.237544069792359,0.242187500000008,0.246093750000008,0.248046875000008,
0.250000000000008,0.29085297613211,0.312500000000008,0.328940100260377,
0.343750000000007,0.359375000000007,0.367187500000007,0.371093750000007,
0.373046875000007,0.375000000000007,0.425222667492041,0.437500000000007,
0.468750000000007,0.484375000000007,0.492187500000007,0.496093750000007,
0.500000000000007,0.520152743002406,0.572584842158793,0.616900729702386,
0.625000000000005,0.651342131071929,0.678251292688293,0.687500000000004,
0.709160584351542,0.750000000000004,0.781250000000003,0.789062500000003,
0.796875000000003,0.799072641440133,0.812500000000003,0.858399949290242,
0.875000000000002,0.885492822282815,0.932681905157277,0.980790028010998,
0.985730934543369,1.),.UNSPECIFIED.);
#201=B_SPLINE_CURVE_WITH_KNOTS('',3,(#47521,#47522,#47523,#47524,#47525,
#47526,#47527,#47528,#47529,#47530,#47531,#47532,#47533,#47534,#47535,#47536,
#47537,#47538,#47539,#47540,#47541,#47542,#47543,#47544,#47545,#47546,#47547,
#47548,#47549,#47550,#47551,#47552,#47553,#47554,#47555,#47556,#47557,#47558,
#47559,#47560,#47561,#47562,#47563,#47564,#47565,#47566,#47567,#47568,#47569,
#47570,#47571,#47572,#47573,#47574,#47575,#47576,#47577,#47578,#47579,#47580,
#47581,#47582,#47583,#47584,#47585,#47586,#47587,#47588,#47589,#47590,#47591,
#47592,#47593,#47594,#47595,#47596,#47597,#47598,#47599,#47600,#47601,#47602,
#47603,#47604,#47605,#47606,#47607,#47608,#47609,#47610,#47611,#47612,#47613,
#47614,#47615,#47616,#47617,#47618,#47619,#47620,#47621,#47622,#47623,#47624,
#47625,#47626,#47627,#47628,#47629,#47630,#47631,#47632,#47633,#47634,#47635,
#47636,#47637,#47638,#47639,#47640,#47641,#47642,#47643,#47644,#47645,#47646,
#47647,#47648,#47649,#47650,#47651,#47652,#47653,#47654,#47655,#47656,#47657,
#47658,#47659,#47660,#47661,#47662),.UNSPECIFIED.,.F.,.F.,(4,3,3,3,3,3,
3,3,3,3,3,3,3,3,3,3,3,3,3,3,3,3,3,3,3,3,3,3,3,3,3,3,3,3,3,3,3,3,3,3,3,3,
3,3,3,3,3,4),(2.34638067050473E-7,0.0315958280048414,0.0628964697291262,
0.0937122537280348,0.104172143004049,0.125000000000003,0.154837231687147,
0.184674463374292,0.213175783877095,0.218750000000005,0.234375000000006,
0.242187500000006,0.246093750000006,0.248046875000006,0.250000000000006,
0.257790373821085,0.295642404986771,0.334483401403744,0.354334938901152,
0.392683241215207,0.431398966624688,0.470482034495911,0.482378819653905,
0.484375000000001,0.496585822661942,0.500000000000001,0.540377618734413,
0.580372331510874,0.609456767722748,0.649167581317096,0.687499999999997,
0.700832884820975,0.718749999999996,0.734374999999996,0.742187499999996,
0.746093749999996,0.748046874999996,0.749999999999996,0.76909192808113,
0.798967073993967,0.828842219906804,0.858577127007425,0.874999999999998,
0.896782378211392,0.927914314370241,0.959582515324487,0.985641745354497,
1.),.UNSPECIFIED.);
#202=B_SPLINE_CURVE_WITH_KNOTS('',3,(#47699,#47700,#47701,#47702,#47703,
#47704,#47705,#47706,#47707,#47708,#47709,#47710,#47711,#47712,#47713,#47714,
#47715,#47716,#47717,#47718,#47719,#47720,#47721,#47722,#47723,#47724,#47725,
#47726,#47727,#47728,#47729,#47730,#47731,#47732,#47733,#47734,#47735,#47736,
#47737,#47738,#47739,#47740,#47741,#47742,#47743,#47744,#47745,#47746,#47747,
#47748,#47749,#47750,#47751,#47752,#47753,#47754,#47755,#47756,#47757,#47758,
#47759),.UNSPECIFIED.,.F.,.F.,(4,3,3,3,3,3,3,3,3,3,3,3,3,3,3,3,3,3,3,3,
4),(3.81437099953529E-8,0.0594692301267317,0.11946134523179,0.180335245674018,
0.22823334864808,0.25,0.3125,0.375,0.420629664625766,0.4664807256031,0.5,
0.532982689971054,0.595584386743332,0.657507316660725,0.71846862277759,
0.75,0.809830725006028,0.831293934527991,0.890887161148583,0.949594354583762,
1.),.UNSPECIFIED.);
#203=B_SPLINE_CURVE_WITH_KNOTS('',3,(#47760,#47761,#47762,#47763,#47764,
#47765,#47766,#47767,#47768,#47769,#47770,#47771,#47772,#47773,#47774,#47775,
#47776,#47777,#47778,#47779,#47780,#47781,#47782,#47783,#47784,#47785,#47786,
#47787,#47788,#47789,#47790,#47791,#47792,#47793,#47794,#47795,#47796,#47797,
#47798,#47799,#47800,#47801,#47802,#47803,#47804,#47805,#47806,#47807,#47808,
#47809,#47810,#47811,#47812,#47813,#47814,#47815,#47816,#47817),
 .UNSPECIFIED.,.F.,.F.,(4,3,3,3,3,3,3,3,3,3,3,3,3,3,3,3,3,3,3,4),(0.,0.0701431897639297,
0.13604417473497,0.197334652086801,0.25,0.307833948589721,0.364819438044064,
0.421421997850492,0.477619532142297,0.5,0.500034450215325,0.555641456198574,
0.611685710202809,0.668080534996765,0.725149887541437,0.75,0.8125,0.876721757771727,
0.946972970382545,1.),.UNSPECIFIED.);
#204=B_SPLINE_CURVE_WITH_KNOTS('',3,(#47863,#47864,#47865,#47866,#47867,
#47868,#47869,#47870,#47871,#47872,#47873,#47874,#47875,#47876,#47877,#47878,
#47879,#47880,#47881,#47882,#47883,#47884,#47885,#47886,#47887,#47888,#47889,
#47890,#47891,#47892,#47893,#47894,#47895,#47896,#47897,#47898,#47899,#47900,
#47901,#47902,#47903,#47904,#47905,#47906,#47907,#47908,#47909,#47910,#47911,
#47912,#47913,#47914,#47915,#47916,#47917,#47918,#47919,#47920),
 .UNSPECIFIED.,.F.,.F.,(4,3,3,3,3,3,3,3,3,3,3,3,3,3,3,3,3,3,3,4),(0.,0.0625,
0.123429164348376,0.183419166724562,0.24235510130439,0.25,0.308040960610337,
0.365338359396875,0.422299309833655,0.479067004587782,0.535783618539891,
0.592776619814919,0.649990135834089,0.707861008608383,0.75,0.808903107716075,
0.869153662199582,0.930296626253199,0.992905895259067,1.),.UNSPECIFIED.);
#205=B_SPLINE_CURVE_WITH_KNOTS('',3,(#47921,#47922,#47923,#47924,#47925,
#47926,#47927,#47928,#47929,#47930,#47931,#47932,#47933,#47934,#47935,#47936,
#47937,#47938,#47939,#47940,#47941,#47942,#47943,#47944,#47945,#47946,#47947,
#47948,#47949,#47950,#47951,#47952,#47953,#47954,#47955,#47956,#47957,#47958,
#47959,#47960,#47961,#47962,#47963,#47964,#47965,#47966,#47967,#47968,#47969,
#47970,#47971,#47972,#47973,#47974,#47975,#47976,#47977,#47978,#47979,#47980,
#47981,#47982,#47983,#47984,#47985,#47986,#47987,#47988,#47989,#47990,#47991,
#47992,#47993,#47994,#47995,#47996,#47997,#47998,#47999,#48000,#48001,#48002,
#48003,#48004,#48005,#48006,#48007,#48008,#48009,#48010,#48011,#48012,#48013,
#48014,#48015,#48016,#48017,#48018,#48019,#48020),.UNSPECIFIED.,.F.,.F.,
(4,3,3,3,3,3,3,3,3,3,3,3,3,3,3,3,3,3,3,3,3,3,3,3,3,3,3,3,3,3,3,3,3,4),(0.,
0.00328733869888417,0.0753749786215322,0.124999999999997,0.164356278458853,
0.187499999999995,0.218749999999994,0.234374999999994,0.242187499999994,
0.246093749999994,0.24961089402613,0.249999999999994,0.315510705211053,
0.331931331987761,0.396997846930877,0.460736474732702,0.499909864635484,
0.499999999999991,0.563260702089509,0.624999999999989,0.667901539577085,
0.687499999999989,0.718749999999988,0.734374999999988,0.742187499999988,
0.746093749999988,0.749555837689128,0.749999999999988,0.820384404417581,
0.835461566544658,0.907599319949528,0.981379542643532,0.996551188491584,
1.),.UNSPECIFIED.);
#206=B_SPLINE_CURVE_WITH_KNOTS('',3,(#48059,#48060,#48061,#48062,#48063,
#48064,#48065,#48066,#48067,#48068,#48069,#48070,#48071,#48072,#48073,#48074,
#48075,#48076,#48077,#48078,#48079,#48080,#48081,#48082,#48083,#48084,#48085,
#48086,#48087,#48088,#48089),.UNSPECIFIED.,.F.,.F.,(4,3,3,3,3,3,3,3,3,3,
4),(0.,0.124999999999988,0.187499999999983,0.21874999999998,0.234374999999979,
0.24218749999998,0.24999999999998,0.374999999999982,0.499999999999985,0.749999999999992,
1.),.UNSPECIFIED.);
#207=B_SPLINE_CURVE_WITH_KNOTS('',3,(#48090,#48091,#48092,#48093,#48094,
#48095),.UNSPECIFIED.,.F.,.F.,(4,1,1,4),(0.,0.3333333333333,0.6666666666667,
0.999998511429527),.UNSPECIFIED.);
#208=B_SPLINE_CURVE_WITH_KNOTS('',3,(#48096,#48097,#48098,#48099,#48100,
#48101,#48102,#48103,#48104,#48105,#48106,#48107,#48108,#48109,#48110,#48111,
#48112,#48113,#48114,#48115,#48116,#48117,#48118,#48119,#48120,#48121,#48122,
#48123,#48124,#48125,#48126,#48127,#48128,#48129,#48130,#48131,#48132,#48133,
#48134,#48135,#48136,#48137,#48138,#48139,#48140,#48141,#48142,#48143,#48144,
#48145,#48146,#48147,#48148,#48149,#48150,#48151,#48152,#48153,#48154,#48155,
#48156),.UNSPECIFIED.,.F.,.F.,(4,3,3,3,3,3,3,3,3,3,3,3,3,3,3,3,3,3,3,3,
4),(1.42553447152832E-10,0.0839810989411267,0.196377742902089,0.24999999999996,
0.279015455686927,0.37499999999994,0.437499999999929,0.468749999999923,
0.468865232487923,0.484374999999921,0.492187499999922,0.498689296997412,
0.499999999999923,0.579361224328497,0.654563668474195,0.68797699979001,
0.749999999999961,0.818702539099431,0.877832781625891,0.941885020163088,
0.999999999925446),.UNSPECIFIED.);
#209=B_SPLINE_CURVE_WITH_KNOTS('',3,(#48199,#48200,#48201,#48202,#48203,
#48204,#48205,#48206,#48207,#48208,#48209,#48210,#48211,#48212,#48213,#48214,
#48215,#48216,#48217,#48218,#48219,#48220,#48221,#48222,#48223,#48224,#48225,
#48226,#48227,#48228,#48229,#48230,#48231,#48232,#48233,#48234,#48235,#48236,
#48237,#48238,#48239,#48240,#48241,#48242,#48243,#48244,#48245,#48246,#48247,
#48248,#48249,#48250,#48251,#48252,#48253,#48254,#48255,#48256,#48257,#48258,
#48259,#48260,#48261,#48262,#48263,#48264,#48265,#48266,#48267,#48268,#48269,
#48270,#48271,#48272,#48273,#48274,#48275,#48276,#48277,#48278,#48279,#48280,
#48281,#48282,#48283,#48284,#48285,#48286,#48287,#48288,#48289),
 .UNSPECIFIED.,.F.,.F.,(4,3,3,3,3,3,3,3,3,3,3,3,3,3,3,3,3,3,3,3,3,3,3,3,
3,3,3,3,3,3,4),(1.9887196109883E-7,0.0470903055258525,0.0950885788175302,
0.109526530949826,0.125000000000002,0.176685448395246,0.187500000000003,
0.195574875832608,0.203125000000002,0.218750000000002,0.250000000000001,
0.270621369536984,0.334103679086635,0.398264763362707,0.43041445463061,
0.437499999999997,0.468749999999996,0.484374999999996,0.492187499999997,
0.498034134221128,0.499999999999997,0.559924709834862,0.600124997687488,
0.658475316866043,0.715889402365164,0.764251055692731,0.821850435693596,
0.87861656776704,0.918179747173176,0.97096325070799,1.),.UNSPECIFIED.);
#210=B_SPLINE_CURVE_WITH_KNOTS('',3,(#48330,#48331,#48332,#48333,#48334,
#48335,#48336,#48337,#48338,#48339,#48340,#48341,#48342,#48343,#48344,#48345,
#48346,#48347,#48348,#48349,#48350,#48351,#48352,#48353,#48354,#48355,#48356,
#48357,#48358,#48359,#48360,#48361,#48362,#48363,#48364,#48365,#48366,#48367,
#48368,#48369,#48370,#48371,#48372,#48373,#48374,#48375,#48376,#48377,#48378,
#48379,#48380,#48381,#48382,#48383,#48384,#48385,#48386,#48387),
 .UNSPECIFIED.,.F.,.F.,(4,3,3,3,3,3,3,3,3,3,3,3,3,3,3,3,3,3,3,4),(0.,0.0625,
0.123439667231836,0.183439614487077,0.242384759211611,0.25,0.308039807183335,
0.365336058327834,0.422295847686103,0.479062355395686,0.535777748341937,
0.592769485850589,0.64998171356429,0.707851314182894,0.75,0.808900888439781,
0.869149194465956,0.930289889916406,0.992896943668474,1.),.UNSPECIFIED.);
#211=B_SPLINE_CURVE_WITH_KNOTS('',3,(#48389,#48390,#48391,#48392,#48393,
#48394,#48395,#48396,#48397,#48398,#48399,#48400,#48401,#48402,#48403,#48404,
#48405,#48406,#48407,#48408,#48409,#48410,#48411,#48412,#48413),
 .UNSPECIFIED.,.F.,.F.,(4,3,3,3,3,3,3,3,4),(2.75410129806085E-6,0.104998984641379,
0.285738798613509,0.468553914078819,0.5,0.679723771264366,0.694842839233207,
0.871856624429499,0.999999999992336),.UNSPECIFIED.);
#212=B_SPLINE_CURVE_WITH_KNOTS('',3,(#48415,#48416,#48417,#48418,#48419,
#48420,#48421,#48422,#48423,#48424,#48425,#48426,#48427),.UNSPECIFIED.,
 .F.,.F.,(4,3,3,3,4),(0.,0.218750000000002,0.250000000000002,0.500000000000001,
1.),.UNSPECIFIED.);
#213=B_SPLINE_CURVE_WITH_KNOTS('',3,(#48428,#48429,#48430,#48431,#48432,
#48433,#48434,#48435,#48436,#48437,#48438,#48439,#48440,#48441,#48442,#48443,
#48444,#48445,#48446,#48447,#48448,#48449,#48450,#48451,#48452,#48453,#48454,
#48455,#48456,#48457,#48458,#48459,#48460,#48461,#48462,#48463,#48464,#48465,
#48466,#48467,#48468,#48469,#48470,#48471,#48472,#48473,#48474,#48475,#48476,
#48477,#48478,#48479,#48480,#48481,#48482,#48483,#48484,#48485),
 .UNSPECIFIED.,.F.,.F.,(4,3,3,3,3,3,3,3,3,3,3,3,3,3,3,3,3,3,3,4),(0.,0.0665772925752716,
0.0719281228356136,0.141169980961546,0.214018425126579,0.249999999999986,
0.264563302840939,0.341169571707878,0.374999999999978,0.437499999999976,
0.468749999999975,0.484374999999976,0.486525989533565,0.496474805711493,
0.499999999999976,0.607879987507896,0.687145580677176,0.799955784674695,
0.890947396547385,1.),.UNSPECIFIED.);
#214=B_SPLINE_CURVE_WITH_KNOTS('',3,(#48527,#48528,#48529,#48530,#48531,
#48532,#48533,#48534,#48535,#48536,#48537,#48538,#48539,#48540,#48541,#48542,
#48543,#48544,#48545,#48546,#48547,#48548,#48549,#48550,#48551,#48552,#48553,
#48554,#48555,#48556,#48557,#48558,#48559,#48560,#48561,#48562,#48563,#48564,
#48565,#48566,#48567,#48568,#48569,#48570,#48571,#48572,#48573,#48574,#48575,
#48576,#48577,#48578,#48579,#48580,#48581,#48582,#48583,#48584,#48585,#48586,
#48587,#48588,#48589,#48590,#48591,#48592,#48593,#48594,#48595,#48596,#48597,
#48598,#48599,#48600,#48601,#48602,#48603,#48604,#48605,#48606,#48607,#48608,
#48609,#48610,#48611,#48612,#48613,#48614),.UNSPECIFIED.,.F.,.F.,(4,3,3,
3,3,3,3,3,3,3,3,3,3,3,3,3,3,3,3,3,3,3,3,3,3,3,3,3,3,4),(0.,0.0527820704689245,
0.081820550075384,0.138472337731971,0.195944438078264,0.23574955951297,
0.293011727177245,0.351192985818588,0.399875426522106,0.437499999999996,
0.468749999999997,0.484374999999997,0.492187499999997,0.496093749999997,
0.499508599033293,0.499999999999998,0.56586096599558,0.629575206715251,
0.693959306753081,0.725751294986733,0.781250000000004,0.790730946680812,
0.796875000000004,0.812500000000004,0.86904415250083,0.875000000000003,
0.884835923229597,0.938701686179648,0.993362246004367,0.999999777714025),
 .UNSPECIFIED.);
#215=B_SPLINE_CURVE_WITH_KNOTS('',3,(#48617,#48618,#48619,#48620,#48621,
#48622,#48623,#48624,#48625,#48626,#48627,#48628,#48629,#48630,#48631,#48632,
#48633,#48634,#48635,#48636,#48637,#48638,#48639,#48640,#48641,#48642,#48643,
#48644,#48645,#48646,#48647,#48648,#48649,#48650,#48651,#48652,#48653,#48654,
#48655,#48656,#48657,#48658,#48659,#48660,#48661,#48662,#48663,#48664,#48665,
#48666,#48667,#48668,#48669,#48670,#48671,#48672,#48673,#48674),
 .UNSPECIFIED.,.F.,.F.,(4,3,3,3,3,3,3,3,3,3,3,3,3,3,3,3,3,3,3,4),(1.82694913577423E-11,
0.0585628393002113,0.117996178041119,0.168707834458927,0.22854128310571,
0.249999999999999,0.312499999999999,0.374999999999999,0.421054295308903,
0.467108590617808,0.499999999999999,0.56353289982233,0.626399530677736,
0.688223249658798,0.749999999999999,0.771768873464095,0.832605909367747,
0.892881470692987,0.952307026214462,0.999999961863703),.UNSPECIFIED.);
#216=B_SPLINE_CURVE_WITH_KNOTS('',3,(#48725,#48726,#48727,#48728,#48729,
#48730,#48731,#48732,#48733,#48734,#48735,#48736,#48737,#48738,#48739,#48740,
#48741,#48742,#48743,#48744,#48745,#48746,#48747,#48748,#48749,#48750,#48751,
#48752,#48753,#48754,#48755,#48756,#48757,#48758,#48759,#48760,#48761,#48762,
#48763,#48764,#48765,#48766,#48767,#48768,#48769,#48770,#48771,#48772,#48773,
#48774,#48775,#48776,#48777,#48778,#48779,#48780,#48781,#48782,#48783,#48784,
#48785,#48786,#48787,#48788,#48789,#48790,#48791,#48792,#48793,#48794,#48795,
#48796,#48797,#48798,#48799,#48800,#48801,#48802,#48803,#48804,#48805,#48806,
#48807,#48808,#48809,#48810,#48811,#48812,#48813,#48814,#48815,#48816,#48817,
#48818,#48819,#48820,#48821,#48822,#48823,#48824,#48825,#48826,#48827,#48828,
#48829,#48830,#48831,#48832,#48833,#48834,#48835,#48836,#48837,#48838,#48839,
#48840,#48841,#48842,#48843,#48844,#48845,#48846,#48847,#48848,#48849,#48850,
#48851,#48852,#48853,#48854,#48855,#48856,#48857,#48858,#48859,#48860,#48861,
#48862,#48863,#48864,#48865,#48866,#48867,#48868,#48869,#48870,#48871,#48872,
#48873,#48874,#48875,#48876,#48877,#48878,#48879,#48880,#48881,#48882,#48883,
#48884,#48885,#48886,#48887,#48888,#48889,#48890,#48891,#48892,#48893,#48894,
#48895,#48896,#48897,#48898,#48899,#48900,#48901,#48902,#48903,#48904,#48905,
#48906,#48907,#48908,#48909,#48910,#48911,#48912,#48913,#48914,#48915,#48916,
#48917,#48918,#48919,#48920,#48921,#48922,#48923,#48924,#48925,#48926,#48927,
#48928,#48929,#48930,#48931,#48932,#48933,#48934,#48935,#48936,#48937,#48938,
#48939,#48940,#48941,#48942,#48943,#48944,#48945,#48946,#48947,#48948,#48949,
#48950,#48951,#48952,#48953,#48954,#48955,#48956,#48957,#48958,#48959,#48960,
#48961,#48962,#48963,#48964,#48965,#48966,#48967,#48968,#48969,#48970,#48971),
 .UNSPECIFIED.,.F.,.F.,(4,3,3,3,3,3,3,3,3,3,3,3,3,3,3,3,3,3,3,3,3,3,3,3,
3,3,3,3,3,3,3,3,3,3,3,3,3,3,3,3,3,3,3,3,3,3,3,3,3,3,3,3,3,3,3,3,3,3,3,3,
3,3,3,3,3,3,3,3,3,3,3,3,3,3,3,3,3,3,3,3,3,3,4),(9.75973301747209E-8,0.0159118695155719,
0.0312500000000116,0.0468750000000174,0.0546875000000203,0.0585937500000218,
0.0623038556224994,0.0625000000000233,0.064880126691803,0.0838067325806669,
0.102671826588194,0.109375000000042,0.117187500000045,0.121093750000046,
0.123046875000047,0.124023437500047,0.124511718750048,0.125000000000048,
0.130903386642066,0.145647760556128,0.16030635703608,0.171875000000055,
0.179687500000056,0.183593750000057,0.185546875000057,0.186523437500057,
0.187500000000057,0.198318862785137,0.209096158356209,0.213486683424382,
0.224229801399845,0.234902287104572,0.242187500000057,0.246093750000057,
0.248046875000057,0.249023437500057,0.249755859375057,0.250000000000057,
0.286148785115262,0.331156930318982,0.373125773103967,0.413994518747176,
0.43750000000003,0.442035565805872,0.468750000000026,0.484375000000024,
0.492187500000022,0.496093750000022,0.498046875000022,0.498793771580626,
0.499023437500022,0.499511718750022,0.500000000000021,0.52780801953624,
0.555633916578266,0.58020272164201,0.608271007010268,0.634689717609213,
0.640624999999996,0.645733764714709,0.648437499999995,0.665743528084154,
0.677861217283039,0.695360989880092,0.712946719081514,0.730621384502898,
0.734374999999979,0.742187499999977,0.746093749999977,0.748046874999976,
0.749023437499976,0.749511718749976,0.749999999999976,0.752465380543056,
0.797962909276469,0.804120644423907,0.850530768471112,0.858778904853475,
0.906286042923783,0.920200820756934,0.968991302096034,0.993035530701956,
1.),.UNSPECIFIED.);
#217=B_SPLINE_CURVE_WITH_KNOTS('',3,(#49054,#49055,#49056,#49057,#49058,
#49059,#49060,#49061,#49062,#49063,#49064,#49065,#49066,#49067,#49068,#49069,
#49070,#49071,#49072,#49073,#49074,#49075,#49076,#49077,#49078,#49079,#49080,
#49081,#49082,#49083,#49084,#49085,#49086,#49087,#49088,#49089,#49090,#49091,
#49092,#49093,#49094,#49095,#49096,#49097,#49098,#49099,#49100,#49101,#49102,
#49103,#49104,#49105,#49106,#49107,#49108,#49109,#49110,#49111,#49112,#49113,
#49114,#49115,#49116,#49117,#49118,#49119,#49120,#49121,#49122,#49123,#49124,
#49125,#49126,#49127,#49128,#49129,#49130,#49131,#49132,#49133,#49134,#49135,
#49136,#49137,#49138,#49139,#49140,#49141,#49142,#49143,#49144,#49145,#49146,
#49147,#49148,#49149,#49150,#49151,#49152,#49153,#49154,#49155,#49156,#49157,
#49158,#49159,#49160,#49161,#49162,#49163,#49164,#49165,#49166,#49167,#49168,
#49169,#49170,#49171,#49172,#49173,#49174,#49175,#49176,#49177,#49178,#49179,
#49180,#49181,#49182,#49183,#49184,#49185,#49186,#49187,#49188,#49189,#49190,
#49191,#49192,#49193,#49194,#49195,#49196,#49197,#49198,#49199,#49200,#49201,
#49202,#49203,#49204,#49205,#49206,#49207,#49208,#49209,#49210),
 .UNSPECIFIED.,.F.,.F.,(4,3,3,3,3,3,3,3,3,3,3,3,3,3,3,3,3,3,3,3,3,3,3,3,
3,3,3,3,3,3,3,3,3,3,3,3,3,3,3,3,3,3,3,3,3,3,3,3,3,3,3,3,4),(1.72726539092123E-7,
0.043457309737723,0.0863338395015235,0.0932167347872756,0.124999999999967,
0.165840006934032,0.177273215764065,0.18749999999995,0.218749999999942,
0.234374999999937,0.242187499999935,0.246093749999934,0.249511718749934,
0.249999999999933,0.260113268690261,0.284904696510657,0.309601788337845,
0.31249999999994,0.336932312064704,0.343749999999943,0.359374999999945,
0.359741477424532,0.367187499999946,0.371093749999946,0.373046874999946,
0.374023437499947,0.374999999999947,0.427161972770903,0.437499999999952,
0.446539278308906,0.468749999999955,0.484374999999956,0.492187499999957,
0.499058228052342,0.499999999999957,0.52937268418032,0.595489014678813,
0.601624978398085,0.624999999999968,0.666787080930481,0.687499999999974,
0.718749999999976,0.726755041126725,0.734374999999978,0.746093749999979,
0.749999999999979,0.777565452150545,0.821930738816808,0.864144411456503,
0.906141574463173,0.949726410631746,0.995918599599637,0.999999956001335),
 .UNSPECIFIED.);
#218=B_SPLINE_CURVE_WITH_KNOTS('',3,(#49251,#49252,#49253,#49254,#49255,
#49256,#49257,#49258,#49259,#49260,#49261,#49262,#49263,#49264,#49265,#49266,
#49267,#49268,#49269,#49270,#49271,#49272,#49273,#49274,#49275,#49276,#49277,
#49278,#49279,#49280,#49281),.UNSPECIFIED.,.F.,.F.,(4,3,3,3,3,3,3,3,3,3,
4),(0.,0.125,0.1875,0.218750000000001,0.234375000000001,0.242187500000001,
0.250000000000001,0.375000000000001,0.500000000000001,0.75,1.),
 .UNSPECIFIED.);
#219=B_SPLINE_CURVE_WITH_KNOTS('',3,(#49283,#49284,#49285,#49286,#49287,
#49288,#49289,#49290,#49291,#49292,#49293,#49294,#49295,#49296,#49297,#49298,
#49299,#49300,#49301,#49302,#49303,#49304,#49305,#49306,#49307),
 .UNSPECIFIED.,.F.,.F.,(4,3,3,3,3,3,3,3,4),(0.,0.177032879059826,0.297841464654054,
0.477609256376899,0.5,0.682857180362573,0.863757928480276,0.887961286767199,
0.999997248082941),.UNSPECIFIED.);
#220=B_SPLINE_CURVE_WITH_KNOTS('',3,(#49310,#49311,#49312,#49313,#49314,
#49315,#49316,#49317,#49318,#49319,#49320,#49321,#49322,#49323,#49324,#49325,
#49326,#49327,#49328,#49329,#49330,#49331,#49332,#49333,#49334,#49335,#49336,
#49337,#49338,#49339,#49340,#49341,#49342,#49343,#49344,#49345,#49346,#49347,
#49348,#49349,#49350,#49351,#49352,#49353,#49354,#49355,#49356,#49357,#49358,
#49359,#49360,#49361,#49362,#49363,#49364,#49365,#49366,#49367,#49368,#49369,
#49370),.UNSPECIFIED.,.F.,.F.,(4,3,3,3,3,3,3,3,3,3,3,3,3,3,3,3,3,3,3,3,
4),(0.,0.106434110907981,0.221226834799591,0.249999999999998,0.31037540950159,
0.374999999999998,0.437499999999997,0.468749999999998,0.484374999999999,
0.494167919221464,0.5,0.510705335967005,0.592733299703605,0.670419047251969,
0.732755379993678,0.75,0.823662512114083,0.893640330195904,0.925951097491995,
0.992933814532853,0.99999999981018),.UNSPECIFIED.);
#221=B_SPLINE_CURVE_WITH_KNOTS('',3,(#49415,#49416,#49417,#49418,#49419,
#49420,#49421,#49422,#49423,#49424,#49425,#49426,#49427,#49428,#49429,#49430,
#49431,#49432,#49433,#49434,#49435,#49436,#49437,#49438,#49439,#49440,#49441,
#49442,#49443,#49444,#49445,#49446,#49447,#49448,#49449,#49450,#49451,#49452,
#49453,#49454,#49455,#49456,#49457,#49458,#49459,#49460,#49461,#49462,#49463,
#49464,#49465,#49466,#49467,#49468,#49469,#49470,#49471,#49472,#49473,#49474,
#49475,#49476,#49477,#49478,#49479,#49480,#49481,#49482,#49483,#49484),
 .UNSPECIFIED.,.F.,.F.,(4,3,3,3,3,3,3,3,3,3,3,3,3,3,3,3,3,3,3,3,3,3,3,4),
(1.12531523137531E-11,0.0435574969286064,0.0764692287957928,0.120152779061659,
0.125,0.178557276903457,0.223905113123066,0.25,0.318766865591617,0.371575001885328,
0.375,0.469117767069314,0.5,0.519436421805622,0.625,0.667313247416635,0.741709817797934,
0.75,0.808035688025396,0.814957802298849,0.875,0.919742785397221,0.96245146142866,
0.999999720290089),.UNSPECIFIED.);
#222=B_SPLINE_CURVE_WITH_KNOTS('',3,(#49485,#49486,#49487,#49488,#49489,
#49490,#49491,#49492,#49493,#49494,#49495,#49496,#49497,#49498,#49499,#49500,
#49501,#49502,#49503,#49504,#49505,#49506,#49507,#49508,#49509,#49510,#49511,
#49512,#49513,#49514,#49515,#49516,#49517,#49518,#49519,#49520,#49521,#49522,
#49523,#49524,#49525,#49526,#49527,#49528,#49529,#49530,#49531,#49532,#49533,
#49534,#49535,#49536,#49537,#49538,#49539,#49540,#49541,#49542,#49543,#49544,
#49545,#49546,#49547,#49548,#49549,#49550,#49551,#49552,#49553,#49554),
 .UNSPECIFIED.,.F.,.F.,(4,3,3,3,3,3,3,3,3,3,3,3,3,3,3,3,3,3,3,3,3,3,3,4),
(0.,0.0642447266186201,0.129222196775793,0.139648686470079,0.203363383249967,
0.250000000000004,0.300656411054288,0.369078205527147,0.437500000000007,
0.468750000000006,0.469711834217933,0.484375000000006,0.495155243842182,
0.500000000000006,0.563334858178523,0.625631040088055,0.644014782496406,
0.704247086115865,0.750000000000003,0.807879611466452,0.868482449145389,
0.928163587732209,0.96196228291215,0.999999992441464),.UNSPECIFIED.);
#223=B_SPLINE_CURVE_WITH_KNOTS('',3,(#49590,#49591,#49592,#49593,#49594,
#49595,#49596,#49597,#49598,#49599,#49600,#49601,#49602,#49603,#49604,#49605,
#49606,#49607,#49608,#49609,#49610,#49611,#49612,#49613,#49614,#49615,#49616,
#49617,#49618,#49619,#49620,#49621,#49622,#49623,#49624,#49625,#49626,#49627,
#49628,#49629,#49630,#49631,#49632,#49633,#49634,#49635,#49636,#49637,#49638,
#49639,#49640,#49641,#49642,#49643,#49644,#49645,#49646,#49647),
 .UNSPECIFIED.,.F.,.F.,(4,3,3,3,3,3,3,3,3,3,3,3,3,3,3,3,3,3,3,4),(1.7829606324839E-11,
0.0708213913417186,0.13721260991132,0.198853000409921,0.25,0.306729430221608,
0.362647740453726,0.418203642728849,0.473372817506931,0.5,0.500000496896627,
0.555649586140288,0.611781191912524,0.668290257959578,0.725514453399843,
0.75,0.8125,0.877125626676368,0.947977205464318,1.),.UNSPECIFIED.);
#224=B_SPLINE_CURVE_WITH_KNOTS('',3,(#49684,#49685,#49686,#49687,#49688,
#49689,#49690,#49691,#49692,#49693,#49694,#49695,#49696,#49697,#49698,#49699,
#49700,#49701,#49702,#49703,#49704,#49705,#49706,#49707,#49708,#49709,#49710,
#49711,#49712,#49713,#49714,#49715,#49716,#49717,#49718,#49719,#49720,#49721,
#49722,#49723,#49724,#49725,#49726,#49727,#49728,#49729,#49730,#49731,#49732,
#49733,#49734,#49735,#49736,#49737,#49738,#49739,#49740,#49741,#49742,#49743,
#49744,#49745,#49746,#49747,#49748,#49749,#49750,#49751,#49752,#49753,#49754,
#49755,#49756,#49757,#49758,#49759,#49760,#49761,#49762,#49763,#49764,#49765),
 .UNSPECIFIED.,.F.,.F.,(4,3,3,3,3,3,3,3,3,3,3,3,3,3,3,3,3,3,3,3,3,3,3,3,
3,3,3,4),(0.,0.0665074781408924,0.124999999999997,0.128587305872536,0.187499999999996,
0.218749999999995,0.234374999999995,0.242187499999995,0.246093749999995,
0.249999999999995,0.31357815937848,0.385910368691815,0.457052959592689,
0.499999999999993,0.500014077280664,0.570198395648231,0.624999999999993,
0.686457107520193,0.687499999999992,0.718749999999992,0.734374999999992,
0.742187499999992,0.746093749999992,0.749999999999992,0.813997647135706,
0.871428993161989,0.938277857776933,1.),.UNSPECIFIED.);
#225=B_SPLINE_CURVE_WITH_KNOTS('',3,(#49810,#49811,#49812,#49813,#49814,
#49815,#49816,#49817,#49818,#49819,#49820,#49821,#49822,#49823,#49824,#49825,
#49826,#49827,#49828,#49829,#49830,#49831,#49832,#49833,#49834),
 .UNSPECIFIED.,.F.,.F.,(4,3,3,3,3,3,3,3,4),(1.36947301852406E-7,0.18198259021518,
0.249918134546699,0.432569342894789,0.5,0.68030149702564,0.803687769765186,
0.980976573749724,0.999933076643282),.UNSPECIFIED.);
#226=B_SPLINE_CURVE_WITH_KNOTS('',3,(#49836,#49837,#49838,#49839,#49840,
#49841,#49842,#49843),.UNSPECIFIED.,.F.,.F.,(4,2,2,4),(-0.00420679853302169,
0.,0.0656255554488885,0.124431075933089),.UNSPECIFIED.);
#227=B_SPLINE_CURVE_WITH_KNOTS('',3,(#49844,#49845,#49846,#49847,#49848,
#49849,#49850,#49851,#49852,#49853,#49854,#49855,#49856,#49857,#49858,#49859,
#49860,#49861,#49862,#49863,#49864,#49865,#49866,#49867,#49868,#49869,#49870,
#49871,#49872,#49873,#49874,#49875,#49876,#49877,#49878,#49879,#49880,#49881,
#49882,#49883,#49884,#49885,#49886,#49887,#49888,#49889,#49890,#49891,#49892,
#49893,#49894,#49895,#49896,#49897,#49898,#49899,#49900,#49901),
 .UNSPECIFIED.,.F.,.F.,(4,3,3,3,3,3,3,3,3,3,3,3,3,3,3,3,3,3,3,4),(4.63074357751375E-6,
0.0537910573104376,0.124260671753383,0.198033873731291,0.202362264714046,
0.250000000000014,0.329872316171993,0.391843303964045,0.437500000000024,
0.468750000000025,0.484375000000024,0.492187500000023,0.498247326271446,
0.500000000000022,0.586936000013064,0.685649851920606,0.757785027674918,
0.860226013175883,0.934923100363294,0.999973164507014),.UNSPECIFIED.);
#228=B_SPLINE_CURVE_WITH_KNOTS('',3,(#49947,#49948,#49949,#49950,#49951,
#49952,#49953,#49954,#49955,#49956,#49957,#49958,#49959,#49960,#49961,#49962,
#49963,#49964,#49965,#49966,#49967,#49968,#49969,#49970,#49971,#49972,#49973,
#49974,#49975,#49976,#49977,#49978,#49979,#49980,#49981,#49982,#49983,#49984,
#49985,#49986,#49987,#49988,#49989,#49990,#49991,#49992,#49993,#49994,#49995,
#49996,#49997,#49998,#49999,#50000,#50001,#50002,#50003,#50004,#50005,#50006,
#50007,#50008,#50009,#50010,#50011,#50012,#50013,#50014,#50015,#50016,#50017,
#50018,#50019),.UNSPECIFIED.,.F.,.F.,(4,3,3,3,3,3,3,3,3,3,3,3,3,3,3,3,3,
3,3,3,3,3,3,3,4),(1.4541246487959E-9,0.0431191253455669,0.0863267720301174,
0.129382358811508,0.1428571428571,0.153643952151576,0.204633581280749,0.255730997948089,
0.2857142857143,0.306393509456684,0.370923699443645,0.4285714285714,0.459412017999017,
0.526893092613459,0.5714285714286,0.612488429046519,0.677675308052048,0.7142857142857,
0.765391329809934,0.81987081595669,0.8571428571429,0.900979334814105,0.918139369307915,
0.961788840323352,0.999999180955248),.UNSPECIFIED.);
#229=B_SPLINE_CURVE_WITH_KNOTS('',3,(#50022,#50023,#50024,#50025,#50026,
#50027,#50028,#50029,#50030,#50031,#50032,#50033,#50034,#50035,#50036,#50037,
#50038,#50039,#50040,#50041,#50042,#50043,#50044,#50045,#50046,#50047,#50048,
#50049,#50050,#50051,#50052,#50053,#50054,#50055,#50056,#50057,#50058,#50059,
#50060,#50061,#50062,#50063,#50064,#50065,#50066,#50067,#50068,#50069,#50070,
#50071,#50072,#50073,#50074,#50075,#50076,#50077,#50078,#50079,#50080,#50081,
#50082,#50083,#50084,#50085,#50086,#50087,#50088,#50089,#50090,#50091,#50092,
#50093,#50094),.UNSPECIFIED.,.F.,.F.,(4,3,3,3,3,3,3,3,3,3,3,3,3,3,3,3,3,
3,3,3,3,3,3,3,4),(0.,0.0558892577558595,0.112669247365332,0.156953409719216,
0.215052214438557,0.25000000000001,0.309316250903252,0.324310832292704,
0.385391022432193,0.437500000000018,0.468750000000019,0.48437500000002,
0.49218750000002,0.4989493455236,0.500000000000019,0.504583562497372,0.573408597222544,
0.641343712531288,0.680145778473015,0.75000000000001,0.815926534003008,
0.847891270040952,0.91466903667937,0.980716328284555,1.),.UNSPECIFIED.);
#230=B_SPLINE_CURVE_WITH_KNOTS('',3,(#50193,#50194,#50195,#50196,#50197,
#50198,#50199,#50200,#50201,#50202,#50203,#50204,#50205,#50206,#50207,#50208,
#50209,#50210,#50211,#50212,#50213,#50214,#50215,#50216,#50217,#50218,#50219,
#50220,#50221,#50222,#50223,#50224,#50225,#50226,#50227,#50228,#50229,#50230,
#50231,#50232,#50233,#50234,#50235,#50236,#50237,#50238,#50239,#50240,#50241,
#50242,#50243,#50244,#50245,#50246,#50247,#50248,#50249,#50250,#50251,#50252,
#50253,#50254,#50255,#50256,#50257,#50258,#50259,#50260,#50261,#50262,#50263,
#50264,#50265,#50266,#50267,#50268,#50269,#50270,#50271,#50272,#50273,#50274,
#50275,#50276,#50277,#50278,#50279,#50280,#50281,#50282,#50283,#50284,#50285,
#50286,#50287,#50288,#50289,#50290,#50291,#50292,#50293,#50294,#50295,#50296,
#50297,#50298,#50299,#50300,#50301,#50302,#50303,#50304,#50305,#50306,#50307,
#50308,#50309,#50310,#50311,#50312,#50313,#50314,#50315,#50316,#50317,#50318,
#50319,#50320,#50321,#50322,#50323,#50324,#50325,#50326,#50327,#50328,#50329,
#50330,#50331,#50332,#50333,#50334,#50335,#50336,#50337,#50338,#50339,#50340,
#50341,#50342,#50343,#50344,#50345,#50346,#50347,#50348,#50349,#50350,#50351,
#50352,#50353,#50354,#50355,#50356,#50357,#50358),.UNSPECIFIED.,.F.,.F.,
(4,3,3,3,3,3,3,3,3,3,3,3,3,3,3,3,3,3,3,3,3,3,3,3,3,3,3,3,3,3,3,3,3,3,3,
3,3,3,3,3,3,3,3,3,3,3,3,3,3,3,3,3,3,3,3,4),(8.91796462514105E-8,0.0341889233486022,
0.0625000000000075,0.0800235801072087,0.0937500000000111,0.109375000000013,
0.117187500000014,0.121093750000014,0.123046875000014,0.125000000000014,
0.156896093632204,0.187500000000017,0.218750000000019,0.234375000000019,
0.237544069789223,0.242187500000019,0.24609375000002,0.248046875000019,
0.250000000000019,0.290852976477788,0.312500000000018,0.328940100187335,
0.343750000000017,0.359375000000017,0.367187500000017,0.371093750000017,
0.373046875000017,0.375000000000017,0.425222667670205,0.437500000000015,
0.468750000000014,0.484375000000014,0.492187500000013,0.496093750000013,
0.500000000000013,0.520152742598536,0.572584836177622,0.616900729170795,
0.62500000000001,0.65134213620691,0.678251303075323,0.687500000000008,0.709160585412811,
0.750000000000007,0.781250000000006,0.789062500000006,0.796875000000006,
0.799072644259708,0.812500000000005,0.858399969519928,0.875000000000003,
0.885492836009458,0.932681943708858,0.98079009164065,0.98573093829117,1.),
 .UNSPECIFIED.);
#231=B_SPLINE_CURVE_WITH_KNOTS('',3,(#50361,#50362,#50363,#50364,#50365,
#50366,#50367,#50368,#50369,#50370,#50371,#50372,#50373,#50374,#50375,#50376,
#50377,#50378,#50379,#50380,#50381,#50382,#50383,#50384,#50385,#50386,#50387,
#50388,#50389,#50390,#50391,#50392,#50393,#50394,#50395,#50396,#50397,#50398,
#50399,#50400,#50401,#50402,#50403,#50404,#50405,#50406,#50407,#50408,#50409,
#50410,#50411,#50412,#50413,#50414,#50415,#50416,#50417,#50418,#50419,#50420,
#50421,#50422,#50423,#50424,#50425,#50426,#50427,#50428,#50429,#50430,#50431,
#50432,#50433,#50434,#50435,#50436,#50437,#50438,#50439,#50440,#50441,#50442,
#50443,#50444,#50445,#50446,#50447,#50448,#50449,#50450,#50451,#50452,#50453,
#50454,#50455,#50456,#50457,#50458,#50459,#50460,#50461,#50462,#50463,#50464,
#50465,#50466,#50467,#50468,#50469,#50470,#50471,#50472,#50473,#50474,#50475,
#50476,#50477,#50478,#50479,#50480,#50481,#50482,#50483,#50484,#50485,#50486,
#50487,#50488,#50489,#50490,#50491,#50492,#50493,#50494,#50495,#50496,#50497,
#50498,#50499,#50500,#50501,#50502),.UNSPECIFIED.,.F.,.F.,(4,3,3,3,3,3,
3,3,3,3,3,3,3,3,3,3,3,3,3,3,3,3,3,3,3,3,3,3,3,3,3,3,3,3,3,3,3,3,3,3,3,3,
3,3,3,3,3,4),(2.34637988656816E-7,0.0315958274976916,0.0628964687251239,
0.0937122522318575,0.104172143984534,0.125,0.154837231987697,0.184674463975394,
0.213175784027995,0.218750000000001,0.234375000000001,0.242187500000001,
0.246093750000001,0.248046875000001,0.250000000000001,0.257790373752442,
0.295642404285767,0.33448340003201,0.354334938238437,0.392683239873593,
0.431398964572153,0.4704820316817,0.482378819405289,0.484374999999999,0.49658582239736,
0.499999999999999,0.540377618081788,0.580372330237114,0.609456768302146,
0.64916758132608,0.687499999999997,0.700832885131154,0.718749999999997,
0.734374999999997,0.742187499999997,0.746093749999997,0.748046874999997,
0.749999999999997,0.769091927835171,0.798967073430337,0.828842219025503,
0.858577125548687,0.874999999999998,0.896782376980454,0.927914312513236,
0.959582512827434,0.985641744950711,1.),.UNSPECIFIED.);
#232=B_SPLINE_CURVE_WITH_KNOTS('',3,(#50539,#50540,#50541,#50542,#50543,
#50544,#50545,#50546,#50547,#50548,#50549,#50550,#50551,#50552,#50553,#50554,
#50555,#50556,#50557,#50558,#50559,#50560,#50561,#50562,#50563,#50564,#50565,
#50566,#50567,#50568,#50569,#50570,#50571,#50572,#50573,#50574,#50575,#50576,
#50577,#50578,#50579,#50580,#50581,#50582,#50583,#50584,#50585,#50586,#50587,
#50588,#50589,#50590,#50591,#50592,#50593,#50594,#50595,#50596,#50597,#50598,
#50599),.UNSPECIFIED.,.F.,.F.,(4,3,3,3,3,3,3,3,3,3,3,3,3,3,3,3,3,3,3,3,
4),(3.81436954511069E-8,0.0594692266925058,0.119461338390937,0.180335235503925,
0.228233344473427,0.250000000000001,0.312500000000001,0.375000000000001,
0.420629555808829,0.466480510808558,0.500000000000001,0.532982686561363,
0.59558437717701,0.657507300746284,0.718468600168369,0.750000000000001,
0.809830738944292,0.831293936966436,0.890887168088582,0.94959438235366,
1.),.UNSPECIFIED.);
#233=B_SPLINE_CURVE_WITH_KNOTS('',3,(#50600,#50601,#50602,#50603,#50604,
#50605,#50606,#50607,#50608,#50609,#50610,#50611,#50612,#50613,#50614,#50615,
#50616,#50617,#50618,#50619,#50620,#50621,#50622,#50623,#50624,#50625,#50626,
#50627,#50628,#50629,#50630,#50631,#50632,#50633,#50634,#50635,#50636,#50637,
#50638,#50639,#50640,#50641,#50642,#50643,#50644,#50645,#50646,#50647,#50648,
#50649,#50650,#50651,#50652,#50653,#50654,#50655,#50656,#50657),
 .UNSPECIFIED.,.F.,.F.,(4,3,3,3,3,3,3,3,3,3,3,3,3,3,3,3,3,3,3,4),(0.,0.07023511355664,
0.136204759980801,0.197546204775853,0.25,0.308361863568339,0.365828750984795,
0.422887295093721,0.479509854680895,0.5,0.500088874817559,0.555696428953905,
0.611747912029764,0.668153881503749,0.725240099299435,0.75,0.8125,0.87677552836491,
0.947109081823081,1.),.UNSPECIFIED.);
#234=B_SPLINE_CURVE_WITH_KNOTS('',3,(#50703,#50704,#50705,#50706,#50707,
#50708,#50709,#50710,#50711,#50712,#50713,#50714,#50715,#50716,#50717,#50718,
#50719,#50720,#50721,#50722,#50723,#50724,#50725,#50726,#50727,#50728,#50729,
#50730,#50731,#50732,#50733,#50734,#50735,#50736,#50737,#50738,#50739,#50740,
#50741,#50742,#50743,#50744,#50745,#50746,#50747,#50748,#50749,#50750,#50751,
#50752,#50753,#50754,#50755,#50756,#50757,#50758,#50759,#50760),
 .UNSPECIFIED.,.F.,.F.,(4,3,3,3,3,3,3,3,3,3,3,3,3,3,3,3,3,3,3,4),(0.,0.0625,
0.123429255825999,0.183419343641415,0.242355359067083,0.25,0.308040972645323,
0.36533838298242,0.422299344729593,0.479067050605816,0.535783675525185,
0.592776687427881,0.649990213922836,0.707861096511507,0.75,0.808903293455612,
0.869154047623437,0.930297220487149,0.99290670407742,1.),.UNSPECIFIED.);
#235=B_SPLINE_CURVE_WITH_KNOTS('',3,(#50761,#50762,#50763,#50764,#50765,
#50766,#50767,#50768,#50769,#50770,#50771,#50772,#50773,#50774,#50775,#50776,
#50777,#50778,#50779,#50780,#50781,#50782,#50783,#50784,#50785,#50786,#50787,
#50788,#50789,#50790,#50791,#50792,#50793,#50794,#50795,#50796,#50797,#50798,
#50799,#50800,#50801,#50802,#50803,#50804,#50805,#50806,#50807,#50808,#50809,
#50810,#50811,#50812,#50813,#50814,#50815,#50816,#50817,#50818,#50819,#50820,
#50821,#50822,#50823,#50824,#50825,#50826,#50827,#50828,#50829,#50830,#50831,
#50832,#50833,#50834,#50835,#50836,#50837,#50838,#50839,#50840,#50841,#50842,
#50843,#50844,#50845,#50846,#50847,#50848,#50849,#50850,#50851,#50852,#50853,
#50854),.UNSPECIFIED.,.F.,.F.,(4,3,3,3,3,3,3,3,3,3,3,3,3,3,3,3,3,3,3,3,
3,3,3,3,3,3,3,3,3,3,3,4),(0.,0.00526477685132137,0.0911120621260249,0.124999999999999,
0.164492696482799,0.187499999999998,0.218749999999998,0.234374999999998,
0.242187499999998,0.246093749999998,0.248046874999998,0.249999999999997,
0.315561405830368,0.332546042754748,0.397233658308089,0.461991812577509,
0.499894561889816,0.499999999999991,0.564586350481157,0.624999999999988,
0.667250942464425,0.687499999999987,0.718749999999986,0.734374999999985,
0.742187499999985,0.746093749999985,0.748046874999985,0.749999999999985,
0.83529834404552,0.918975525864169,0.994552082753247,1.),.UNSPECIFIED.);
#236=B_SPLINE_CURVE_WITH_KNOTS('',3,(#50897,#50898,#50899,#50900,#50901,
#50902,#50903,#50904,#50905,#50906,#50907,#50908,#50909,#50910,#50911,#50912,
#50913,#50914,#50915,#50916,#50917,#50918,#50919,#50920,#50921,#50922,#50923,
#50924,#50925,#50926,#50927),.UNSPECIFIED.,.F.,.F.,(4,3,3,3,3,3,3,3,3,3,
4),(0.,0.124999999999993,0.18749999999999,0.218749999999989,0.234374999999987,
0.242187499999987,0.249999999999986,0.374999999999988,0.49999999999999,
0.749999999999995,1.),.UNSPECIFIED.);
#237=B_SPLINE_CURVE_WITH_KNOTS('',3,(#50928,#50929,#50930,#50931,#50932,
#50933,#50934,#50935,#50936,#50937,#50938,#50939,#50940,#50941,#50942,#50943,
#50944,#50945,#50946,#50947,#50948,#50949,#50950,#50951,#50952),
 .UNSPECIFIED.,.F.,.F.,(4,3,3,3,3,3,3,3,4),(0.,0.177256629021432,0.214956465801327,
0.395210606083471,0.5,0.682544097815536,0.772277414116928,0.954142569649918,
0.999999140627182),.UNSPECIFIED.);
#238=B_SPLINE_CURVE_WITH_KNOTS('',3,(#50953,#50954,#50955,#50956,#50957,
#50958,#50959,#50960,#50961,#50962,#50963,#50964,#50965,#50966,#50967,#50968,
#50969,#50970,#50971,#50972,#50973,#50974,#50975,#50976,#50977,#50978,#50979,
#50980,#50981,#50982,#50983,#50984,#50985,#50986,#50987,#50988,#50989,#50990,
#50991,#50992,#50993,#50994,#50995,#50996,#50997,#50998,#50999,#51000,#51001,
#51002,#51003,#51004,#51005,#51006,#51007,#51008,#51009,#51010,#51011,#51012,
#51013),.UNSPECIFIED.,.F.,.F.,(4,3,3,3,3,3,3,3,3,3,3,3,3,3,3,3,3,3,3,3,
4),(1.28199134739398E-10,0.070962309054426,0.173238035306535,0.248450970868743,
0.25,0.348335417086408,0.41932009272992,0.437499999999997,0.468749999999996,
0.484374999999996,0.492187499999996,0.497900248415515,0.499999999999997,
0.583530657236138,0.616659679343955,0.696381996825757,0.749999999999998,
0.804571254699382,0.878158467774757,0.951745680850132,0.999999999996763),
 .UNSPECIFIED.);
#239=B_SPLINE_CURVE_WITH_KNOTS('',3,(#51056,#51057,#51058,#51059,#51060,
#51061,#51062,#51063,#51064,#51065,#51066,#51067,#51068,#51069,#51070,#51071,
#51072,#51073,#51074,#51075,#51076,#51077,#51078,#51079,#51080,#51081,#51082,
#51083,#51084,#51085,#51086,#51087,#51088,#51089,#51090,#51091,#51092,#51093,
#51094,#51095,#51096,#51097,#51098,#51099,#51100,#51101,#51102,#51103,#51104,
#51105,#51106,#51107,#51108,#51109,#51110,#51111,#51112,#51113,#51114,#51115,
#51116,#51117,#51118,#51119,#51120,#51121,#51122,#51123,#51124,#51125,#51126,
#51127,#51128,#51129,#51130,#51131,#51132,#51133,#51134,#51135,#51136,#51137,
#51138,#51139,#51140,#51141,#51142,#51143,#51144,#51145,#51146),
 .UNSPECIFIED.,.F.,.F.,(4,3,3,3,3,3,3,3,3,3,3,3,3,3,3,3,3,3,3,3,3,3,3,3,
3,3,3,3,3,3,4),(1.98906495286848E-7,0.0470898563921683,0.0950876937980486,
0.109526430295898,0.125,0.176684971632146,0.1875,0.195574841813231,0.203125,
0.21875,0.25,0.270621653555496,0.334104133193722,0.398265383295987,0.430414688308331,
0.4375,0.46875,0.484375,0.4921875,0.498034123291998,0.500000000000001,0.559924704434065,
0.600124957473912,0.658475263308525,0.715889338441014,0.764250567660699,
0.8218499773925,0.878616139622934,0.918178964193708,0.970962436356723,1.),
 .UNSPECIFIED.);
#240=B_SPLINE_CURVE_WITH_KNOTS('',3,(#51197,#51198,#51199,#51200,#51201,
#51202,#51203,#51204,#51205,#51206,#51207,#51208,#51209,#51210,#51211,#51212,
#51213,#51214,#51215,#51216,#51217,#51218,#51219,#51220,#51221),
 .UNSPECIFIED.,.F.,.F.,(4,3,3,3,3,3,3,3,4),(8.00074943874998E-8,0.150887609476909,
0.211670949228306,0.3333333333333,0.508675768769221,0.623916433730383,0.6666666666667,
0.83333333333335,1.),.UNSPECIFIED.);
#241=B_SPLINE_CURVE_WITH_KNOTS('',3,(#51223,#51224,#51225,#51226,#51227,
#51228,#51229,#51230,#51231,#51232,#51233),.UNSPECIFIED.,.F.,.F.,(4,1,2,
2,2,4),(0.,0.124999999999996,0.218749999999993,0.249999999999992,0.499999999999995,
1.),.UNSPECIFIED.);
#242=B_SPLINE_CURVE_WITH_KNOTS('',3,(#51234,#51235,#51236,#51237,#51238,
#51239,#51240,#51241,#51242,#51243,#51244,#51245,#51246,#51247,#51248,#51249,
#51250,#51251,#51252,#51253,#51254,#51255,#51256,#51257,#51258,#51259,#51260,
#51261,#51262,#51263,#51264,#51265,#51266,#51267,#51268,#51269,#51270,#51271,
#51272,#51273,#51274,#51275,#51276,#51277,#51278,#51279,#51280,#51281,#51282,
#51283,#51284,#51285,#51286,#51287,#51288),.UNSPECIFIED.,.F.,.F.,(4,3,3,
3,3,3,3,3,3,3,3,3,3,3,3,3,3,3,4),(0.,0.0544322267884975,0.110762977555986,
0.168281172499134,0.227824949411008,0.250000000000006,0.315494399733559,
0.375000000000008,0.43750000000001,0.468750000000011,0.484375000000011,
0.494989881597992,0.500000000000011,0.59005681178326,0.685607308844679,
0.783754001548365,0.886959143600766,0.972258800028934,1.),.UNSPECIFIED.);
#243=B_SPLINE_CURVE_WITH_KNOTS('',3,(#51330,#51331,#51332,#51333,#51334,
#51335,#51336,#51337,#51338,#51339,#51340,#51341,#51342,#51343,#51344,#51345,
#51346,#51347,#51348,#51349,#51350,#51351,#51352,#51353,#51354,#51355,#51356,
#51357,#51358,#51359,#51360,#51361,#51362,#51363,#51364,#51365,#51366,#51367,
#51368,#51369,#51370,#51371,#51372,#51373,#51374,#51375,#51376,#51377,#51378,
#51379,#51380,#51381,#51382,#51383,#51384,#51385,#51386,#51387,#51388,#51389,
#51390,#51391,#51392,#51393,#51394,#51395,#51396,#51397,#51398,#51399,#51400,
#51401,#51402,#51403,#51404,#51405,#51406,#51407,#51408,#51409,#51410,#51411,
#51412,#51413,#51414,#51415,#51416,#51417),.UNSPECIFIED.,.F.,.F.,(4,3,3,
3,3,3,3,3,3,3,3,3,3,3,3,3,3,3,3,3,3,3,3,3,3,3,3,3,3,4),(0.,0.0527820095289333,
0.0818213288309768,0.138473111371745,0.195945206951966,0.235750026621739,
0.293012168939004,0.351193384242706,0.399875448565708,0.437500000000007,
0.468750000000007,0.484375000000007,0.492187500000006,0.496093750000006,
0.499508594967082,0.500000000000006,0.565860739773587,0.629574808670008,
0.693958741288855,0.725750998861238,0.781250000000002,0.790730932595577,
0.796875000000001,0.812500000000001,0.869044093253454,0.875000000000001,
0.884835905848476,0.938701632182115,0.99336215698859,0.999999777714142),
 .UNSPECIFIED.);
#244=B_SPLINE_CURVE_WITH_KNOTS('',3,(#51420,#51421,#51422,#51423,#51424,
#51425,#51426,#51427,#51428,#51429,#51430,#51431,#51432,#51433,#51434,#51435,
#51436,#51437,#51438,#51439,#51440,#51441,#51442,#51443,#51444,#51445,#51446,
#51447,#51448,#51449,#51450,#51451,#51452,#51453,#51454,#51455,#51456,#51457,
#51458,#51459,#51460,#51461,#51462,#51463,#51464,#51465,#51466,#51467,#51468,
#51469,#51470,#51471,#51472,#51473,#51474,#51475,#51476,#51477),
 .UNSPECIFIED.,.F.,.F.,(4,3,3,3,3,3,3,3,3,3,3,3,3,3,3,3,3,3,3,4),(8.78525880136469E-7,
0.0585642409233348,0.117997885332985,0.168707876010783,0.228541702004436,
0.25,0.3125,0.375,0.421054242624552,0.467108485249104,0.5,0.563532905950584,
0.626399542664273,0.688223267168837,0.75,0.771768826617254,0.83260586843843,
0.892881435436045,0.952306996196428,0.999999961863698),.UNSPECIFIED.);
#245=B_SPLINE_CURVE_WITH_KNOTS('',3,(#51528,#51529,#51530,#51531,#51532,
#51533,#51534,#51535,#51536,#51537,#51538,#51539,#51540,#51541,#51542,#51543,
#51544,#51545,#51546,#51547,#51548,#51549,#51550,#51551,#51552,#51553,#51554,
#51555,#51556,#51557,#51558,#51559,#51560,#51561,#51562,#51563,#51564,#51565,
#51566,#51567,#51568,#51569,#51570,#51571,#51572,#51573,#51574,#51575,#51576,
#51577,#51578,#51579,#51580,#51581,#51582,#51583,#51584,#51585,#51586,#51587,
#51588,#51589,#51590,#51591,#51592,#51593,#51594,#51595,#51596,#51597,#51598,
#51599,#51600,#51601,#51602,#51603,#51604,#51605,#51606,#51607,#51608,#51609,
#51610,#51611,#51612,#51613,#51614,#51615,#51616,#51617,#51618,#51619,#51620,
#51621,#51622,#51623,#51624,#51625,#51626,#51627,#51628,#51629,#51630,#51631,
#51632,#51633,#51634,#51635,#51636,#51637,#51638,#51639,#51640,#51641,#51642,
#51643,#51644,#51645,#51646,#51647,#51648,#51649,#51650,#51651,#51652,#51653,
#51654,#51655,#51656,#51657,#51658,#51659,#51660,#51661,#51662,#51663,#51664,
#51665,#51666,#51667,#51668,#51669,#51670,#51671,#51672,#51673,#51674,#51675,
#51676,#51677,#51678,#51679,#51680,#51681,#51682,#51683,#51684,#51685,#51686,
#51687,#51688,#51689,#51690,#51691,#51692,#51693,#51694,#51695,#51696,#51697,
#51698,#51699,#51700,#51701,#51702,#51703,#51704,#51705,#51706,#51707,#51708,
#51709,#51710,#51711,#51712,#51713,#51714,#51715,#51716,#51717,#51718,#51719,
#51720,#51721,#51722,#51723,#51724,#51725,#51726,#51727,#51728,#51729,#51730,
#51731,#51732,#51733,#51734,#51735,#51736,#51737,#51738,#51739,#51740,#51741,
#51742,#51743,#51744,#51745,#51746,#51747,#51748,#51749,#51750,#51751,#51752,
#51753,#51754,#51755,#51756,#51757,#51758,#51759,#51760,#51761,#51762,#51763,
#51764,#51765,#51766,#51767,#51768,#51769,#51770,#51771),.UNSPECIFIED.,
 .F.,.F.,(4,3,3,3,3,3,3,3,3,3,3,3,3,3,3,3,3,3,3,3,3,3,3,3,3,3,3,3,3,3,3,
3,3,3,3,3,3,3,3,3,3,3,3,3,3,3,3,3,3,3,3,3,3,3,3,3,3,3,3,3,3,3,3,3,3,3,3,
3,3,3,3,3,3,3,3,3,3,3,3,3,3,4),(9.75974323886041E-8,0.0159118694038098,
0.031250000000004,0.0468750000000061,0.0546875000000072,0.0585937500000077,
0.0623038553748027,0.0625000000000082,0.064880126712784,0.0838067330365208,
0.102671827483111,0.109375000000014,0.117187500000015,0.121093750000015,
0.123046875000016,0.124023437500016,0.124511718750016,0.125000000000016,
0.130903386566927,0.14564776013408,0.160306356267678,0.171875000000023,
0.179687500000024,0.183593750000025,0.185546875000025,0.186523437500025,
0.187500000000025,0.198318863007,0.209096158798105,0.213486682905972,0.224229801102837,
0.234902287027138,0.242187500000032,0.246093750000033,0.248046875000033,
0.249023437500033,0.249755859375033,0.250000000000033,0.28614878553653,
0.331156929523491,0.373125773860353,0.413936165812502,0.442035566291532,
0.468750000000073,0.484375000000075,0.492187500000077,0.496093750000077,
0.498046875000078,0.49879377159272,0.499023437500078,0.499511718750078,
0.500000000000078,0.527808016721212,0.555633910969737,0.580202724032766,
0.608271006625457,0.634689718024949,0.640625000000101,0.645733762002606,
0.648437500000103,0.665743521005006,0.677861205829731,0.695360971298973,
0.712946693311888,0.730621351505351,0.734375000000116,0.742187500000117,
0.746093750000118,0.748046875000119,0.749023437500118,0.749511718750118,
0.750000000000118,0.752465380464155,0.797962909864778,0.804120644560384,
0.850530769082291,0.858778905128583,0.906286043966465,0.920200821048477,
0.968991302762396,0.99303553074547,1.),.UNSPECIFIED.);
#246=B_SPLINE_CURVE_WITH_KNOTS('',3,(#51854,#51855,#51856,#51857,#51858,
#51859,#51860,#51861,#51862,#51863,#51864,#51865,#51866,#51867,#51868,#51869,
#51870,#51871,#51872,#51873,#51874,#51875,#51876,#51877,#51878,#51879,#51880,
#51881,#51882,#51883,#51884,#51885,#51886,#51887,#51888,#51889,#51890,#51891,
#51892,#51893,#51894,#51895,#51896,#51897,#51898,#51899,#51900,#51901,#51902,
#51903,#51904,#51905,#51906,#51907,#51908,#51909,#51910,#51911,#51912,#51913,
#51914,#51915,#51916,#51917,#51918,#51919,#51920,#51921,#51922,#51923,#51924,
#51925,#51926,#51927,#51928,#51929,#51930,#51931,#51932,#51933,#51934,#51935,
#51936,#51937,#51938,#51939,#51940,#51941,#51942,#51943,#51944,#51945,#51946,
#51947,#51948,#51949,#51950,#51951,#51952,#51953,#51954,#51955,#51956,#51957,
#51958,#51959,#51960,#51961,#51962,#51963,#51964,#51965,#51966,#51967,#51968,
#51969,#51970,#51971,#51972,#51973,#51974,#51975,#51976,#51977,#51978,#51979,
#51980,#51981,#51982,#51983,#51984,#51985,#51986,#51987,#51988,#51989,#51990,
#51991,#51992,#51993,#51994,#51995,#51996,#51997,#51998,#51999,#52000,#52001,
#52002,#52003,#52004,#52005,#52006,#52007,#52008,#52009,#52010),
 .UNSPECIFIED.,.F.,.F.,(4,3,3,3,3,3,3,3,3,3,3,3,3,3,3,3,3,3,3,3,3,3,3,3,
3,3,3,3,3,3,3,3,3,3,3,3,3,3,3,3,3,3,3,3,3,3,3,3,3,3,3,3,4),(1.72726422180961E-7,
0.0434573104264856,0.0863338408497661,0.0932167342994617,0.125000000000013,
0.165840007447092,0.177273215395186,0.18750000000002,0.218750000000023,
0.234375000000024,0.242187500000025,0.246093750000026,0.249511718750026,
0.250000000000026,0.260113267055131,0.284904699064489,0.309601795003255,
0.312500000000022,0.336932316022879,0.34375000000002,0.359375000000019,
0.359741476131033,0.367187500000018,0.371093750000018,0.373046875000018,
0.374023437500018,0.375000000000018,0.427161996877003,0.437500000000016,
0.446539280842715,0.468750000000016,0.484375000000016,0.492187500000015,
0.49905823116347,0.500000000000015,0.529372684176819,0.595489014668126,
0.601624978392567,0.625000000000013,0.66678708092323,0.687500000000012,
0.718750000000011,0.726755041117905,0.734375000000011,0.746093750000011,
0.750000000000011,0.777565452151945,0.821930738832105,0.864144411482225,
0.906141574496073,0.949726410668509,0.995918599635573,0.999999956010348),
 .UNSPECIFIED.);
#247=B_SPLINE_CURVE_WITH_KNOTS('',3,(#52055,#52056,#52057,#52058,#52059,
#52060,#52061,#52062,#52063,#52064,#52065,#52066,#52067,#52068,#52069,#52070,
#52071,#52072,#52073,#52074,#52075,#52076,#52077,#52078,#52079,#52080,#52081,
#52082,#52083,#52084,#52085),.UNSPECIFIED.,.F.,.F.,(4,3,3,3,3,3,3,3,3,3,
4),(0.,0.124999999999999,0.187499999999999,0.218750000000001,0.234375000000003,
0.242187500000003,0.250000000000002,0.375000000000001,0.5,0.75,1.),
 .UNSPECIFIED.);
#248=B_SPLINE_CURVE_WITH_KNOTS('',3,(#52087,#52088,#52089,#52090,#52091,
#52092,#52093,#52094,#52095,#52096,#52097,#52098,#52099,#52100,#52101,#52102,
#52103,#52104,#52105,#52106,#52107,#52108,#52109,#52110,#52111),
 .UNSPECIFIED.,.F.,.F.,(4,3,3,3,3,3,3,3,4),(0.,0.16666666666665,0.3333333333333,
0.34683559518902,0.517983212474509,0.6666666666667,0.757476212651963,0.908784227355494,
1.),.UNSPECIFIED.);
#249=B_SPLINE_CURVE_WITH_KNOTS('',3,(#52114,#52115,#52116,#52117,#52118,
#52119,#52120,#52121,#52122,#52123,#52124,#52125,#52126,#52127,#52128,#52129,
#52130,#52131,#52132,#52133,#52134,#52135,#52136,#52137,#52138,#52139,#52140,
#52141,#52142,#52143,#52144,#52145,#52146,#52147,#52148,#52149,#52150,#52151,
#52152,#52153,#52154,#52155,#52156,#52157,#52158,#52159,#52160,#52161,#52162,
#52163,#52164,#52165,#52166,#52167,#52168,#52169,#52170,#52171),
 .UNSPECIFIED.,.F.,.F.,(4,3,3,3,3,3,3,3,3,3,3,3,3,3,3,3,3,3,3,4),(0.,0.105109524119636,
0.210219048239273,0.250000000000008,0.34862072745125,0.375000000000012,
0.437500000000015,0.468750000000017,0.484375000000017,0.495049246442063,
0.500000000000017,0.569750769769646,0.637746941740444,0.703349698996779,
0.750000000000009,0.812499999999997,0.86990370050903,0.926035857903304,
0.980615255774514,0.999999999999961),.UNSPECIFIED.);
#250=B_SPLINE_CURVE_WITH_KNOTS('',3,(#52216,#52217,#52218,#52219,#52220,
#52221,#52222,#52223,#52224,#52225,#52226,#52227,#52228,#52229,#52230,#52231,
#52232,#52233,#52234,#52235,#52236,#52237,#52238,#52239,#52240,#52241,#52242,
#52243,#52244,#52245,#52246,#52247,#52248,#52249,#52250,#52251,#52252,#52253,
#52254,#52255,#52256,#52257,#52258,#52259,#52260,#52261,#52262,#52263,#52264,
#52265,#52266,#52267,#52268,#52269,#52270,#52271,#52272,#52273,#52274,#52275,
#52276,#52277,#52278,#52279,#52280,#52281,#52282,#52283,#52284,#52285),
 .UNSPECIFIED.,.F.,.F.,(4,3,3,3,3,3,3,3,3,3,3,3,3,3,3,3,3,3,3,3,3,3,3,4),
(0.,0.0435526678755794,0.0764717462981114,0.120149499615019,0.125,0.178506530376304,
0.223907959984569,0.25,0.31871927758898,0.371577094927995,0.375,0.469063824151086,
0.5,0.519438184278401,0.625,0.667314605350398,0.741711751481222,0.75,0.808035504284208,
0.814958211926088,0.875,0.919742637241602,0.962451077979713,0.999999720285091),
 .UNSPECIFIED.);
#251=B_SPLINE_CURVE_WITH_KNOTS('',3,(#52286,#52287,#52288,#52289,#52290,
#52291,#52292,#52293,#52294,#52295,#52296,#52297,#52298,#52299,#52300,#52301,
#52302,#52303,#52304,#52305,#52306,#52307,#52308,#52309,#52310,#52311,#52312,
#52313,#52314,#52315,#52316,#52317,#52318,#52319,#52320,#52321,#52322,#52323,
#52324,#52325,#52326,#52327,#52328,#52329,#52330,#52331,#52332,#52333,#52334,
#52335,#52336,#52337,#52338,#52339,#52340,#52341,#52342,#52343,#52344,#52345,
#52346,#52347,#52348,#52349,#52350,#52351,#52352,#52353,#52354,#52355),
 .UNSPECIFIED.,.F.,.F.,(4,3,3,3,3,3,3,3,3,3,3,3,3,3,3,3,3,3,3,3,3,3,3,4),
(1.03865533685802E-6,0.0642465706088212,0.129224553569229,0.139648939065381,
0.203364160200743,0.249999999999996,0.300656465499399,0.369078232749696,
0.437499999999993,0.468749999999993,0.469711939585008,0.484374999999993,
0.495154941811767,0.499999999999992,0.563334700450325,0.625630715657075,
0.644015096124142,0.704247231797919,0.749999999999996,0.807879474143196,
0.86848214525923,0.928163112418586,0.961961792804727,0.999999992445085),
 .UNSPECIFIED.);
#252=B_SPLINE_CURVE_WITH_KNOTS('',3,(#52391,#52392,#52393,#52394,#52395,
#52396,#52397,#52398,#52399,#52400,#52401,#52402,#52403,#52404,#52405,#52406,
#52407,#52408,#52409,#52410,#52411,#52412,#52413,#52414,#52415,#52416,#52417,
#52418,#52419,#52420,#52421,#52422,#52423,#52424,#52425,#52426,#52427,#52428,
#52429,#52430,#52431,#52432,#52433,#52434,#52435,#52436,#52437,#52438,#52439,
#52440,#52441,#52442,#52443,#52444,#52445,#52446,#52447,#52448),
 .UNSPECIFIED.,.F.,.F.,(4,3,3,3,3,3,3,3,3,3,3,3,3,3,3,3,3,3,3,4),(1.80896803019825E-6,
0.0702777913312772,0.136276551999961,0.197638148831127,0.25,0.306990176879288,
0.363185832858698,0.419028057645599,0.47449970114341,0.5,0.500063301622431,
0.555684146132839,0.611743964881915,0.668155434484592,0.725242836573191,
0.75,0.812499421639319,0.876725635073414,0.946985306096238,0.999997686557278),
 .UNSPECIFIED.);
#253=B_SPLINE_CURVE_WITH_KNOTS('',3,(#52493,#52494,#52495,#52496,#52497,
#52498,#52499,#52500,#52501,#52502,#52503,#52504,#52505,#52506,#52507,#52508,
#52509,#52510,#52511,#52512,#52513,#52514,#52515,#52516,#52517,#52518,#52519,
#52520,#52521,#52522,#52523,#52524,#52525,#52526,#52527,#52528,#52529,#52530,
#52531,#52532,#52533,#52534,#52535,#52536,#52537,#52538,#52539,#52540,#52541,
#52542,#52543,#52544,#52545,#52546,#52547,#52548,#52549,#52550,#52551,#52552,
#52553,#52554,#52555,#52556,#52557,#52558,#52559,#52560,#52561,#52562,#52563,
#52564,#52565,#52566,#52567,#52568,#52569,#52570,#52571,#52572,#52573,#52574,
#52575,#52576,#52577),.UNSPECIFIED.,.F.,.F.,(4,3,3,3,3,3,3,3,3,3,3,3,3,
3,3,3,3,3,3,3,3,3,3,3,3,3,3,3,4),(3.09998686814312E-6,0.071014663091211,
0.124999999999999,0.187499999999998,0.218749999999998,0.234374999999998,
0.242187499999998,0.246093749999998,0.249999999999998,0.307063177457838,
0.363609740399054,0.40239397193843,0.458356131953603,0.499999999999998,
0.55592354852836,0.61211112871015,0.624999999999998,0.681633993337571,0.687499999999998,
0.718749999999998,0.734374999999998,0.742187499999998,0.746093749999998,
0.749999999999998,0.817242329244051,0.886254599421192,0.923154825582442,
0.994899550913029,0.999994036117558),.UNSPECIFIED.);
#254=B_SPLINE_CURVE_WITH_KNOTS('',3,(#52620,#52621,#52622,#52623,#52624,
#52625,#52626,#52627,#52628,#52629,#52630,#52631,#52632,#52633,#52634,#52635,
#52636,#52637,#52638,#52639,#52640,#52641,#52642,#52643,#52644,#52645,#52646,
#52647,#52648,#52649,#52650,#52651,#52652,#52653,#52654,#52655,#52656,#52657,
#52658,#52659,#52660,#52661,#52662,#52663,#52664,#52665,#52666,#52667,#52668,
#52669,#52670,#52671,#52672,#52673,#52674,#52675,#52676,#52677),
 .UNSPECIFIED.,.F.,.F.,(4,3,3,3,3,3,3,3,3,3,3,3,3,3,3,3,3,3,3,4),(1.9911764389659E-11,
0.0625000000149338,0.123437488775076,0.183435355664403,0.242378549348057,
0.25,0.308039612188458,0.365335670776957,0.422295269231874,0.479061587332518,
0.5357767915656,0.592768342789219,0.649980384244181,0.707849804243744,0.75,
0.808900803033482,0.869149031981107,0.930289648544625,0.992896609496699,
0.999999999969533),.UNSPECIFIED.);
#255=B_SPLINE_CURVE_WITH_KNOTS('',3,(#52679,#52680,#52681,#52682,#52683,
#52684,#52685,#52686,#52687,#52688,#52689,#52690,#52691,#52692,#52693,#52694,
#52695,#52696,#52697,#52698,#52699,#52700),.UNSPECIFIED.,.F.,.F.,(4,3,3,
3,3,3,3,4),(1.5041390606593E-6,0.142631039269413,0.324838433643509,0.5,
0.67989376920272,0.724939089794903,0.90203826115051,0.999999999994462),
 .UNSPECIFIED.);
#256=B_SPLINE_CURVE_WITH_KNOTS('',3,(#52702,#52703,#52704,#52705,#52706,
#52707,#52708,#52709,#52710,#52711,#52712),.UNSPECIFIED.,.F.,.F.,(4,1,2,
2,2,4),(0.,0.124999999999997,0.187499999999997,0.249999999999997,0.499999999999997,
1.),.UNSPECIFIED.);
#257=B_SPLINE_CURVE_WITH_KNOTS('',3,(#52713,#52714,#52715,#52716,#52717,
#52718,#52719,#52720,#52721,#52722,#52723,#52724,#52725,#52726,#52727,#52728,
#52729,#52730,#52731,#52732,#52733,#52734,#52735,#52736,#52737,#52738,#52739,
#52740,#52741,#52742,#52743,#52744,#52745,#52746,#52747,#52748,#52749,#52750,
#52751,#52752,#52753,#52754,#52755,#52756,#52757,#52758,#52759,#52760,#52761,
#52762,#52763,#52764,#52765,#52766,#52767),.UNSPECIFIED.,.F.,.F.,(4,3,3,
3,3,3,3,3,3,3,3,3,3,3,3,3,3,3,4),(0.,0.0650994436402108,0.130198887280422,
0.199793608914402,0.25,0.313473939291271,0.390075348944641,0.437499999999999,
0.468749999999999,0.484374999999998,0.492187499999998,0.498312113050278,
0.499999999999998,0.537870461654632,0.639813161810115,0.71967098213258,
0.82663606314356,0.908057804663619,1.),.UNSPECIFIED.);
#258=B_SPLINE_CURVE_WITH_KNOTS('',3,(#52813,#52814,#52815,#52816,#52817,
#52818,#52819,#52820,#52821,#52822,#52823,#52824,#52825,#52826,#52827,#52828,
#52829,#52830,#52831,#52832,#52833,#52834,#52835,#52836,#52837,#52838,#52839,
#52840,#52841,#52842,#52843,#52844,#52845,#52846,#52847,#52848,#52849,#52850,
#52851,#52852,#52853,#52854,#52855,#52856,#52857,#52858,#52859,#52860,#52861,
#52862,#52863,#52864,#52865,#52866,#52867,#52868,#52869,#52870,#52871,#52872,
#52873,#52874,#52875,#52876,#52877,#52878,#52879,#52880,#52881,#52882,#52883,
#52884,#52885),.UNSPECIFIED.,.F.,.F.,(4,3,3,3,3,3,3,3,3,3,3,3,3,3,3,3,3,
3,3,3,3,3,3,3,4),(1.45421879214282E-9,0.0431191253427652,0.0863267720250147,
0.129382358804927,0.1428571428571,0.153643952151919,0.204633581287644,0.255730997960889,
0.2857142857143,0.306393509456594,0.370923699532922,0.4285714285714,0.45941201799842,
0.526893092898446,0.5714285714286,0.612488429044932,0.677675308974725,0.7142857142857,
0.765391329815468,0.819870817397087,0.8571428571429,0.900979338361016,0.918139369288227,
0.961788840617674,1.),.UNSPECIFIED.);
#259=B_SPLINE_CURVE_WITH_KNOTS('',3,(#52888,#52889,#52890,#52891,#52892,
#52893,#52894,#52895,#52896,#52897,#52898,#52899,#52900,#52901,#52902,#52903,
#52904,#52905,#52906,#52907,#52908,#52909,#52910,#52911,#52912,#52913,#52914,
#52915,#52916,#52917,#52918,#52919,#52920,#52921,#52922,#52923,#52924,#52925,
#52926,#52927,#52928,#52929,#52930,#52931,#52932,#52933,#52934,#52935,#52936,
#52937,#52938,#52939,#52940,#52941,#52942,#52943,#52944,#52945,#52946,#52947,
#52948,#52949,#52950,#52951,#52952,#52953,#52954,#52955,#52956,#52957,#52958,
#52959,#52960),.UNSPECIFIED.,.F.,.F.,(4,3,3,3,3,3,3,3,3,3,3,3,3,3,3,3,3,
3,3,3,3,3,3,3,4),(0.,0.0558892582289014,0.112669247781944,0.156953381452509,
0.215052185968344,0.249999999999993,0.309316249815091,0.32431076563434,
0.38539095426848,0.437499999999988,0.468749999999988,0.484374999999988,
0.492187499999988,0.498949390062523,0.499999999999988,0.504583453135758,
0.573408356689112,0.64134333511677,0.680145776021464,0.749999999999994,
0.815926291102209,0.847891300901525,0.914668851233571,0.980715804659358,
1.),.UNSPECIFIED.);
#260=B_SPLINE_CURVE_WITH_KNOTS('',3,(#53059,#53060,#53061,#53062,#53063,
#53064,#53065,#53066,#53067,#53068,#53069,#53070,#53071,#53072,#53073,#53074,
#53075,#53076,#53077,#53078,#53079,#53080,#53081,#53082,#53083,#53084,#53085,
#53086,#53087,#53088,#53089,#53090,#53091,#53092,#53093,#53094,#53095,#53096,
#53097,#53098,#53099,#53100,#53101,#53102,#53103,#53104,#53105,#53106,#53107,
#53108,#53109,#53110,#53111,#53112,#53113,#53114,#53115,#53116,#53117,#53118,
#53119,#53120,#53121,#53122,#53123,#53124,#53125,#53126,#53127,#53128,#53129,
#53130,#53131,#53132,#53133,#53134,#53135,#53136,#53137,#53138,#53139,#53140,
#53141,#53142,#53143,#53144,#53145,#53146,#53147,#53148,#53149,#53150,#53151,
#53152,#53153,#53154,#53155,#53156,#53157,#53158,#53159,#53160,#53161,#53162,
#53163,#53164,#53165,#53166,#53167,#53168,#53169,#53170,#53171,#53172,#53173,
#53174,#53175,#53176,#53177,#53178,#53179,#53180,#53181,#53182,#53183,#53184,
#53185,#53186,#53187,#53188,#53189,#53190,#53191,#53192,#53193,#53194,#53195,
#53196,#53197,#53198,#53199,#53200,#53201,#53202,#53203,#53204,#53205,#53206,
#53207,#53208,#53209,#53210,#53211,#53212,#53213,#53214,#53215,#53216,#53217,
#53218,#53219,#53220,#53221,#53222,#53223,#53224),.UNSPECIFIED.,.F.,.F.,
(4,3,3,3,3,3,3,3,3,3,3,3,3,3,3,3,3,3,3,3,3,3,3,3,3,3,3,3,3,3,3,3,3,3,3,
3,3,3,3,3,3,3,3,3,3,3,3,3,3,3,3,3,3,3,3,4),(8.91633426931597E-8,0.0341866200056338,
0.0624999999999992,0.0800113026486996,0.0937499999999987,0.109374999999998,
0.117187499999998,0.121093749999998,0.123046874999998,0.124999999999998,
0.156875028251668,0.1875,0.218750000000001,0.234375000000001,0.237518692308383,
0.242187500000002,0.246093750000002,0.248046875000002,0.250000000000002,
0.290850977675925,0.312500000000002,0.328922102328694,0.343750000000002,
0.359375000000002,0.367187500000002,0.371093750000002,0.373046875000002,
0.375000000000002,0.425211651263262,0.437500000000002,0.468750000000001,
0.484375000000001,0.492187500000001,0.496093750000001,0.500000000000001,
0.520156881115364,0.572597422442347,0.616913355571128,0.625000000000001,
0.651328060847,0.678222159827132,0.6875,0.709176140839145,0.75,0.78125,
0.7890625,0.796875,0.799086910217881,0.8125,0.858396212816867,0.875,0.885500856062245,
0.932686341515045,0.980790797833406,0.98573188374278,1.),.UNSPECIFIED.);
#261=B_SPLINE_CURVE_WITH_KNOTS('',3,(#53227,#53228,#53229,#53230,#53231,
#53232,#53233,#53234,#53235,#53236,#53237,#53238,#53239,#53240,#53241,#53242,
#53243,#53244,#53245,#53246,#53247,#53248,#53249,#53250,#53251,#53252,#53253,
#53254,#53255,#53256,#53257,#53258,#53259,#53260,#53261,#53262,#53263,#53264,
#53265,#53266,#53267,#53268,#53269,#53270,#53271,#53272,#53273,#53274,#53275,
#53276,#53277,#53278,#53279,#53280,#53281,#53282,#53283,#53284,#53285,#53286,
#53287,#53288,#53289,#53290,#53291,#53292,#53293,#53294,#53295,#53296,#53297,
#53298,#53299,#53300,#53301,#53302,#53303,#53304,#53305,#53306,#53307,#53308,
#53309,#53310,#53311,#53312,#53313,#53314,#53315,#53316,#53317,#53318,#53319,
#53320,#53321,#53322,#53323,#53324,#53325,#53326,#53327,#53328,#53329,#53330,
#53331,#53332,#53333,#53334,#53335,#53336,#53337,#53338,#53339,#53340,#53341,
#53342,#53343,#53344,#53345,#53346,#53347,#53348,#53349,#53350,#53351,#53352,
#53353,#53354,#53355,#53356,#53357,#53358,#53359,#53360,#53361,#53362,#53363,
#53364,#53365,#53366,#53367,#53368),.UNSPECIFIED.,.F.,.F.,(4,3,3,3,3,3,
3,3,3,3,3,3,3,3,3,3,3,3,3,3,3,3,3,3,3,3,3,3,3,3,3,3,3,3,3,3,3,3,3,3,3,3,
3,3,3,3,3,4),(2.34638000429566E-7,0.0315958252999231,0.0628964643186087,
0.0937122453289208,0.10417220844182,0.124999999999999,0.154837292802782,
0.184674585605564,0.213175902892385,0.218749999999999,0.234374999999999,
0.242187499999999,0.246093749999999,0.248046874999998,0.249999999999998,
0.257790527710696,0.295642545408796,0.334483525618913,0.354334856151428,
0.392683149567989,0.431398866791145,0.470481924430731,0.482377267678491,
0.484375000000002,0.496585772826167,0.500000000000002,0.540377617471143,
0.58037233206427,0.609455371445993,0.649166188301461,0.687500000000005,
0.700832172402015,0.718750000000005,0.734375000000005,0.742187500000005,
0.746093750000005,0.748046875000005,0.750000000000005,0.769091706308904,
0.79896691623487,0.828842126160835,0.858577033135406,0.875000000000003,
0.89678232603399,0.927914261958254,0.959582462922759,0.985641707998622,
1.),.UNSPECIFIED.);
#262=B_SPLINE_CURVE_WITH_KNOTS('',3,(#53405,#53406,#53407,#53408,#53409,
#53410,#53411,#53412,#53413,#53414,#53415,#53416,#53417,#53418,#53419,#53420,
#53421,#53422,#53423,#53424,#53425,#53426,#53427,#53428,#53429,#53430,#53431,
#53432,#53433,#53434,#53435,#53436,#53437,#53438,#53439,#53440,#53441,#53442,
#53443,#53444,#53445,#53446,#53447,#53448,#53449,#53450,#53451,#53452,#53453,
#53454,#53455,#53456,#53457,#53458,#53459,#53460,#53461,#53462,#53463,#53464,
#53465),.UNSPECIFIED.,.F.,.F.,(4,3,3,3,3,3,3,3,3,3,3,3,3,3,3,3,3,3,3,3,
4),(3.81436863215028E-8,0.0594692241135463,0.119461332976601,0.180335226693879,
0.228233297279517,0.25,0.3125,0.375,0.420627166446326,0.466475792531788,
0.500000000000001,0.532982594262802,0.595584209629977,0.657507055367544,
0.718468272244316,0.75,0.809830564880495,0.831293963743825,0.890887057024469,
0.949594063922645,0.999999999994814),.UNSPECIFIED.);
#263=B_SPLINE_CURVE_WITH_KNOTS('',3,(#53466,#53467,#53468,#53469,#53470,
#53471,#53472,#53473,#53474,#53475,#53476,#53477,#53478,#53479,#53480,#53481,
#53482,#53483,#53484,#53485,#53486,#53487,#53488,#53489,#53490,#53491,#53492,
#53493,#53494,#53495,#53496,#53497,#53498,#53499,#53500,#53501,#53502,#53503,
#53504,#53505,#53506,#53507,#53508,#53509,#53510,#53511,#53512,#53513,#53514,
#53515,#53516,#53517,#53518,#53519,#53520,#53521,#53522,#53523),
 .UNSPECIFIED.,.F.,.F.,(4,3,3,3,3,3,3,3,3,3,3,3,3,3,3,3,3,3,3,4),(0.,0.0707847540439358,
0.13714897876124,0.19876944030244,0.25,0.307617673205022,0.364360156798302,
0.42070510310328,0.476621035240063,0.49999980758445,0.5,0.555639382305717,
0.611765726333174,0.668272106356441,0.72549762942489,0.75,0.812499999999486,
0.877170052799808,0.948088545219367,0.999999999997942),.UNSPECIFIED.);
#264=B_SPLINE_CURVE_WITH_KNOTS('',3,(#53562,#53563,#53564,#53565,#53566,
#53567,#53568,#53569,#53570,#53571,#53572,#53573,#53574,#53575,#53576,#53577,
#53578,#53579,#53580,#53581,#53582,#53583,#53584,#53585,#53586,#53587,#53588,
#53589,#53590,#53591,#53592,#53593,#53594,#53595,#53596,#53597,#53598,#53599,
#53600,#53601,#53602,#53603,#53604,#53605,#53606,#53607,#53608,#53609,#53610,
#53611,#53612,#53613,#53614,#53615,#53616,#53617,#53618,#53619,#53620,#53621,
#53622,#53623,#53624,#53625,#53626,#53627,#53628,#53629,#53630,#53631,#53632,
#53633,#53634,#53635,#53636,#53637,#53638,#53639,#53640,#53641,#53642,#53643),
 .UNSPECIFIED.,.F.,.F.,(4,3,3,3,3,3,3,3,3,3,3,3,3,3,3,3,3,3,3,3,3,3,3,3,
3,3,3,4),(0.,0.0792150655842689,0.124999999999999,0.125921017487507,0.187499999999999,
0.218749999999999,0.234374999999999,0.242187499999999,0.248597221451861,
0.249999999999999,0.312515849372989,0.385046619809545,0.457415846192531,
0.499988433043988,0.499999999999998,0.570823904390727,0.624999999999998,
0.687466106592308,0.687499999999998,0.718749999999998,0.734374999999998,
0.742187499999998,0.748633296290449,0.749999999999998,0.823394013248657,
0.874049304626543,0.94994762549464,1.),.UNSPECIFIED.);
#265=B_SPLINE_CURVE_WITH_KNOTS('',3,(#53682,#53683,#53684,#53685,#53686,
#53687,#53688,#53689,#53690,#53691,#53692,#53693,#53694,#53695,#53696,#53697,
#53698,#53699,#53700,#53701,#53702,#53703,#53704,#53705,#53706,#53707,#53708,
#53709,#53710,#53711,#53712),.UNSPECIFIED.,.F.,.F.,(4,3,3,3,3,3,3,3,3,3,
4),(0.,0.124999999999982,0.187499999999974,0.218749999999971,0.234374999999969,
0.242187499999969,0.249999999999969,0.374999999999973,0.499999999999977,
0.749999999999989,1.),.UNSPECIFIED.);
#266=B_SPLINE_CURVE_WITH_KNOTS('',3,(#53713,#53714,#53715,#53716,#53717,
#53718,#53719,#53720,#53721,#53722,#53723,#53724,#53725,#53726,#53727,#53728,
#53729,#53730,#53731,#53732,#53733,#53734),.UNSPECIFIED.,.F.,.F.,(4,3,3,
3,3,3,3,4),(0.,0.177024512090844,0.292989167962771,0.472837133506511,0.5,
0.689142403121388,0.878284806242776,0.999997308150379),.UNSPECIFIED.);
#267=B_SPLINE_CURVE_WITH_KNOTS('',3,(#53735,#53736,#53737,#53738,#53739,
#53740,#53741,#53742,#53743,#53744,#53745,#53746,#53747,#53748,#53749,#53750,
#53751,#53752,#53753,#53754,#53755,#53756,#53757,#53758,#53759,#53760,#53761,
#53762,#53763,#53764,#53765,#53766,#53767,#53768,#53769,#53770,#53771,#53772,
#53773,#53774,#53775,#53776,#53777,#53778,#53779,#53780,#53781,#53782,#53783,
#53784,#53785,#53786,#53787,#53788,#53789,#53790,#53791,#53792,#53793,#53794,
#53795),.UNSPECIFIED.,.F.,.F.,(4,3,3,3,3,3,3,3,3,3,3,3,3,3,3,3,3,3,3,3,
4),(0.,0.0976856521887196,0.205020687001143,0.250000000000006,0.286357328179635,
0.375000000000008,0.437500000000008,0.467815798455655,0.468750000000008,
0.484375000000007,0.492187500000007,0.497983320289822,0.500000000000006,
0.581183162361599,0.657948135640541,0.692880023009447,0.750000000000003,
0.820238740768344,0.874892120286855,0.9403090323846,0.999999999888379),
 .UNSPECIFIED.);
#268=B_SPLINE_CURVE_WITH_KNOTS('',3,(#53838,#53839,#53840,#53841,#53842,
#53843,#53844,#53845,#53846,#53847,#53848,#53849,#53850,#53851,#53852,#53853,
#53854,#53855,#53856,#53857,#53858,#53859,#53860,#53861,#53862,#53863,#53864,
#53865,#53866,#53867,#53868,#53869,#53870,#53871,#53872,#53873,#53874,#53875,
#53876,#53877,#53878,#53879,#53880,#53881,#53882,#53883,#53884,#53885,#53886,
#53887,#53888,#53889,#53890,#53891,#53892,#53893,#53894,#53895,#53896,#53897,
#53898,#53899,#53900,#53901,#53902,#53903,#53904,#53905,#53906,#53907,#53908,
#53909,#53910,#53911,#53912,#53913,#53914,#53915,#53916,#53917,#53918,#53919,
#53920,#53921,#53922,#53923,#53924,#53925,#53926,#53927,#53928),
 .UNSPECIFIED.,.F.,.F.,(4,3,3,3,3,3,3,3,3,3,3,3,3,3,3,3,3,3,3,3,3,3,3,3,
3,3,3,3,3,3,4),(1.98871583907149E-7,0.0470903211130683,0.0950886099489182,
0.109526542541016,0.125000000000008,0.176685447236339,0.187500000000013,
0.19557488232977,0.203125000000014,0.218750000000014,0.250000000000015,
0.27062164890649,0.3341041042639,0.398265330724908,0.430414683829977,0.437500000000016,
0.468750000000016,0.484375000000016,0.492187500000016,0.49803412523616,
0.500000000000016,0.559924707782723,0.6001249554854,0.658475264874343,0.715889345308872,
0.764250567674328,0.821849981037566,0.878616147063133,0.918178967654373,
0.970962443959493,1.),.UNSPECIFIED.);
#269=B_SPLINE_CURVE_WITH_KNOTS('',3,(#53973,#53974,#53975,#53976,#53977,
#53978,#53979,#53980,#53981,#53982,#53983,#53984,#53985,#53986,#53987,#53988,
#53989,#53990,#53991,#53992,#53993,#53994,#53995,#53996,#53997,#53998,#53999,
#54000,#54001,#54002,#54003,#54004,#54005,#54006,#54007,#54008,#54009,#54010,
#54011,#54012,#54013,#54014,#54015,#54016,#54017,#54018,#54019,#54020,#54021,
#54022,#54023,#54024,#54025,#54026,#54027,#54028,#54029,#54030),
 .UNSPECIFIED.,.F.,.F.,(4,3,3,3,3,3,3,3,3,3,3,3,3,3,3,3,3,3,3,4),(0.,0.0625,
0.123437357561668,0.183435176402664,0.242378391891801,0.25,0.308040053618873,
0.365336549014984,0.422296583768566,0.479063340059895,0.535778986169599,
0.592770982238121,0.6499834721799,0.707853330673838,0.75,0.808902290745458,
0.869152098427341,0.930294379921426,0.992903114983252,1.),.UNSPECIFIED.);
#270=B_SPLINE_CURVE_WITH_KNOTS('',3,(#54032,#54033,#54034,#54035,#54036,
#54037,#54038,#54039,#54040,#54041,#54042,#54043,#54044,#54045,#54046,#54047,
#54048,#54049,#54050,#54051,#54052,#54053,#54054,#54055,#54056),
 .UNSPECIFIED.,.F.,.F.,(4,3,3,3,3,3,3,3,4),(1.330406108134E-6,0.181643406415568,
0.207927514662845,0.390638495071313,0.5,0.679764878140392,0.772661902357852,
0.949922356290452,1.),.UNSPECIFIED.);
#271=B_SPLINE_CURVE_WITH_KNOTS('',3,(#54058,#54059,#54060,#54061,#54062,
#54063,#54064,#54065,#54066,#54067,#54068,#54069,#54070),.UNSPECIFIED.,
 .F.,.F.,(4,3,3,3,4),(0.,0.187500000000001,0.250000000000001,0.500000000000001,
1.),.UNSPECIFIED.);
#272=B_SPLINE_CURVE_WITH_KNOTS('',3,(#54071,#54072,#54073,#54074,#54075,
#54076,#54077,#54078,#54079,#54080,#54081,#54082,#54083,#54084,#54085,#54086,
#54087,#54088,#54089,#54090,#54091,#54092,#54093,#54094,#54095,#54096,#54097,
#54098,#54099,#54100,#54101,#54102,#54103,#54104,#54105,#54106,#54107,#54108,
#54109,#54110,#54111,#54112,#54113,#54114,#54115,#54116,#54117,#54118,#54119,
#54120,#54121,#54122,#54123,#54124,#54125,#54126,#54127,#54128,#54129,#54130,
#54131,#54132,#54133,#54134,#54135,#54136,#54137,#54138,#54139,#54140,#54141,
#54142,#54143,#54144,#54145,#54146,#54147,#54148,#54149),.UNSPECIFIED.,
 .F.,.F.,(4,3,3,3,3,3,3,3,3,3,3,3,3,3,3,3,3,3,3,3,3,3,3,3,3,3,4),(1.45817479409027E-11,
0.00165012278096161,0.0447426246888551,0.0904394296673588,0.124999999999989,
0.158030392352972,0.187499999999984,0.218749999999981,0.23437499999998,
0.242187499999982,0.246093749999983,0.248046874999984,0.249999999999984,
0.335606080067904,0.366241870352233,0.374999999999973,0.437499999999968,
0.468749999999966,0.484374999999965,0.495318580094463,0.499999999999964,
0.553856462622792,0.656803820681865,0.736020610771133,0.84337533284278,
0.922615832922426,0.999999999885346),.UNSPECIFIED.);
#273=B_SPLINE_CURVE_WITH_KNOTS('',3,(#54191,#54192,#54193,#54194,#54195,
#54196,#54197,#54198,#54199,#54200,#54201,#54202,#54203,#54204,#54205,#54206,
#54207,#54208,#54209,#54210,#54211,#54212,#54213,#54214,#54215,#54216,#54217,
#54218,#54219,#54220,#54221,#54222,#54223,#54224,#54225,#54226,#54227,#54228,
#54229,#54230,#54231,#54232,#54233,#54234,#54235,#54236,#54237,#54238,#54239,
#54240,#54241,#54242,#54243,#54244,#54245,#54246,#54247,#54248,#54249,#54250,
#54251,#54252,#54253,#54254,#54255,#54256,#54257,#54258,#54259,#54260,#54261,
#54262,#54263,#54264,#54265,#54266,#54267,#54268,#54269,#54270,#54271,#54272,
#54273,#54274,#54275,#54276,#54277,#54278),.UNSPECIFIED.,.F.,.F.,(4,3,3,
3,3,3,3,3,3,3,3,3,3,3,3,3,3,3,3,3,3,3,3,3,3,3,3,3,3,4),(0.,0.0527820104074715,
0.0818213323246725,0.138473115952622,0.195945212509441,0.235750029132872,
0.293012176753044,0.351193392797035,0.39987544901493,0.437500000000017,
0.468750000000018,0.484375000000019,0.492187500000019,0.496093750000018,
0.499508594500751,0.500000000000018,0.565860735166544,0.629574768817817,
0.693958667104365,0.72575099412064,0.781250000000005,0.790730854104752,
0.796875000000005,0.812500000000005,0.869043334984336,0.875000000000003,
0.884835783967175,0.938700818461981,0.993360674255924,0.999999777750421),
 .UNSPECIFIED.);
#274=B_SPLINE_CURVE_WITH_KNOTS('',3,(#54281,#54282,#54283,#54284,#54285,
#54286,#54287,#54288,#54289,#54290,#54291,#54292,#54293,#54294,#54295,#54296,
#54297,#54298,#54299,#54300,#54301,#54302,#54303,#54304,#54305,#54306,#54307,
#54308,#54309,#54310,#54311,#54312,#54313,#54314,#54315,#54316,#54317,#54318,
#54319,#54320,#54321,#54322,#54323,#54324,#54325,#54326,#54327,#54328,#54329,
#54330,#54331,#54332,#54333,#54334,#54335,#54336,#54337,#54338),
 .UNSPECIFIED.,.F.,.F.,(4,3,3,3,3,3,3,3,3,3,3,3,3,3,3,3,3,3,3,4),(0.,0.0585630956581098,
0.11799660785587,0.16870786218184,0.228541511703754,0.250000000000001,0.312500000000001,
0.375000000000001,0.421054231074681,0.467108462149362,0.500000000000001,
0.563532899274307,0.626399529047779,0.688223246127237,0.750000000000001,
0.771768823660319,0.832605857581761,0.892881416492703,0.95230696880294,
0.999999961863694),.UNSPECIFIED.);
#275=B_SPLINE_CURVE_WITH_KNOTS('',3,(#54389,#54390,#54391,#54392,#54393,
#54394,#54395,#54396,#54397,#54398,#54399,#54400,#54401,#54402,#54403,#54404,
#54405,#54406,#54407,#54408,#54409,#54410,#54411,#54412,#54413,#54414,#54415,
#54416,#54417,#54418,#54419,#54420,#54421,#54422,#54423,#54424,#54425,#54426,
#54427,#54428,#54429,#54430,#54431,#54432,#54433,#54434,#54435,#54436,#54437,
#54438,#54439,#54440,#54441,#54442,#54443,#54444,#54445,#54446,#54447,#54448,
#54449,#54450,#54451,#54452,#54453,#54454,#54455,#54456,#54457,#54458,#54459,
#54460,#54461,#54462,#54463,#54464,#54465,#54466,#54467,#54468,#54469,#54470,
#54471,#54472,#54473,#54474,#54475,#54476,#54477,#54478,#54479,#54480,#54481,
#54482,#54483,#54484,#54485,#54486,#54487,#54488,#54489,#54490,#54491,#54492,
#54493,#54494,#54495,#54496,#54497,#54498,#54499,#54500,#54501,#54502,#54503,
#54504,#54505,#54506,#54507,#54508,#54509,#54510,#54511,#54512,#54513,#54514,
#54515,#54516,#54517,#54518,#54519,#54520,#54521,#54522,#54523,#54524,#54525,
#54526,#54527,#54528,#54529,#54530,#54531,#54532,#54533,#54534,#54535,#54536,
#54537,#54538,#54539,#54540,#54541,#54542,#54543,#54544,#54545,#54546,#54547,
#54548,#54549,#54550,#54551,#54552,#54553,#54554,#54555,#54556,#54557,#54558,
#54559,#54560,#54561,#54562,#54563,#54564,#54565,#54566,#54567,#54568,#54569,
#54570,#54571,#54572,#54573,#54574,#54575,#54576,#54577,#54578,#54579,#54580,
#54581,#54582,#54583,#54584,#54585,#54586,#54587,#54588,#54589,#54590,#54591,
#54592,#54593,#54594,#54595,#54596,#54597,#54598,#54599,#54600,#54601,#54602,
#54603,#54604,#54605,#54606,#54607,#54608,#54609,#54610,#54611,#54612,#54613,
#54614,#54615,#54616,#54617,#54618,#54619,#54620,#54621,#54622,#54623,#54624,
#54625,#54626,#54627,#54628,#54629,#54630,#54631,#54632),.UNSPECIFIED.,
 .F.,.F.,(4,3,3,3,3,3,3,3,3,3,3,3,3,3,3,3,3,3,3,3,3,3,3,3,3,3,3,3,3,3,3,
3,3,3,3,3,3,3,3,3,3,3,3,3,3,3,3,3,3,3,3,3,3,3,3,3,3,3,3,3,3,3,3,3,3,3,3,
3,3,3,3,3,3,3,3,3,3,3,3,3,3,4),(9.74885373639512E-8,0.0159200062587186,
0.031250000000024,0.0468750000000361,0.0546875000000421,0.0585937500000451,
0.0625000000000481,0.064860891737383,0.0837424297147262,0.10256194718207,
0.109375000000083,0.117187500000089,0.121093750000092,0.123046875000094,
0.124023437500095,0.124511718750095,0.125000000000095,0.13088113283216,
0.145623338057796,0.160279740929913,0.171875000000121,0.179687500000125,
0.183593750000127,0.185546875000129,0.186523437500129,0.18750000000013,
0.198322293578093,0.209103043160817,0.213452349241984,0.224198983077635,
0.234874954929346,0.242187500000162,0.246093750000164,0.248046875000165,
0.249023437500166,0.249755859375166,0.250000000000166,0.28612814128228,
0.331147428104677,0.373117414619281,0.413995852027384,0.437500000000167,
0.442038759562938,0.468750000000167,0.484375000000167,0.492187500000167,
0.496093750000167,0.498046875000167,0.4988073956278,0.499023437500167,0.499511718750167,
0.500000000000167,0.527809511524871,0.55563689272658,0.580222745701537,
0.608292500450986,0.634707899177733,0.640625000000145,0.645734470948701,
0.648437500000144,0.665746275460254,0.677886474696675,0.695389033000862,
0.712977553082935,0.73065498180394,0.734375000000131,0.74218750000013,0.74609375000013,
0.74804687500013,0.74902343750013,0.74951171875013,0.750000000000129,0.752487431508907,
0.797977655326278,0.804136709370455,0.850539439908008,0.858789251719635,
0.906288880937672,0.920205788064523,0.968988607968507,0.993036230187174,
1.),.UNSPECIFIED.);
#276=B_SPLINE_CURVE_WITH_KNOTS('',3,(#54715,#54716,#54717,#54718,#54719,
#54720,#54721,#54722,#54723,#54724,#54725,#54726,#54727,#54728,#54729,#54730,
#54731,#54732,#54733,#54734,#54735,#54736,#54737,#54738,#54739,#54740,#54741,
#54742,#54743,#54744,#54745,#54746,#54747,#54748,#54749,#54750,#54751,#54752,
#54753,#54754,#54755,#54756,#54757,#54758,#54759,#54760,#54761,#54762,#54763,
#54764,#54765,#54766,#54767,#54768,#54769,#54770,#54771,#54772,#54773,#54774,
#54775,#54776,#54777,#54778,#54779,#54780,#54781,#54782,#54783,#54784,#54785,
#54786,#54787,#54788,#54789,#54790,#54791,#54792,#54793,#54794,#54795,#54796,
#54797,#54798,#54799,#54800,#54801,#54802,#54803,#54804,#54805,#54806,#54807,
#54808,#54809,#54810,#54811,#54812,#54813,#54814,#54815,#54816,#54817,#54818,
#54819,#54820,#54821,#54822,#54823,#54824,#54825,#54826,#54827,#54828,#54829,
#54830,#54831,#54832,#54833,#54834,#54835,#54836,#54837,#54838,#54839,#54840,
#54841,#54842,#54843,#54844,#54845,#54846,#54847,#54848,#54849,#54850,#54851,
#54852,#54853,#54854,#54855,#54856,#54857,#54858,#54859,#54860,#54861,#54862,
#54863,#54864,#54865,#54866,#54867,#54868,#54869,#54870,#54871),
 .UNSPECIFIED.,.F.,.F.,(4,3,3,3,3,3,3,3,3,3,3,3,3,3,3,3,3,3,3,3,3,3,3,3,
3,3,3,3,3,3,3,3,3,3,3,3,3,3,3,3,3,3,3,3,3,3,3,3,3,3,3,3,4),(1.72726440594495E-7,
0.0434573132527648,0.0863338474990505,0.093216517716401,0.124999999999985,
0.165840010670402,0.177272924303734,0.187499999999978,0.218749999999974,
0.234374999999973,0.242187499999972,0.246093749999971,0.249511718749971,
0.249999999999971,0.260112842122813,0.284904275703955,0.309601373157129,
0.312499999999974,0.336932316158668,0.343749999999976,0.359374999999977,
0.359741421885534,0.367187499999977,0.371093749999978,0.373046874999978,
0.374023437499978,0.374999999999978,0.427162028762236,0.437499999999979,
0.446539513801691,0.468749999999979,0.48437499999998,0.49218749999998,0.499058235380736,
0.49999999999998,0.529373135558955,0.595489465840445,0.60162559917597,0.624999999999982,
0.666787835011797,0.687499999999983,0.718749999999984,0.726755886335632,
0.734374999999984,0.746093749999984,0.749999999999985,0.777566191164044,
0.821931417214387,0.864144998210834,0.906142061394322,0.949726796380935,
0.995918874659696,0.999999956010456),.UNSPECIFIED.);
#277=B_SPLINE_CURVE_WITH_KNOTS('',3,(#54916,#54917,#54918,#54919,#54920,
#54921,#54922,#54923,#54924,#54925,#54926,#54927,#54928,#54929,#54930,#54931,
#54932,#54933,#54934,#54935,#54936,#54937,#54938,#54939,#54940,#54941,#54942,
#54943,#54944,#54945,#54946),.UNSPECIFIED.,.F.,.F.,(4,3,3,3,3,3,3,3,3,3,
4),(0.,0.125000000000019,0.187500000000028,0.218750000000032,0.234375000000033,
0.242187500000033,0.250000000000033,0.375000000000028,0.500000000000022,
0.750000000000011,1.),.UNSPECIFIED.);
#278=B_SPLINE_CURVE_WITH_KNOTS('',3,(#54948,#54949,#54950,#54951,#54952,
#54953,#54954,#54955,#54956,#54957,#54958,#54959,#54960,#54961,#54962,#54963,
#54964,#54965,#54966,#54967,#54968,#54969,#54970,#54971,#54972),
 .UNSPECIFIED.,.F.,.F.,(4,3,3,3,3,3,3,3,4),(0.,0.177282336143491,0.213907941281364,
0.393665915351053,0.5,0.682805729838532,0.77695616943279,0.958668461365049,
0.999998980185047),.UNSPECIFIED.);
#279=B_SPLINE_CURVE_WITH_KNOTS('',3,(#54974,#54975,#54976,#54977,#54978,
#54979,#54980,#54981,#54982,#54983,#54984,#54985,#54986,#54987,#54988,#54989,
#54990,#54991,#54992,#54993,#54994,#54995,#54996,#54997,#54998,#54999,#55000,
#55001,#55002,#55003,#55004,#55005,#55006,#55007,#55008,#55009,#55010,#55011,
#55012,#55013,#55014,#55015,#55016,#55017,#55018,#55019,#55020,#55021,#55022,
#55023,#55024,#55025,#55026,#55027,#55028,#55029,#55030,#55031,#55032,#55033,
#55034),.UNSPECIFIED.,.F.,.F.,(4,3,3,3,3,3,3,3,3,3,3,3,3,3,3,3,3,3,3,3,
4),(5.73167048359177E-11,0.0625000000429875,0.123430758022991,0.183422273868319,
0.24235958000366,0.25,0.308040146146061,0.365368965521203,0.422365343403545,
0.479130682341562,0.5,0.55673209842876,0.61379107282782,0.671113553585964,
0.729073370544327,0.75,0.808901353783578,0.869150170975925,0.930291454539829,
0.992899267799122,1.),.UNSPECIFIED.);
#280=B_SPLINE_CURVE_WITH_KNOTS('',3,(#55035,#55036,#55037,#55038,#55039,
#55040,#55041,#55042,#55043,#55044,#55045,#55046,#55047,#55048,#55049,#55050,
#55051,#55052,#55053,#55054,#55055,#55056,#55057,#55058,#55059,#55060,#55061,
#55062,#55063,#55064,#55065,#55066,#55067,#55068,#55069,#55070,#55071,#55072,
#55073,#55074,#55075,#55076,#55077,#55078,#55079,#55080,#55081,#55082,#55083,
#55084,#55085,#55086,#55087,#55088,#55089,#55090,#55091,#55092,#55093,#55094,
#55095,#55096,#55097,#55098,#55099,#55100,#55101,#55102,#55103,#55104),
 .UNSPECIFIED.,.F.,.F.,(4,3,3,3,3,3,3,3,3,3,3,3,3,3,3,3,3,3,3,3,3,3,3,4),
(1.15604835473446E-10,0.072945956146836,0.180557791681298,0.25000000000002,
0.259407485718546,0.362622524995456,0.437500000000034,0.441690815636676,
0.468750000000037,0.484375000000039,0.492187500000039,0.498125154992541,
0.500000000000039,0.580027879028248,0.655074895560498,0.660055758056458,
0.732990214315364,0.75000000000002,0.818419921927436,0.849001518755108,
0.914551347658443,0.976944079464395,0.994828975829166,1.),.UNSPECIFIED.);
#281=B_SPLINE_CURVE_WITH_KNOTS('',3,(#55149,#55150,#55151,#55152,#55153,
#55154,#55155,#55156,#55157,#55158,#55159,#55160,#55161,#55162,#55163,#55164,
#55165,#55166,#55167,#55168,#55169,#55170,#55171,#55172,#55173,#55174,#55175,
#55176,#55177,#55178,#55179,#55180,#55181,#55182,#55183,#55184,#55185,#55186,
#55187,#55188,#55189,#55190,#55191,#55192,#55193,#55194,#55195,#55196,#55197,
#55198,#55199,#55200,#55201,#55202,#55203,#55204,#55205,#55206,#55207,#55208,
#55209,#55210,#55211,#55212,#55213,#55214,#55215,#55216,#55217,#55218),
 .UNSPECIFIED.,.F.,.F.,(4,3,3,3,3,3,3,3,3,3,3,3,3,3,3,3,3,3,3,3,3,3,3,4),
(0.,0.0435551679386673,0.076470578260204,0.120151332451966,0.125,0.178532794167066,
0.223906562246117,0.25,0.318743929132965,0.371576002742637,0.375,0.469091817166418,
0.5,0.519437350326105,0.625,0.667314026802467,0.7417108943593,0.75,0.808035583839871,
0.814957891431279,0.875,0.919742711947922,0.962451012488657,0.999999720284603),
 .UNSPECIFIED.);
#282=B_SPLINE_CURVE_WITH_KNOTS('',3,(#55219,#55220,#55221,#55222,#55223,
#55224,#55225,#55226,#55227,#55228,#55229,#55230,#55231,#55232,#55233,#55234,
#55235,#55236,#55237,#55238,#55239,#55240,#55241,#55242,#55243,#55244,#55245,
#55246,#55247,#55248,#55249,#55250,#55251,#55252,#55253,#55254,#55255,#55256,
#55257,#55258,#55259,#55260,#55261,#55262,#55263,#55264,#55265,#55266,#55267,
#55268,#55269,#55270,#55271,#55272,#55273,#55274,#55275,#55276,#55277,#55278,
#55279,#55280,#55281,#55282,#55283,#55284,#55285,#55286,#55287,#55288),
 .UNSPECIFIED.,.F.,.F.,(4,3,3,3,3,3,3,3,3,3,3,3,3,3,3,3,3,3,3,3,3,3,3,4),
(0.,0.0642452018256955,0.129223022111387,0.139648916649683,0.203363964417562,
0.250000000000005,0.300656440952451,0.36907822047623,0.43750000000001,0.468750000000011,
0.469711915463756,0.484375000000011,0.495154959267717,0.500000000000011,
0.563334722729026,0.625630761231619,0.644015065163845,0.704247224853198,
0.750000000000005,0.807879449656103,0.8684821469436,0.928163140833693,0.961961786669929,
0.999999992443035),.UNSPECIFIED.);
#283=B_SPLINE_CURVE_WITH_KNOTS('',3,(#55324,#55325,#55326,#55327,#55328,
#55329,#55330,#55331,#55332,#55333,#55334,#55335,#55336,#55337,#55338,#55339,
#55340,#55341,#55342,#55343,#55344,#55345,#55346,#55347,#55348,#55349,#55350,
#55351,#55352,#55353,#55354,#55355,#55356,#55357,#55358,#55359,#55360,#55361,
#55362,#55363,#55364,#55365,#55366,#55367,#55368,#55369,#55370,#55371,#55372,
#55373,#55374,#55375,#55376,#55377,#55378,#55379,#55380,#55381),
 .UNSPECIFIED.,.F.,.F.,(4,3,3,3,3,3,3,3,3,3,3,3,3,3,3,3,3,3,3,4),(0.,0.0339753543803814,
0.109950566125709,0.168097066017028,0.245117177635656,0.25,0.324143694588969,
0.40341117828457,0.483062939160984,0.5,0.500074284948893,0.580013729768816,
0.658971793933605,0.676028229049525,0.75,0.826841345162694,0.832059158171015,
0.907853033409699,0.966136292621797,1.),.UNSPECIFIED.);
#284=B_SPLINE_CURVE_WITH_KNOTS('',3,(#55426,#55427,#55428,#55429,#55430,
#55431,#55432,#55433,#55434,#55435,#55436,#55437,#55438,#55439,#55440,#55441,
#55442,#55443,#55444,#55445,#55446,#55447,#55448,#55449,#55450,#55451,#55452,
#55453,#55454,#55455,#55456,#55457,#55458,#55459,#55460,#55461,#55462,#55463,
#55464,#55465,#55466,#55467,#55468,#55469,#55470,#55471,#55472,#55473,#55474,
#55475,#55476,#55477,#55478,#55479,#55480,#55481,#55482,#55483,#55484,#55485,
#55486,#55487,#55488,#55489,#55490,#55491,#55492,#55493,#55494,#55495,#55496,
#55497,#55498,#55499,#55500,#55501,#55502,#55503,#55504,#55505,#55506,#55507,
#55508,#55509,#55510,#55511,#55512,#55513,#55514,#55515,#55516),
 .UNSPECIFIED.,.F.,.F.,(4,3,3,3,3,3,3,3,3,3,3,3,3,3,3,3,3,3,3,3,3,3,3,3,
3,3,3,3,3,3,4),(0.,0.0388645141120945,0.125000000000002,0.187500000000003,
0.190146043466364,0.218750000000003,0.234375000000003,0.242187500000003,
0.246093750000004,0.248046875000004,0.250000000000004,0.315771796321043,
0.342916849517666,0.407904968457705,0.472592506143607,0.499999999999999,
0.500065465413701,0.563235050528544,0.624999999999997,0.657214404683583,
0.687499999999995,0.718749999999995,0.734374999999995,0.742187499999994,
0.746093749999994,0.748046874999994,0.749999999999994,0.809981507440316,
0.896400830417988,0.961249318093161,1.),.UNSPECIFIED.);
#285=B_SPLINE_CURVE_WITH_KNOTS('',3,(#55555,#55556,#55557,#55558,#55559,
#55560,#55561,#55562,#55563,#55564,#55565,#55566,#55567,#55568,#55569,#55570,
#55571,#55572,#55573,#55574,#55575,#55576,#55577,#55578,#55579,#55580,#55581,
#55582,#55583,#55584,#55585,#55586,#55587,#55588,#55589,#55590,#55591,#55592,
#55593,#55594,#55595,#55596,#55597,#55598,#55599,#55600,#55601,#55602,#55603,
#55604,#55605,#55606,#55607,#55608,#55609,#55610,#55611,#55612),
 .UNSPECIFIED.,.F.,.F.,(4,3,3,3,3,3,3,3,3,3,3,3,3,3,3,3,3,3,3,4),(0.,0.0625,
0.123436056759143,0.18343260413623,0.24237460068037,0.25,0.308039776325257,
0.365335998405921,0.422295761702448,0.479062247404443,0.535777622950034,
0.592769350027535,0.649981570270837,0.70785116671443,0.75,0.808902110291868,
0.869151749075464,0.930293857117356,0.992902397598166,1.),.UNSPECIFIED.);
#286=B_SPLINE_CURVE_WITH_KNOTS('',3,(#55614,#55615,#55616,#55617,#55618,
#55619),.UNSPECIFIED.,.F.,.F.,(4,1,1,4),(1.40740795308042E-6,0.3333333333333,
0.6666666666667,1.),.UNSPECIFIED.);
#287=B_SPLINE_CURVE_WITH_KNOTS('',3,(#55621,#55622,#55623,#55624,#55625,
#55626,#55627,#55628,#55629,#55630,#55631,#55632,#55633),.UNSPECIFIED.,
 .F.,.F.,(4,3,3,3,4),(0.,0.1875,0.249999999999999,0.499999999999999,1.),
 .UNSPECIFIED.);
#288=B_SPLINE_CURVE_WITH_KNOTS('',3,(#55634,#55635,#55636,#55637,#55638,
#55639,#55640,#55641,#55642,#55643,#55644,#55645,#55646,#55647,#55648,#55649,
#55650,#55651,#55652,#55653,#55654,#55655,#55656,#55657,#55658,#55659,#55660,
#55661,#55662,#55663,#55664,#55665,#55666,#55667,#55668,#55669,#55670,#55671,
#55672,#55673,#55674,#55675,#55676,#55677,#55678,#55679,#55680,#55681,#55682,
#55683,#55684,#55685,#55686,#55687,#55688),.UNSPECIFIED.,.F.,.F.,(4,3,3,
3,3,3,3,3,3,3,3,3,3,3,3,3,3,3,4),(0.,0.0642483351342427,0.123631513668559,
0.192521447460844,0.250000000000009,0.313929035664213,0.389698805114818,
0.437500000000014,0.468750000000015,0.484375000000016,0.492187500000016,
0.49892305110334,0.500000000000016,0.532968101520917,0.640208044354892,
0.723028006675871,0.834863768936946,0.918219616793671,0.999999999866653),
 .UNSPECIFIED.);
#289=B_SPLINE_CURVE_WITH_KNOTS('',3,(#55734,#55735,#55736,#55737,#55738,
#55739,#55740,#55741,#55742,#55743,#55744,#55745,#55746,#55747,#55748,#55749,
#55750,#55751,#55752,#55753,#55754,#55755,#55756,#55757,#55758,#55759,#55760,
#55761,#55762,#55763,#55764,#55765,#55766,#55767,#55768,#55769,#55770,#55771,
#55772,#55773,#55774,#55775,#55776,#55777,#55778,#55779,#55780,#55781,#55782,
#55783,#55784,#55785,#55786,#55787,#55788,#55789,#55790,#55791,#55792,#55793,
#55794,#55795,#55796,#55797,#55798,#55799,#55800,#55801,#55802,#55803,#55804,
#55805,#55806),.UNSPECIFIED.,.F.,.F.,(4,3,3,3,3,3,3,3,3,3,3,3,3,3,3,3,3,
3,3,3,3,3,3,3,4),(1.45391862059565E-9,0.0431123241756327,0.086313162635294,
0.129361940668342,0.1428571428571,0.153622397531604,0.204599352639357,0.255684060316847,
0.2857142857143,0.306350448882393,0.37080198399618,0.4285714285714,0.459347099296346,
0.526502746439944,0.5714285714286,0.612403504379262,0.676567149297245,0.7142857142857,
0.76527664382255,0.818292079191637,0.8571428571429,0.90081416683432,0.918050451477613,
0.961569312477636,1.),.UNSPECIFIED.);
#290=B_SPLINE_CURVE_WITH_KNOTS('',3,(#55809,#55810,#55811,#55812,#55813,
#55814,#55815,#55816,#55817,#55818,#55819,#55820,#55821,#55822,#55823,#55824,
#55825,#55826,#55827,#55828,#55829,#55830,#55831,#55832,#55833,#55834,#55835,
#55836,#55837,#55838,#55839,#55840,#55841,#55842,#55843,#55844,#55845,#55846,
#55847,#55848,#55849,#55850,#55851,#55852,#55853,#55854,#55855,#55856,#55857,
#55858,#55859,#55860,#55861,#55862,#55863,#55864,#55865,#55866,#55867,#55868,
#55869,#55870,#55871,#55872,#55873,#55874,#55875,#55876,#55877,#55878,#55879,
#55880,#55881),.UNSPECIFIED.,.F.,.F.,(4,3,3,3,3,3,3,3,3,3,3,3,3,3,3,3,3,
3,3,3,3,3,3,3,4),(0.,0.0558892574716291,0.112669246806468,0.156953409715992,
0.215052214168376,0.250000000000006,0.309316250654647,0.324310832507047,
0.385391022398012,0.43750000000001,0.46875000000001,0.48437500000001,0.49218750000001,
0.498949346899948,0.50000000000001,0.504583563377448,0.573408589202907,
0.641343695284019,0.680145783129569,0.750000000000005,0.815926487813902,
0.847891275365318,0.914669007590066,0.98071621931426,1.),.UNSPECIFIED.);
#291=B_SPLINE_CURVE_WITH_KNOTS('',3,(#55980,#55981,#55982,#55983,#55984,
#55985,#55986,#55987,#55988,#55989,#55990,#55991,#55992,#55993,#55994,#55995,
#55996,#55997,#55998,#55999,#56000,#56001,#56002,#56003,#56004,#56005,#56006,
#56007,#56008,#56009,#56010,#56011,#56012,#56013,#56014,#56015,#56016,#56017,
#56018,#56019,#56020,#56021,#56022,#56023,#56024,#56025,#56026,#56027,#56028,
#56029,#56030,#56031,#56032,#56033,#56034,#56035,#56036,#56037,#56038,#56039,
#56040,#56041,#56042,#56043,#56044,#56045,#56046,#56047,#56048,#56049,#56050,
#56051,#56052,#56053,#56054,#56055,#56056,#56057,#56058,#56059,#56060,#56061,
#56062,#56063,#56064,#56065,#56066,#56067,#56068,#56069,#56070,#56071,#56072,
#56073,#56074,#56075,#56076,#56077,#56078,#56079,#56080,#56081,#56082,#56083,
#56084,#56085,#56086,#56087,#56088,#56089,#56090,#56091,#56092,#56093,#56094,
#56095,#56096,#56097,#56098,#56099,#56100,#56101,#56102,#56103,#56104,#56105,
#56106,#56107,#56108,#56109,#56110,#56111,#56112,#56113,#56114,#56115,#56116,
#56117,#56118,#56119,#56120,#56121,#56122,#56123,#56124,#56125,#56126,#56127,
#56128,#56129,#56130,#56131,#56132,#56133,#56134,#56135,#56136,#56137,#56138,
#56139,#56140,#56141,#56142,#56143,#56144,#56145),.UNSPECIFIED.,.F.,.F.,
(4,3,3,3,3,3,3,3,3,3,3,3,3,3,3,3,3,3,3,3,3,3,3,3,3,3,3,3,3,3,3,3,3,3,3,
3,3,3,3,3,3,3,3,3,3,3,3,3,3,3,3,3,3,3,3,4),(8.91632442143459E-8,0.0341866199909269,
0.0625000000000018,0.0800113026638258,0.0937500000000027,0.109375000000003,
0.117187500000003,0.121093750000003,0.123046875000003,0.125000000000003,
0.156875028287151,0.187500000000004,0.218750000000004,0.234375000000004,
0.237518692323063,0.242187500000004,0.246093750000004,0.248046875000004,
0.250000000000004,0.290850977616787,0.312500000000003,0.328922102341607,
0.343750000000002,0.359375000000002,0.367187500000002,0.371093750000002,
0.373046875000002,0.375000000000002,0.425211651225354,0.437500000000001,
0.468750000000001,0.484375,0.4921875,0.49609375,0.5,0.520156881116544,0.572597422472742,
0.616913355572735,0.624999999999999,0.651328060799945,0.678222159731897,
0.687499999999998,0.709176140832686,0.749999999999997,0.781249999999997,
0.789062499999997,0.796874999999997,0.799086910214249,0.812499999999997,
0.858396212764482,0.874999999999998,0.885500856041081,0.93268634150154,
0.980790797824736,0.985731883736702,1.),.UNSPECIFIED.);
#292=B_SPLINE_CURVE_WITH_KNOTS('',3,(#56148,#56149,#56150,#56151,#56152,
#56153,#56154,#56155,#56156,#56157,#56158,#56159,#56160,#56161,#56162,#56163,
#56164,#56165,#56166,#56167,#56168,#56169,#56170,#56171,#56172,#56173,#56174,
#56175,#56176,#56177,#56178,#56179,#56180,#56181,#56182,#56183,#56184,#56185,
#56186,#56187,#56188,#56189,#56190,#56191,#56192,#56193,#56194,#56195,#56196,
#56197,#56198,#56199,#56200,#56201,#56202,#56203,#56204,#56205,#56206,#56207,
#56208,#56209,#56210,#56211,#56212,#56213,#56214,#56215,#56216,#56217,#56218,
#56219,#56220,#56221,#56222,#56223,#56224,#56225,#56226,#56227,#56228,#56229,
#56230,#56231,#56232,#56233,#56234,#56235,#56236,#56237,#56238,#56239,#56240,
#56241,#56242,#56243,#56244,#56245,#56246,#56247,#56248,#56249,#56250,#56251,
#56252,#56253,#56254,#56255,#56256,#56257,#56258,#56259,#56260,#56261,#56262,
#56263,#56264,#56265,#56266,#56267,#56268,#56269,#56270,#56271,#56272,#56273,
#56274,#56275,#56276,#56277,#56278,#56279,#56280,#56281,#56282,#56283,#56284,
#56285,#56286,#56287,#56288,#56289),.UNSPECIFIED.,.F.,.F.,(4,3,3,3,3,3,
3,3,3,3,3,3,3,3,3,3,3,3,3,3,3,3,3,3,3,3,3,3,3,3,3,3,3,3,3,3,3,3,3,3,3,3,
3,3,3,3,3,4),(2.34637983009399E-7,0.0315958275913751,0.0628964688330882,
0.093712252016794,0.104172203871702,0.124999999999996,0.154837291401328,
0.184674582802659,0.213175902159575,0.218749999999994,0.234374999999994,
0.242187499999993,0.246093749999993,0.248046874999993,0.249999999999993,
0.257790527886997,0.295642547232279,0.334483529193173,0.354334857867753,
0.39268315304614,0.431398872128228,0.470481931727138,0.482377268318766,
0.484374999999996,0.496585777244764,0.499999999999997,0.540377617220931,
0.580372331573253,0.609455371665288,0.649166188311503,0.687499999999999,
0.700832172519671,0.718749999999999,0.734375,0.7421875,0.74609375,0.748046875,
0.75,0.769091705922879,0.798966915348658,0.828842124774437,0.858577030826336,
0.875,0.896782324096875,0.927914259072886,0.959582459056515,0.985641707363427,
1.),.UNSPECIFIED.);
#293=B_SPLINE_CURVE_WITH_KNOTS('',3,(#56326,#56327,#56328,#56329,#56330,
#56331,#56332,#56333,#56334,#56335,#56336,#56337,#56338,#56339,#56340,#56341,
#56342,#56343,#56344,#56345,#56346,#56347,#56348,#56349,#56350,#56351,#56352,
#56353,#56354,#56355,#56356,#56357,#56358,#56359,#56360,#56361,#56362,#56363,
#56364,#56365,#56366,#56367,#56368,#56369,#56370,#56371,#56372,#56373,#56374,
#56375,#56376,#56377,#56378,#56379,#56380,#56381,#56382,#56383,#56384,#56385,
#56386),.UNSPECIFIED.,.F.,.F.,(4,3,3,3,3,3,3,3,3,3,3,3,3,3,3,3,3,3,3,3,
4),(3.81436950412107E-8,0.0594692249681252,0.119461334964787,0.180335230433945,
0.228233343725019,0.25,0.3125,0.375,0.420629521267839,0.466480442658904,
0.5,0.532982688308766,0.595584374784075,0.657507294105254,0.718468589090622,
0.75,0.809830707906453,0.831293941004929,0.890887152636801,0.949594326669872,
1.),.UNSPECIFIED.);
#294=B_SPLINE_CURVE_WITH_KNOTS('',3,(#56387,#56388,#56389,#56390,#56391,
#56392,#56393,#56394,#56395,#56396,#56397,#56398,#56399,#56400,#56401,#56402,
#56403,#56404,#56405,#56406,#56407,#56408,#56409,#56410,#56411,#56412,#56413,
#56414,#56415,#56416,#56417,#56418,#56419,#56420,#56421,#56422,#56423,#56424,
#56425,#56426,#56427,#56428,#56429,#56430,#56431,#56432,#56433,#56434,#56435,
#56436,#56437,#56438,#56439,#56440,#56441,#56442,#56443,#56444),
 .UNSPECIFIED.,.F.,.F.,(4,3,3,3,3,3,3,3,3,3,3,3,3,3,3,3,3,3,3,4),(0.,0.070136586784253,
0.13603270626599,0.197319690970826,0.25,0.307828697463722,0.364809836743389,
0.421408542734098,0.477602898251202,0.5,0.500034296737292,0.555640241024459,
0.611682773460639,0.668075486783373,0.72514215037561,0.75,0.8125,0.876717029865349,
0.946961303728935,1.),.UNSPECIFIED.);
#295=B_SPLINE_CURVE_WITH_KNOTS('',3,(#56490,#56491,#56492,#56493,#56494,
#56495,#56496,#56497,#56498,#56499,#56500,#56501,#56502,#56503,#56504,#56505,
#56506,#56507,#56508,#56509,#56510,#56511,#56512,#56513,#56514,#56515,#56516,
#56517,#56518,#56519,#56520,#56521,#56522,#56523,#56524,#56525,#56526,#56527,
#56528,#56529,#56530,#56531,#56532,#56533,#56534,#56535,#56536,#56537,#56538,
#56539,#56540,#56541,#56542,#56543,#56544,#56545,#56546,#56547),
 .UNSPECIFIED.,.F.,.F.,(4,3,3,3,3,3,3,3,3,3,3,3,3,3,3,3,3,3,3,4),(0.,0.0625,
0.123429142320394,0.183419124217513,0.242355039406308,0.25,0.308040957847518,
0.365338354022302,0.422299301931396,0.479066994233144,0.535783605802587,
0.592776604825274,0.64999011865553,0.70786098943061,0.75,0.808903052638457,
0.869153547680589,0.930296449526362,0.992905654827065,1.),.UNSPECIFIED.);
#296=B_SPLINE_CURVE_WITH_KNOTS('',3,(#56548,#56549,#56550,#56551,#56552,
#56553,#56554,#56555,#56556,#56557,#56558,#56559,#56560,#56561,#56562,#56563,
#56564,#56565,#56566,#56567,#56568,#56569,#56570,#56571,#56572,#56573,#56574,
#56575,#56576,#56577,#56578,#56579,#56580,#56581,#56582,#56583,#56584,#56585,
#56586,#56587,#56588,#56589,#56590,#56591,#56592,#56593,#56594,#56595,#56596,
#56597,#56598,#56599,#56600,#56601,#56602,#56603,#56604,#56605,#56606,#56607,
#56608,#56609,#56610,#56611,#56612,#56613,#56614,#56615,#56616,#56617,#56618,
#56619,#56620,#56621,#56622,#56623,#56624,#56625,#56626,#56627,#56628,#56629,
#56630,#56631,#56632,#56633,#56634,#56635,#56636,#56637,#56638,#56639,#56640,
#56641,#56642,#56643,#56644),.UNSPECIFIED.,.F.,.F.,(4,3,3,3,3,3,3,3,3,3,
3,3,3,3,3,3,3,3,3,3,3,3,3,3,3,3,3,3,3,3,3,3,4),(0.,0.00285452287324627,
0.0810898927209212,0.124999999999997,0.163513621542303,0.187499999999996,
0.218749999999995,0.234374999999995,0.242187499999995,0.246093749999995,
0.248046874999995,0.249999999999995,0.316063805229939,0.331496676299031,
0.396932120474405,0.461480984752616,0.499909644740874,0.499999999999995,
0.563689652381694,0.624999999999995,0.668335900347379,0.687499999999995,
0.718749999999995,0.734374999999995,0.742187499999995,0.746093749999995,
0.748046874999995,0.749999999999995,0.826034220731771,0.836305307418583,
0.916645663493165,0.996986019567746,1.),.UNSPECIFIED.);
#297=B_SPLINE_CURVE_WITH_KNOTS('',3,(#56683,#56684,#56685,#56686,#56687,
#56688,#56689,#56690,#56691,#56692,#56693,#56694,#56695,#56696,#56697,#56698,
#56699,#56700,#56701,#56702,#56703,#56704,#56705,#56706,#56707,#56708,#56709,
#56710,#56711,#56712,#56713),.UNSPECIFIED.,.F.,.F.,(4,3,3,3,3,3,3,3,3,3,
4),(0.,0.124999999999991,0.187499999999986,0.218749999999983,0.234374999999982,
0.242187499999982,0.249999999999982,0.374999999999986,0.49999999999999,
0.749999999999995,1.),.UNSPECIFIED.);
#298=B_SPLINE_CURVE_WITH_KNOTS('',3,(#56714,#56715,#56716,#56717,#56718,
#56719),.UNSPECIFIED.,.F.,.F.,(4,1,1,4),(0.,0.3333333333333,0.6666666666667,
0.999998328036297),.UNSPECIFIED.);
#299=B_SPLINE_CURVE_WITH_KNOTS('',3,(#56720,#56721,#56722,#56723,#56724,
#56725,#56726,#56727,#56728,#56729,#56730,#56731,#56732,#56733,#56734,#56735,
#56736,#56737,#56738,#56739,#56740,#56741,#56742,#56743,#56744,#56745,#56746,
#56747,#56748,#56749,#56750,#56751,#56752,#56753,#56754,#56755,#56756,#56757,
#56758,#56759,#56760,#56761,#56762,#56763,#56764,#56765,#56766,#56767,#56768,
#56769,#56770,#56771,#56772,#56773,#56774,#56775,#56776,#56777,#56778,#56779,
#56780),.UNSPECIFIED.,.F.,.F.,(4,3,3,3,3,3,3,3,3,3,3,3,3,3,3,3,3,3,3,3,
4),(1.03820017360987E-10,0.0858140043459224,0.198337968205613,0.250000000000019,
0.281117634573999,0.37500000000003,0.437500000000035,0.468750000000038,
0.471374013083689,0.484375000000041,0.492187500000042,0.498687480577556,
0.500000000000043,0.57969855306797,0.655204256162074,0.69128810718509,0.750000000000021,
0.819024361205775,0.881081173000778,0.945467811578077,0.999999999939057),
 .UNSPECIFIED.);
#300=B_SPLINE_CURVE_WITH_KNOTS('',3,(#56823,#56824,#56825,#56826,#56827,
#56828,#56829,#56830,#56831,#56832,#56833,#56834,#56835,#56836,#56837,#56838,
#56839,#56840,#56841,#56842,#56843,#56844,#56845,#56846,#56847,#56848,#56849,
#56850,#56851,#56852,#56853,#56854,#56855,#56856,#56857,#56858,#56859,#56860,
#56861,#56862,#56863,#56864,#56865,#56866,#56867,#56868,#56869,#56870,#56871,
#56872,#56873,#56874,#56875,#56876,#56877,#56878,#56879,#56880,#56881,#56882,
#56883,#56884,#56885,#56886,#56887,#56888,#56889,#56890,#56891,#56892,#56893,
#56894,#56895,#56896,#56897,#56898,#56899,#56900,#56901,#56902,#56903,#56904,
#56905,#56906,#56907,#56908,#56909,#56910,#56911,#56912,#56913),
 .UNSPECIFIED.,.F.,.F.,(4,3,3,3,3,3,3,3,3,3,3,3,3,3,3,3,3,3,3,3,3,3,3,3,
3,3,3,3,3,3,4),(1.98906479309072E-7,0.047089838900463,0.0950876593119024,
0.109526425869498,0.124999999999998,0.176684953882968,0.187499999999997,
0.195574839395448,0.203124999999996,0.218749999999996,0.249999999999996,
0.270621648562703,0.334104108208607,0.398265338859945,0.430414683614596,
0.4375,0.46875,0.484375000000001,0.492187500000001,0.498034123720945,0.500000000000001,
0.55992470032944,0.600124960067209,0.658475261666886,0.7158893297449,0.764250575765468,
0.821849980430899,0.878616137371232,0.918178973503123,0.970962441134751,
1.),.UNSPECIFIED.);
#301=B_SPLINE_CURVE_WITH_KNOTS('',3,(#56956,#56957,#56958,#56959,#56960,
#56961,#56962,#56963,#56964,#56965,#56966,#56967,#56968,#56969,#56970,#56971,
#56972,#56973,#56974,#56975,#56976,#56977),.UNSPECIFIED.,.F.,.F.,(4,3,3,
3,3,3,3,4),(1.63033535856655E-6,0.120934032136536,0.310467016068268,0.5,
0.679851327939551,0.7064121488131,0.883436743746198,1.),.UNSPECIFIED.);
#302=B_SPLINE_CURVE_WITH_KNOTS('',3,(#56979,#56980,#56981,#56982,#56983,
#56984,#56985,#56986,#56987,#56988,#56989),.UNSPECIFIED.,.F.,.F.,(4,1,2,
2,2,4),(0.,0.125,0.1875,0.249999999999999,0.5,1.),.UNSPECIFIED.);
#303=B_SPLINE_CURVE_WITH_KNOTS('',3,(#56990,#56991,#56992,#56993,#56994,
#56995,#56996,#56997,#56998,#56999,#57000,#57001,#57002,#57003,#57004,#57005,
#57006,#57007,#57008,#57009,#57010,#57011,#57012,#57013,#57014,#57015,#57016,
#57017,#57018,#57019,#57020,#57021,#57022,#57023,#57024,#57025,#57026,#57027,
#57028,#57029,#57030,#57031,#57032,#57033,#57034,#57035,#57036,#57037,#57038,
#57039,#57040,#57041,#57042,#57043,#57044),.UNSPECIFIED.,.F.,.F.,(4,3,3,
3,3,3,3,3,3,3,3,3,3,3,3,3,3,3,4),(0.,0.0654580192943895,0.124936971683619,
0.19521642709056,0.250000000000039,0.306913925251286,0.384160992342502,
0.437500000000067,0.468750000000071,0.484375000000072,0.492187500000071,
0.498304651669469,0.50000000000007,0.531997336482634,0.633294429777801,
0.713452211844485,0.819820113326127,0.902138636668165,1.),.UNSPECIFIED.);
#304=B_SPLINE_CURVE_WITH_KNOTS('',3,(#57086,#57087,#57088,#57089,#57090,
#57091,#57092,#57093,#57094,#57095,#57096,#57097,#57098,#57099,#57100,#57101,
#57102,#57103,#57104,#57105,#57106,#57107,#57108,#57109,#57110,#57111,#57112,
#57113,#57114,#57115,#57116,#57117,#57118,#57119,#57120,#57121,#57122,#57123,
#57124,#57125,#57126,#57127,#57128,#57129,#57130,#57131,#57132,#57133,#57134,
#57135,#57136,#57137,#57138,#57139,#57140,#57141,#57142,#57143,#57144,#57145,
#57146,#57147,#57148,#57149,#57150,#57151,#57152,#57153,#57154,#57155,#57156,
#57157,#57158,#57159,#57160,#57161,#57162,#57163,#57164,#57165,#57166,#57167,
#57168,#57169,#57170,#57171,#57172,#57173),.UNSPECIFIED.,.F.,.F.,(4,3,3,
3,3,3,3,3,3,3,3,3,3,3,3,3,3,3,3,3,3,3,3,3,3,3,3,3,3,4),(1.09807446774891E-11,
0.0527820137222502,0.0818213359279545,0.138473123221553,0.195945223360734,
0.235750033133544,0.293012182826601,0.35119340202972,0.399875450857417,
0.437499999999998,0.468749999999998,0.484374999999998,0.492187499999998,
0.496093749999998,0.499508594759178,0.499999999999998,0.565860735503257,
0.629574778776911,0.693958686436161,0.725750994255272,0.781250000000002,
0.790730855827748,0.796875000000002,0.812500000000002,0.8690433465425,0.875000000000002,
0.884835785766576,0.938700830850611,0.993360696887802,0.999999777750431),
 .UNSPECIFIED.);
#305=B_SPLINE_CURVE_WITH_KNOTS('',3,(#57176,#57177,#57178,#57179,#57180,
#57181,#57182,#57183,#57184,#57185,#57186,#57187,#57188,#57189,#57190,#57191,
#57192,#57193,#57194,#57195,#57196,#57197,#57198,#57199,#57200,#57201,#57202,
#57203,#57204,#57205,#57206,#57207,#57208,#57209,#57210,#57211,#57212,#57213,
#57214,#57215,#57216,#57217,#57218,#57219,#57220,#57221,#57222,#57223,#57224,
#57225,#57226,#57227,#57228,#57229,#57230,#57231,#57232,#57233),
 .UNSPECIFIED.,.F.,.F.,(4,3,3,3,3,3,3,3,3,3,3,3,3,3,3,3,3,3,3,4),(1.3581547160307E-11,
0.0585628517632844,0.117996194021253,0.168707832741241,0.228541288466462,
0.25,0.3125,0.375,0.421054296540944,0.467108593081889,0.5,0.563532895370386,
0.62639952166682,0.68822323587103,0.75,0.771768878138407,0.832605908968213,
0.892881465150608,0.952307015390897,0.999999961863706),.UNSPECIFIED.);
#306=B_SPLINE_CURVE_WITH_KNOTS('',3,(#57284,#57285,#57286,#57287,#57288,
#57289,#57290,#57291,#57292,#57293,#57294,#57295,#57296,#57297,#57298,#57299,
#57300,#57301,#57302,#57303,#57304,#57305,#57306,#57307,#57308,#57309,#57310,
#57311,#57312,#57313,#57314,#57315,#57316,#57317,#57318,#57319,#57320,#57321,
#57322,#57323,#57324,#57325,#57326,#57327,#57328,#57329,#57330,#57331,#57332,
#57333,#57334,#57335,#57336,#57337,#57338,#57339,#57340,#57341,#57342,#57343,
#57344,#57345,#57346,#57347,#57348,#57349,#57350,#57351,#57352,#57353,#57354,
#57355,#57356,#57357,#57358,#57359,#57360,#57361,#57362,#57363,#57364,#57365,
#57366,#57367,#57368,#57369,#57370,#57371,#57372,#57373,#57374,#57375,#57376,
#57377,#57378,#57379,#57380,#57381,#57382,#57383,#57384,#57385,#57386,#57387,
#57388,#57389,#57390,#57391,#57392,#57393,#57394,#57395,#57396,#57397,#57398,
#57399,#57400,#57401,#57402,#57403,#57404,#57405,#57406,#57407,#57408,#57409,
#57410,#57411,#57412,#57413,#57414,#57415,#57416,#57417,#57418,#57419,#57420,
#57421,#57422,#57423,#57424,#57425,#57426,#57427,#57428,#57429,#57430,#57431,
#57432,#57433,#57434,#57435,#57436,#57437,#57438,#57439,#57440,#57441,#57442,
#57443,#57444,#57445,#57446,#57447,#57448,#57449,#57450,#57451,#57452,#57453,
#57454,#57455,#57456,#57457,#57458,#57459,#57460,#57461,#57462,#57463,#57464,
#57465,#57466,#57467,#57468,#57469,#57470,#57471,#57472,#57473,#57474,#57475,
#57476,#57477,#57478,#57479,#57480,#57481,#57482,#57483,#57484,#57485,#57486,
#57487,#57488,#57489,#57490,#57491,#57492,#57493,#57494,#57495,#57496,#57497,
#57498,#57499,#57500,#57501,#57502,#57503,#57504,#57505,#57506,#57507,#57508,
#57509,#57510,#57511,#57512,#57513,#57514,#57515,#57516,#57517,#57518,#57519,
#57520,#57521,#57522,#57523,#57524),.UNSPECIFIED.,.F.,.F.,(4,3,3,3,3,3,
3,3,3,3,3,3,3,3,3,3,3,3,3,3,3,3,3,3,3,3,3,3,3,3,3,3,3,3,3,3,3,3,3,3,3,3,
3,3,3,3,3,3,3,3,3,3,3,3,3,3,3,3,3,3,3,3,3,3,3,3,3,3,3,3,3,3,3,3,3,3,3,3,
3,3,4),(9.74886797225189E-8,0.0159200057310286,0.0312500000000033,0.0468750000000049,
0.0546875000000058,0.0585937500000062,0.0625000000000067,0.0648608916794454,
0.0837424285003968,0.10256194479458,0.109375000000012,0.117187500000013,
0.121093750000014,0.123046875000014,0.124023437500014,0.124511718750014,
0.125000000000014,0.130881132752826,0.145623337610177,0.160279740114716,
0.171875000000021,0.179687500000022,0.183593750000023,0.185546875000023,
0.186523437500023,0.187500000000023,0.198322293156087,0.209103042320687,
0.21345235022535,0.224198983639946,0.234874955076149,0.242187500000008,
0.246093750000007,0.248046875000007,0.249023437500007,0.249755859375006,
0.250000000000006,0.286128141198425,0.331147428259678,0.373117414469576,
0.413937461021449,0.442038759456119,0.468750000000021,0.484375000000022,
0.492187500000022,0.496093750000022,0.498046875000023,0.498807395625069,
0.499023437500023,0.499511718750023,0.500000000000023,0.527809509355821,
0.555636888410823,0.580222747550704,0.608292500146189,0.634707899498602,
0.64062500000002,0.645734467803367,0.64843750000002,0.665746267512998,0.677886461833895,
0.695389012135111,0.712977524146475,0.730654944749156,0.734375000000017,
0.742187500000017,0.746093750000017,0.748046875000017,0.749023437500017,
0.749511718750016,0.750000000000016,0.752487431440223,0.79797765669168,
0.804136709872947,0.850539441899368,0.858789252586812,0.906288883068206,
0.920205788951179,0.968988610235553,0.993036230319091,1.),.UNSPECIFIED.);
#307=B_SPLINE_CURVE_WITH_KNOTS('',3,(#57607,#57608,#57609,#57610,#57611,
#57612,#57613,#57614,#57615,#57616,#57617,#57618,#57619,#57620,#57621,#57622,
#57623,#57624,#57625,#57626,#57627,#57628,#57629,#57630,#57631,#57632,#57633,
#57634,#57635,#57636,#57637,#57638,#57639,#57640,#57641,#57642,#57643,#57644,
#57645,#57646,#57647,#57648,#57649,#57650,#57651,#57652,#57653,#57654,#57655,
#57656,#57657,#57658,#57659,#57660,#57661,#57662,#57663,#57664,#57665,#57666,
#57667,#57668,#57669,#57670,#57671,#57672,#57673,#57674,#57675,#57676,#57677,
#57678,#57679,#57680,#57681,#57682,#57683,#57684,#57685,#57686,#57687,#57688,
#57689,#57690,#57691,#57692,#57693,#57694,#57695,#57696,#57697,#57698,#57699,
#57700,#57701,#57702,#57703,#57704,#57705,#57706,#57707,#57708,#57709,#57710,
#57711,#57712,#57713,#57714,#57715,#57716,#57717,#57718,#57719,#57720,#57721,
#57722,#57723,#57724,#57725,#57726,#57727,#57728,#57729,#57730,#57731,#57732,
#57733,#57734,#57735,#57736,#57737,#57738,#57739,#57740,#57741,#57742,#57743,
#57744,#57745,#57746,#57747,#57748,#57749,#57750,#57751,#57752,#57753,#57754,
#57755,#57756,#57757,#57758,#57759,#57760,#57761,#57762,#57763),
 .UNSPECIFIED.,.F.,.F.,(4,3,3,3,3,3,3,3,3,3,3,3,3,3,3,3,3,3,3,3,3,3,3,3,
3,3,3,3,3,3,3,3,3,3,3,3,3,3,3,3,3,3,3,3,3,3,3,3,3,3,3,3,4),(1.72726420505883E-7,
0.0434573133218831,0.0863338476385245,0.0932165176868182,0.124999999999984,
0.165840010671867,0.177272924281379,0.187499999999975,0.218749999999971,
0.234374999999969,0.242187499999968,0.246093749999968,0.249511718749968,
0.249999999999968,0.260112843085009,0.284904274190472,0.309601369212814,
0.312499999999972,0.336932313817438,0.343749999999975,0.359374999999976,
0.359741422647275,0.367187499999977,0.371093749999977,0.373046874999977,
0.374023437499977,0.374999999999977,0.427161994615482,0.43749999999998,
0.446539510208758,0.468749999999981,0.484374999999982,0.492187499999982,
0.499058230973304,0.499999999999982,0.529373135558788,0.59548946583794,
0.601625599175875,0.624999999999987,0.666787835011863,0.687499999999989,
0.718749999999991,0.726755886335713,0.734374999999991,0.746093749999992,
0.749999999999992,0.777566191087922,0.821931417049227,0.864144998003108,
0.906142061190345,0.949726796235432,0.99591887464429,0.99999995601045),
 .UNSPECIFIED.);
#308=B_SPLINE_CURVE_WITH_KNOTS('',3,(#57808,#57809,#57810,#57811,#57812,
#57813,#57814,#57815,#57816,#57817,#57818,#57819,#57820,#57821,#57822,#57823,
#57824,#57825,#57826,#57827,#57828,#57829,#57830,#57831,#57832,#57833,#57834,
#57835,#57836,#57837,#57838),.UNSPECIFIED.,.F.,.F.,(4,3,3,3,3,3,3,3,3,3,
4),(0.,0.12500000000001,0.187500000000016,0.218750000000019,0.23437500000002,
0.24218750000002,0.250000000000019,0.375000000000015,0.500000000000012,
0.750000000000006,1.),.UNSPECIFIED.);
#309=B_SPLINE_CURVE_WITH_KNOTS('',3,(#57840,#57841,#57842,#57843,#57844,
#57845,#57846,#57847,#57848,#57849,#57850,#57851,#57852,#57853,#57854,#57855,
#57856,#57857,#57858,#57859,#57860,#57861),.UNSPECIFIED.,.F.,.F.,(4,3,3,
3,3,3,3,4),(0.,0.177097147826628,0.275749264676803,0.455644332730437,0.5,
0.682209113428456,0.858274289412511,0.999997472817192),.UNSPECIFIED.);
#310=B_SPLINE_CURVE_WITH_KNOTS('',3,(#57864,#57865,#57866,#57867,#57868,
#57869,#57870,#57871,#57872,#57873,#57874,#57875,#57876,#57877,#57878,#57879,
#57880,#57881,#57882,#57883,#57884,#57885,#57886,#57887,#57888,#57889,#57890,
#57891,#57892,#57893,#57894,#57895,#57896,#57897,#57898,#57899,#57900,#57901,
#57902,#57903,#57904,#57905,#57906,#57907,#57908,#57909,#57910,#57911,#57912,
#57913,#57914,#57915,#57916,#57917,#57918,#57919,#57920,#57921,#57922,#57923,
#57924),.UNSPECIFIED.,.F.,.F.,(4,3,3,3,3,3,3,3,3,3,3,3,3,3,3,3,3,3,3,3,
4),(4.66155616960519E-11,0.0921586796163419,0.199885250793164,0.250000000000005,
0.280572529806289,0.383374079103984,0.437500000000011,0.462355616577624,
0.468750000000013,0.484375000000013,0.492187500000013,0.497992587906964,
0.500000000000012,0.580654371451503,0.656974867867654,0.686606159361902,
0.750000000000006,0.819755880055471,0.86988546566209,0.934942732831045,
1.),.UNSPECIFIED.);
#311=B_SPLINE_CURVE_WITH_KNOTS('',3,(#57969,#57970,#57971,#57972,#57973,
#57974,#57975,#57976,#57977,#57978,#57979,#57980,#57981,#57982,#57983,#57984,
#57985,#57986,#57987,#57988,#57989,#57990,#57991,#57992,#57993,#57994,#57995,
#57996,#57997,#57998,#57999,#58000,#58001,#58002,#58003,#58004,#58005,#58006,
#58007,#58008,#58009,#58010,#58011,#58012,#58013,#58014,#58015,#58016,#58017,
#58018,#58019,#58020,#58021,#58022,#58023,#58024,#58025,#58026,#58027,#58028,
#58029,#58030,#58031,#58032,#58033,#58034,#58035,#58036,#58037,#58038),
 .UNSPECIFIED.,.F.,.F.,(4,3,3,3,3,3,3,3,3,3,3,3,3,3,3,3,3,3,3,3,3,3,3,4),
(0.,0.0436825095638117,0.0764111191893734,0.120245151483468,0.125,0.179962620917879,
0.223835356219091,0.25,0.320059900246058,0.371520369880292,0.375,0.470560244901238,
0.5,0.519394870044145,0.625,0.667284556549449,0.741667232712626,0.75,0.808039637089994,
0.814941565966665,0.875,0.919746518961679,0.962447676468616,0.999999720259698),
 .UNSPECIFIED.);
#312=B_SPLINE_CURVE_WITH_KNOTS('',3,(#58039,#58040,#58041,#58042,#58043,
#58044,#58045,#58046,#58047,#58048,#58049,#58050,#58051,#58052,#58053,#58054,
#58055,#58056,#58057,#58058,#58059,#58060,#58061,#58062,#58063,#58064,#58065,
#58066,#58067,#58068,#58069,#58070,#58071,#58072,#58073,#58074,#58075,#58076,
#58077,#58078,#58079,#58080,#58081,#58082,#58083,#58084,#58085,#58086,#58087,
#58088,#58089,#58090,#58091,#58092,#58093,#58094,#58095,#58096,#58097,#58098,
#58099,#58100,#58101,#58102,#58103,#58104,#58105,#58106,#58107,#58108),
 .UNSPECIFIED.,.F.,.F.,(4,3,3,3,3,3,3,3,3,3,3,3,3,3,3,3,3,3,3,3,3,3,3,4),
(0.,0.0642447928422595,0.129222307761572,0.139648855540338,0.203363599061252,
0.250000000000004,0.300656405338484,0.369078202669245,0.437500000000007,
0.468750000000007,0.469712015730873,0.484375000000006,0.495155221973674,
0.500000000000006,0.563334839048207,0.625631000054916,0.644015069360023,
0.704247356561986,0.750000000000003,0.80787939926093,0.868482237357585,
0.928163376395018,0.961961767983911,0.999999992445097),.UNSPECIFIED.);
#313=B_SPLINE_CURVE_WITH_KNOTS('',3,(#58144,#58145,#58146,#58147,#58148,
#58149,#58150,#58151,#58152,#58153,#58154,#58155,#58156,#58157,#58158,#58159,
#58160,#58161,#58162,#58163,#58164,#58165,#58166,#58167,#58168,#58169,#58170,
#58171,#58172,#58173,#58174,#58175,#58176,#58177,#58178,#58179,#58180,#58181,
#58182,#58183,#58184,#58185,#58186,#58187,#58188,#58189,#58190,#58191,#58192,
#58193,#58194,#58195,#58196,#58197,#58198,#58199,#58200,#58201),
 .UNSPECIFIED.,.F.,.F.,(4,3,3,3,3,3,3,3,3,3,3,3,3,3,3,3,3,3,3,4),(6.48487790812236E-12,
0.0708156629893494,0.137202248264932,0.198838711004642,0.25,0.306727758080084,
0.362644355852727,0.418198532410901,0.473365958253842,0.5,0.500000490542878,
0.555648115907319,0.611778291583337,0.668285949116982,0.725508796212218,
0.75,0.8125,0.877120927925331,0.947966479212715,1.),.UNSPECIFIED.);
#314=B_SPLINE_CURVE_WITH_KNOTS('',3,(#58238,#58239,#58240,#58241,#58242,
#58243,#58244,#58245,#58246,#58247,#58248,#58249,#58250,#58251,#58252,#58253,
#58254,#58255,#58256,#58257,#58258,#58259,#58260,#58261,#58262,#58263,#58264,
#58265,#58266,#58267,#58268,#58269,#58270,#58271,#58272,#58273,#58274,#58275,
#58276,#58277,#58278,#58279,#58280,#58281,#58282,#58283,#58284,#58285,#58286,
#58287,#58288,#58289,#58290,#58291,#58292,#58293,#58294,#58295,#58296,#58297,
#58298,#58299,#58300,#58301,#58302,#58303,#58304,#58305,#58306,#58307,#58308,
#58309,#58310,#58311,#58312,#58313),.UNSPECIFIED.,.F.,.F.,(4,3,3,3,3,3,
3,3,3,3,3,3,3,3,3,3,3,3,3,3,3,3,3,3,3,4),(0.,0.081446458091042,0.125,0.125095970230205,
0.1875,0.21875,0.234375,0.244468168526415,0.25,0.312288980304435,0.384238156676023,
0.456663011015709,0.5,0.500013819131351,0.570973042205914,0.625,0.6875,
0.687743582276575,0.71875,0.734375,0.74450304915607,0.75,0.825461747691051,
0.874925048178083,0.950952013946258,1.),.UNSPECIFIED.);
#315=B_SPLINE_CURVE_WITH_KNOTS('',3,(#58360,#58361,#58362,#58363,#58364,
#58365,#58366,#58367,#58368,#58369,#58370,#58371,#58372,#58373,#58374,#58375,
#58376,#58377,#58378,#58379,#58380,#58381,#58382,#58383,#58384,#58385,#58386,
#58387,#58388,#58389,#58390,#58391,#58392,#58393,#58394,#58395,#58396,#58397,
#58398,#58399,#58400,#58401,#58402,#58403,#58404,#58405,#58406,#58407,#58408,
#58409,#58410,#58411,#58412,#58413,#58414,#58415,#58416,#58417,#58418,#58419,
#58420,#58421,#58422,#58423,#58424,#58425,#58426,#58427,#58428,#58429,#58430,
#58431,#58432),.UNSPECIFIED.,.F.,.F.,(4,3,3,3,3,3,3,3,3,3,3,3,3,3,3,3,3,
3,3,3,3,3,3,3,4),(1.45289839851345E-9,0.0431123229967307,0.0863131612725165,
0.129361940334382,0.1428571428571,0.153622117526577,0.204599112173322,0.255683858334241,
0.2857142857143,0.306349830038087,0.370801333218286,0.4285714285714,0.45934656340666,
0.52650199371959,0.5714285714286,0.612403301821111,0.676566210914991,0.7142857142857,
0.765276968910288,0.818291465317779,0.8571428571429,0.900814068173372,0.918051237057175,
0.961570018597272,1.),.UNSPECIFIED.);
#316=B_SPLINE_CURVE_WITH_KNOTS('',3,(#58436,#58437,#58438,#58439,#58440,
#58441,#58442,#58443,#58444,#58445,#58446,#58447,#58448,#58449,#58450,#58451,
#58452,#58453,#58454,#58455,#58456,#58457,#58458,#58459,#58460,#58461,#58462,
#58463,#58464,#58465,#58466,#58467,#58468,#58469,#58470,#58471,#58472,#58473,
#58474,#58475,#58476,#58477,#58478,#58479,#58480,#58481,#58482,#58483,#58484,
#58485,#58486,#58487,#58488,#58489,#58490,#58491,#58492,#58493,#58494,#58495,
#58496,#58497,#58498,#58499,#58500,#58501,#58502,#58503,#58504,#58505,#58506,
#58507,#58508),.UNSPECIFIED.,.F.,.F.,(4,3,3,3,3,3,3,3,3,3,3,3,3,3,3,3,3,
3,3,3,3,3,3,3,4),(0.,0.0558892464250319,0.112669224042606,0.15695313080606,
0.215051924639428,0.250000000000001,0.309316237904606,0.324310163867534,
0.385390337781192,0.437500000000002,0.468750000000002,0.484375000000003,
0.492187500000003,0.498949343333879,0.500000000000003,0.504582992891419,
0.573408026528877,0.641343139401869,0.680145623339031,0.750000000000002,
0.815926508015868,0.847891709112523,0.914669427968693,0.980716642894602,
1.),.UNSPECIFIED.);
#317=B_SPLINE_CURVE_WITH_KNOTS('',3,(#58509,#58510,#58511,#58512,#58513,
#58514,#58515,#58516,#58517,#58518,#58519,#58520,#58521,#58522,#58523,#58524,
#58525,#58526,#58527,#58528,#58529,#58530,#58531,#58532,#58533,#58534,#58535,
#58536,#58537,#58538,#58539,#58540,#58541,#58542,#58543,#58544,#58545,#58546,
#58547,#58548,#58549,#58550,#58551,#58552,#58553,#58554,#58555,#58556,#58557,
#58558,#58559,#58560,#58561,#58562,#58563,#58564,#58565,#58566),
 .UNSPECIFIED.,.F.,.F.,(4,3,3,3,3,3,3,3,3,3,3,3,3,3,3,3,3,3,3,4),(2.0837214114929E-13,
0.0546995064401617,0.111292609133422,0.169067321533811,0.228833933582854,
0.249999999999952,0.315860528667816,0.374999999999929,0.437499999999917,
0.468749999999912,0.48437499999991,0.49218749999991,0.498919423983201,0.49999999999991,
0.594327222529717,0.691604111918216,0.793562197925487,0.87730889011914,
0.981274245474638,1.),.UNSPECIFIED.);
#318=B_SPLINE_CURVE_WITH_KNOTS('',3,(#58604,#58605,#58606,#58607,#58608,
#58609,#58610,#58611,#58612,#58613,#58614,#58615,#58616,#58617,#58618,#58619,
#58620,#58621,#58622,#58623,#58624,#58625,#58626,#58627,#58628,#58629,#58630,
#58631,#58632,#58633,#58634,#58635,#58636,#58637,#58638,#58639,#58640,#58641,
#58642,#58643,#58644,#58645,#58646,#58647,#58648,#58649,#58650,#58651,#58652,
#58653,#58654,#58655,#58656,#58657,#58658,#58659,#58660,#58661),
 .UNSPECIFIED.,.F.,.F.,(4,3,3,3,3,3,3,3,3,3,3,3,3,3,3,3,3,3,3,4),(0.,0.0625,
0.123435565785335,0.183431668501261,0.242373265682533,0.25,0.30803982181753,
0.365336089158461,0.42229589810465,0.479062430264781,0.535777853356141,
0.59276962932548,0.649981899303138,0.707851544831901,0.75,0.808902168984071,
0.869151867693713,0.930294043556206,0.992902673504759,1.),.UNSPECIFIED.);
#319=B_SPLINE_CURVE_WITH_KNOTS('',3,(#58663,#58664,#58665,#58666,#58667,
#58668,#58669,#58670,#58671,#58672,#58673,#58674,#58675,#58676,#58677,#58678,
#58679,#58680,#58681,#58682,#58683,#58684,#58685,#58686,#58687),
 .UNSPECIFIED.,.F.,.F.,(4,3,3,3,3,3,3,3,4),(1.09119041741671E-6,0.173330994215996,
0.218339178824648,0.3333333333333,0.61546897963696,0.6666666666667,0.781166266027237,
0.949153050471761,1.),.UNSPECIFIED.);
#320=B_SPLINE_CURVE_WITH_KNOTS('',3,(#58688,#58689,#58690,#58691,#58692,
#58693,#58694,#58695,#58696,#58697,#58698,#58699,#58700),.UNSPECIFIED.,
 .F.,.F.,(4,3,3,3,4),(0.,0.1875,0.25,0.500000000000001,1.),
 .UNSPECIFIED.);
#321=B_SPLINE_CURVE_WITH_KNOTS('',3,(#58747,#58748,#58749,#58750,#58751,
#58752,#58753,#58754,#58755,#58756,#58757,#58758,#58759,#58760,#58761,#58762,
#58763,#58764,#58765,#58766,#58767,#58768,#58769,#58770,#58771,#58772,#58773,
#58774,#58775,#58776,#58777,#58778,#58779,#58780,#58781,#58782,#58783,#58784,
#58785,#58786,#58787,#58788,#58789,#58790,#58791,#58792,#58793,#58794,#58795,
#58796,#58797,#58798,#58799,#58800,#58801,#58802,#58803,#58804),
 .UNSPECIFIED.,.F.,.F.,(4,3,3,3,3,3,3,3,3,3,3,3,3,3,3,3,3,3,3,4),(0.,0.0625,
0.123429189990172,0.183419216265491,0.24235517342882,0.25,0.308040963404769,
0.365338364834653,0.422299317831246,0.479067015070969,0.53578363144022,
0.592776635003554,0.649990153248546,0.70786102805877,0.75,0.808903163413945,
0.869153777952148,0.930296804862004,0.992906138380765,1.),.UNSPECIFIED.);
#322=B_SPLINE_CURVE_WITH_KNOTS('',3,(#58805,#58806,#58807,#58808,#58809,
#58810,#58811,#58812,#58813,#58814,#58815,#58816,#58817,#58818,#58819,#58820,
#58821,#58822,#58823,#58824,#58825,#58826,#58827,#58828,#58829,#58830,#58831,
#58832,#58833,#58834,#58835,#58836,#58837,#58838,#58839,#58840,#58841,#58842,
#58843,#58844,#58845,#58846,#58847,#58848,#58849,#58850,#58851,#58852,#58853,
#58854,#58855,#58856,#58857,#58858,#58859,#58860,#58861,#58862,#58863,#58864,
#58865,#58866,#58867,#58868,#58869,#58870,#58871,#58872,#58873,#58874,#58875,
#58876,#58877,#58878,#58879,#58880,#58881,#58882,#58883,#58884,#58885,#58886,
#58887,#58888,#58889,#58890,#58891,#58892,#58893,#58894,#58895,#58896,#58897,
#58898),.UNSPECIFIED.,.F.,.F.,(4,3,3,3,3,3,3,3,3,3,3,3,3,3,3,3,3,3,3,3,
3,3,3,3,3,3,3,3,3,3,3,4),(0.,0.00359421609921195,0.0901499213363355,0.124999999999999,
0.163074003856875,0.187499999999999,0.218749999999998,0.234374999999998,
0.242187499999998,0.246093749999998,0.248046874999998,0.249999999999998,
0.315877948487601,0.331449187946985,0.3964014492295,0.461540192267028,0.499908689841259,
0.499999999999999,0.564252115945543,0.625,0.668380810462763,0.6875,0.71875,
0.734375000000001,0.742187500000001,0.746093750000001,0.748046875000001,
0.750000000000001,0.836745522375066,0.920992550643248,0.99624855591021,
1.),.UNSPECIFIED.);
#323=B_SPLINE_CURVE_WITH_KNOTS('',3,(#58899,#58900,#58901,#58902,#58903,
#58904,#58905,#58906,#58907,#58908,#58909,#58910,#58911,#58912,#58913,#58914,
#58915,#58916,#58917,#58918,#58919,#58920,#58921,#58922,#58923,#58924,#58925,
#58926,#58927,#58928,#58929,#58930,#58931,#58932,#58933,#58934,#58935,#58936,
#58937,#58938,#58939,#58940,#58941,#58942,#58943,#58944,#58945,#58946,#58947,
#58948,#58949,#58950,#58951,#58952,#58953,#58954,#58955,#58956),
 .UNSPECIFIED.,.F.,.F.,(4,3,3,3,3,3,3,3,3,3,3,3,3,3,3,3,3,3,3,4),(0.,0.0701503128262514,
0.136056545864733,0.197350793223507,0.25,0.307839026190954,0.364828669625009,
0.421434874490469,0.477635358311654,0.5,0.500034575059412,0.555642599320633,
0.611688567793988,0.668085517949893,0.725157605455238,0.75,0.8125,0.876726864335634,
0.946985567133671,1.),.UNSPECIFIED.);
#324=B_SPLINE_CURVE_WITH_KNOTS('',3,(#58993,#58994,#58995,#58996,#58997,
#58998,#58999,#59000,#59001,#59002,#59003,#59004,#59005,#59006,#59007,#59008,
#59009,#59010,#59011,#59012,#59013,#59014,#59015,#59016,#59017,#59018,#59019,
#59020,#59021,#59022,#59023,#59024,#59025,#59026,#59027,#59028,#59029,#59030,
#59031,#59032,#59033,#59034,#59035,#59036,#59037,#59038,#59039,#59040,#59041,
#59042,#59043,#59044,#59045,#59046,#59047,#59048,#59049,#59050,#59051,#59052,
#59053,#59054,#59055,#59056,#59057,#59058,#59059,#59060,#59061,#59062,#59063,
#59064,#59065,#59066,#59067,#59068,#59069,#59070,#59071,#59072,#59073,#59074,
#59075,#59076,#59077,#59078,#59079,#59080,#59081,#59082,#59083,#59084,#59085,
#59086,#59087,#59088,#59089,#59090,#59091,#59092,#59093,#59094,#59095,#59096,
#59097,#59098,#59099,#59100,#59101,#59102,#59103,#59104,#59105,#59106,#59107,
#59108,#59109,#59110,#59111,#59112,#59113,#59114,#59115,#59116),
 .UNSPECIFIED.,.F.,.F.,(4,3,3,3,3,3,3,3,3,3,3,3,3,3,3,3,3,3,3,3,3,3,3,3,
3,3,3,3,3,3,3,3,3,3,3,3,3,3,3,3,3,4),(2.34638652342419E-7,0.0312501759789898,
0.0620856368219447,0.0935428184109735,0.125000000000002,0.156250000000003,
0.187500000000003,0.218750000000004,0.234375000000004,0.242187500000004,
0.246093750000004,0.248046875000004,0.250000000000004,0.298059640401285,
0.343846953199899,0.375000000000004,0.41630338916026,0.437500000000004,
0.468750000000004,0.484375000000004,0.496666652157399,0.499736069550179,
0.500000000000004,0.542051437923008,0.584507507123047,0.625000000000003,
0.671672548344778,0.687500000000003,0.718750000000003,0.734375000000003,
0.742187500000003,0.746093750000003,0.748046875000003,0.750000000000003,
0.781250000000003,0.811342334720831,0.843171167360416,0.875000000000002,
0.906250000000001,0.937257522432499,0.968641912191417,1.),.UNSPECIFIED.);
#325=B_SPLINE_CURVE_WITH_KNOTS('',3,(#59117,#59118,#59119,#59120,#59121,
#59122,#59123,#59124,#59125,#59126,#59127,#59128,#59129,#59130,#59131,#59132,
#59133,#59134,#59135,#59136,#59137,#59138,#59139,#59140,#59141,#59142,#59143,
#59144,#59145,#59146,#59147,#59148,#59149,#59150,#59151,#59152,#59153,#59154,
#59155,#59156,#59157,#59158,#59159,#59160,#59161,#59162,#59163,#59164,#59165,
#59166,#59167,#59168,#59169,#59170,#59171,#59172,#59173,#59174,#59175,#59176,
#59177),.UNSPECIFIED.,.F.,.F.,(4,3,3,3,3,3,3,3,3,3,3,3,3,3,3,3,3,3,3,3,
4),(3.81433860989148E-8,0.0594692343242972,0.119461353578183,0.180335258041045,
0.228233351338028,0.25,0.3125,0.375,0.420629587711987,0.46648057363459,
0.5,0.532982690390264,0.595584385518065,0.657507313747222,0.718468618098683,
0.75,0.809830728585965,0.831293935547951,0.890887163314741,0.94959436212385,
1.),.UNSPECIFIED.);
#326=B_SPLINE_CURVE_WITH_KNOTS('',3,(#59245,#59246,#59247,#59248,#59249,
#59250,#59251,#59252,#59253,#59254,#59255,#59256,#59257,#59258,#59259,#59260,
#59261,#59262,#59263,#59264,#59265,#59266,#59267,#59268,#59269,#59270,#59271,
#59272,#59273,#59274,#59275,#59276,#59277,#59278,#59279,#59280,#59281,#59282,
#59283,#59284,#59285,#59286,#59287,#59288,#59289,#59290,#59291,#59292,#59293,
#59294,#59295,#59296,#59297,#59298,#59299,#59300,#59301,#59302,#59303,#59304,
#59305,#59306,#59307,#59308,#59309,#59310,#59311,#59312,#59313,#59314,#59315,
#59316,#59317,#59318,#59319,#59320,#59321,#59322,#59323,#59324,#59325,#59326,
#59327,#59328,#59329,#59330,#59331,#59332,#59333,#59334,#59335,#59336,#59337,
#59338,#59339,#59340,#59341,#59342,#59343,#59344,#59345,#59346,#59347,#59348,
#59349,#59350,#59351,#59352,#59353,#59354,#59355,#59356,#59357,#59358,#59359,
#59360,#59361,#59362,#59363,#59364,#59365,#59366,#59367,#59368,#59369,#59370,
#59371,#59372,#59373,#59374,#59375,#59376,#59377,#59378,#59379,#59380,#59381,
#59382,#59383,#59384,#59385,#59386,#59387,#59388,#59389,#59390,#59391,#59392,
#59393,#59394,#59395,#59396,#59397,#59398,#59399,#59400,#59401,#59402,#59403,
#59404,#59405,#59406,#59407,#59408,#59409,#59410),.UNSPECIFIED.,.F.,.F.,
(4,3,3,3,3,3,3,3,3,3,3,3,3,3,3,3,3,3,3,3,3,3,3,3,3,3,3,3,3,3,3,3,3,3,3,
3,3,3,3,3,3,3,3,3,3,3,3,3,3,3,3,3,3,3,3,4),(8.92126295307914E-8,0.0341935387179955,
0.0625000000000023,0.0800482297466476,0.0937500000000034,0.109375000000004,
0.117187500000004,0.121093750000004,0.123046875000004,0.125000000000004,
0.156938379731607,0.187500000000001,0.21875,0.234374999999999,0.237595027422283,
0.242187499999999,0.246093749999998,0.248046874999998,0.249999999999998,
0.290857013627676,0.312499999999998,0.328976223561752,0.343749999999998,
0.359374999999998,0.367187499999998,0.371093749999998,0.373046874999998,
0.374999999999998,0.425244790370268,0.437499999999998,0.468749999999998,
0.484374999999998,0.492187499999998,0.496093749999998,0.499999999999998,
0.520144459031146,0.572559628884996,0.616875406841374,0.624999999999999,
0.65137052874562,0.678310089621322,0.687499999999999,0.709129374678632,
0.749999999999999,0.781249999999999,0.789062499999999,0.796875,0.799044011249208,
0.8125,0.858407509871286,0.875,0.885476739305792,0.932673117967918,0.980788676053958,
0.985729040830903,1.),.UNSPECIFIED.);
#327=B_SPLINE_CURVE_WITH_KNOTS('',3,(#59464,#59465,#59466,#59467,#59468,
#59469,#59470,#59471,#59472,#59473,#59474,#59475,#59476,#59477,#59478,#59479,
#59480,#59481,#59482,#59483,#59484,#59485,#59486,#59487,#59488,#59489,#59490,
#59491,#59492,#59493,#59494,#59495,#59496,#59497,#59498,#59499,#59500,#59501,
#59502,#59503,#59504,#59505,#59506,#59507,#59508,#59509,#59510,#59511,#59512,
#59513,#59514,#59515,#59516,#59517,#59518,#59519,#59520,#59521,#59522,#59523,
#59524,#59525,#59526,#59527,#59528,#59529,#59530,#59531,#59532,#59533,#59534,
#59535,#59536,#59537,#59538,#59539,#59540,#59541,#59542,#59543,#59544,#59545,
#59546,#59547,#59548,#59549,#59550,#59551,#59552,#59553,#59554,#59555,#59556,
#59557,#59558,#59559,#59560,#59561,#59562,#59563,#59564,#59565,#59566,#59567,
#59568,#59569,#59570,#59571,#59572,#59573,#59574,#59575,#59576,#59577,#59578,
#59579,#59580,#59581,#59582,#59583,#59584,#59585,#59586,#59587,#59588,#59589,
#59590,#59591,#59592,#59593,#59594,#59595,#59596,#59597,#59598,#59599,#59600,
#59601,#59602,#59603,#59604,#59605,#59606,#59607,#59608,#59609,#59610,#59611,
#59612,#59613,#59614,#59615,#59616,#59617,#59618,#59619,#59620,#59621,#59622,
#59623,#59624,#59625,#59626,#59627,#59628,#59629,#59630,#59631,#59632,#59633,
#59634,#59635,#59636,#59637,#59638,#59639,#59640,#59641,#59642,#59643,#59644,
#59645,#59646,#59647,#59648,#59649,#59650,#59651,#59652,#59653,#59654,#59655,
#59656,#59657,#59658,#59659,#59660,#59661,#59662,#59663,#59664,#59665,#59666,
#59667,#59668,#59669,#59670,#59671,#59672,#59673,#59674,#59675,#59676,#59677),
 .UNSPECIFIED.,.F.,.F.,(4,3,3,3,3,3,3,3,3,3,3,3,3,3,3,3,3,3,3,3,3,3,3,3,
3,3,3,3,3,3,3,3,3,3,3,3,3,3,3,3,3,3,3,3,3,3,3,3,3,3,3,3,3,3,3,3,3,3,3,3,
3,3,3,3,3,3,3,3,3,3,3,4),(1.24252210392226E-7,0.0158962995490016,0.0300344810503092,
0.0432269198228004,0.0555827596438185,0.0625000000000163,0.0703125000000184,
0.0712890625000187,0.0722656250000189,0.0742187500000193,0.0781250000000199,
0.0927960918760498,0.093750000000022,0.10750217113599,0.109375000000024,
0.117187500000025,0.121093750000026,0.123046875000026,0.124023437500026,
0.125000000000026,0.145668040803103,0.156250000000028,0.171875000000029,
0.17968750000003,0.186599973254188,0.18750000000003,0.218750000000033,0.234375000000035,
0.242187500000036,0.249023437500036,0.250000000000036,0.273948923410479,
0.297787299536743,0.312500000000037,0.336691512690665,0.343750000000037,
0.359375000000037,0.367187500000037,0.371093750000037,0.373046875000037,
0.374023437500037,0.375000000000037,0.402438386449995,0.437500000000038,
0.468750000000039,0.484375000000039,0.492187500000039,0.496093750000039,
0.498046875000039,0.499023437500039,0.499511718750039,0.500000000000039,
0.531454858450231,0.563785493779374,0.598875571442389,0.625000000000031,
0.661168477061904,0.687500000000027,0.712237630428612,0.718750000000025,
0.734375000000024,0.742187500000023,0.746093750000023,0.748046875000023,
0.749023437500023,0.750000000000023,0.79575267113575,0.84060489234686,0.884625373990666,
0.928360534765868,0.971893735048001,1.),.UNSPECIFIED.);
#328=B_SPLINE_CURVE_WITH_KNOTS('',3,(#59762,#59763,#59764,#59765,#59766,
#59767,#59768,#59769,#59770,#59771,#59772,#59773,#59774,#59775,#59776,#59777,
#59778,#59779,#59780,#59781,#59782,#59783,#59784,#59785,#59786,#59787,#59788,
#59789,#59790,#59791,#59792,#59793,#59794,#59795,#59796,#59797,#59798,#59799,
#59800,#59801,#59802,#59803,#59804,#59805,#59806,#59807,#59808,#59809,#59810,
#59811,#59812,#59813,#59814,#59815,#59816,#59817,#59818,#59819,#59820,#59821,
#59822,#59823,#59824,#59825,#59826,#59827,#59828,#59829,#59830,#59831,#59832,
#59833,#59834,#59835,#59836,#59837,#59838,#59839,#59840,#59841,#59842,#59843,
#59844,#59845,#59846,#59847,#59848,#59849,#59850,#59851,#59852,#59853,#59854,
#59855,#59856,#59857,#59858,#59859,#59860,#59861,#59862,#59863,#59864,#59865,
#59866,#59867,#59868,#59869,#59870,#59871,#59872,#59873,#59874,#59875,#59876,
#59877,#59878,#59879,#59880,#59881,#59882,#59883,#59884,#59885,#59886,#59887,
#59888,#59889,#59890,#59891,#59892,#59893,#59894,#59895,#59896,#59897,#59898,
#59899,#59900,#59901,#59902,#59903,#59904,#59905,#59906,#59907,#59908,#59909,
#59910,#59911,#59912,#59913,#59914,#59915,#59916,#59917,#59918),
 .UNSPECIFIED.,.F.,.F.,(4,3,3,3,3,3,3,3,3,3,3,3,3,3,3,3,3,3,3,3,3,3,3,3,
3,3,3,3,3,3,3,3,3,3,3,3,3,3,3,3,3,3,3,3,3,3,3,3,3,3,3,3,4),(1.72726524224126E-7,
0.0434573043788212,0.0863338267586707,0.0932171693142727,0.124999999999993,
0.165840000814769,0.177273799940387,0.187499999999989,0.218749999999987,
0.234374999999986,0.242187499999986,0.246093749999986,0.249511718749986,
0.249999999999986,0.260114116099238,0.284905555310815,0.309602658376984,
0.312499999999988,0.33693232554173,0.343749999999989,0.35937499999999,0.359741581816558,
0.36718749999999,0.37109374999999,0.373046874999991,0.374023437499991,0.374999999999991,
0.4271620062675,0.437499999999993,0.446538820825428,0.468749999999994,0.484374999999994,
0.492187499999994,0.499058232171587,0.499999999999994,0.529371777930485,
0.59548810882445,0.601623732066306,0.624999999999998,0.666785566987401,
0.6875,0.718750000000001,0.726753344238875,0.734375000000002,0.746093750000002,
0.750000000000002,0.777563968254758,0.821929376370596,0.864143232885838,
0.906140596325827,0.949725635816364,0.995918047404073,0.999999956001043),
 .UNSPECIFIED.);
#329=B_SPLINE_CURVE_WITH_KNOTS('',3,(#59960,#59961,#59962,#59963,#59964,
#59965,#59966,#59967,#59968,#59969,#59970,#59971,#59972,#59973,#59974,#59975,
#59976,#59977,#59978,#59979,#59980,#59981,#59982,#59983,#59984,#59985,#59986,
#59987,#59988,#59989,#59990),.UNSPECIFIED.,.F.,.F.,(4,3,3,3,3,3,3,3,3,3,
4),(0.,0.125000000000012,0.187500000000019,0.21875000000002,0.234375000000022,
0.242187500000021,0.25000000000002,0.375000000000017,0.500000000000013,
0.750000000000007,1.),.UNSPECIFIED.);
#330=B_SPLINE_CURVE_WITH_KNOTS('',3,(#59992,#59993,#59994,#59995,#59996,
#59997,#59998,#59999,#60000,#60001,#60002,#60003,#60004,#60005,#60006,#60007,
#60008,#60009,#60010,#60011,#60012,#60013),.UNSPECIFIED.,.F.,.F.,(4,3,3,
3,3,3,3,4),(6.12536510437413E-13,0.177079554736073,0.285234641299018,0.46505528483709,
0.5,0.685616239441862,0.871232478883723,0.999997383318307),
 .UNSPECIFIED.);
#331=B_SPLINE_CURVE_WITH_KNOTS('',3,(#60016,#60017,#60018,#60019,#60020,
#60021,#60022,#60023,#60024,#60025,#60026,#60027,#60028,#60029,#60030,#60031,
#60032,#60033,#60034,#60035,#60036,#60037,#60038,#60039,#60040,#60041,#60042,
#60043,#60044,#60045,#60046,#60047,#60048,#60049,#60050,#60051,#60052,#60053,
#60054,#60055,#60056,#60057,#60058,#60059,#60060,#60061,#60062,#60063,#60064,
#60065,#60066,#60067,#60068,#60069,#60070,#60071,#60072,#60073,#60074,#60075,
#60076),.UNSPECIFIED.,.F.,.F.,(4,3,3,3,3,3,3,3,3,3,3,3,3,3,3,3,3,3,3,3,
4),(3.08984601557555E-11,0.101977911095453,0.216247452367153,0.250000000000008,
0.304568311352161,0.375000000000011,0.437500000000014,0.468750000000016,
0.484375000000017,0.49416989406617,0.500000000000017,0.502028002520118,
0.58458238428531,0.662800125303651,0.723699269222825,0.750000000000009,
0.823969575829282,0.894343004279093,0.916583809267426,0.983994210266332,
0.999999999983593),.UNSPECIFIED.);
#332=B_SPLINE_CURVE_WITH_KNOTS('',3,(#60121,#60122,#60123,#60124,#60125,
#60126,#60127,#60128,#60129,#60130,#60131,#60132,#60133,#60134,#60135,#60136,
#60137,#60138,#60139,#60140,#60141,#60142,#60143,#60144,#60145,#60146,#60147,
#60148,#60149,#60150,#60151,#60152,#60153,#60154,#60155,#60156,#60157,#60158,
#60159,#60160,#60161,#60162,#60163,#60164,#60165,#60166,#60167,#60168,#60169,
#60170,#60171,#60172,#60173,#60174,#60175,#60176,#60177,#60178,#60179,#60180,
#60181,#60182,#60183,#60184,#60185,#60186,#60187,#60188,#60189,#60190),
 .UNSPECIFIED.,.F.,.F.,(4,3,3,3,3,3,3,3,3,3,3,3,3,3,3,3,3,3,3,3,3,3,3,4),
(0.,0.043555149686333,0.0764703251628506,0.120151057814094,0.125,0.178532566021585,
0.223906425134656,0.25,0.318743687382601,0.371576027078518,0.375,0.469091463337279,
0.5,0.519437204606587,0.625,0.667313790479252,0.741710622422343,0.75,0.808035613360659,
0.814958103135643,0.875,0.919742715260402,0.962451522902248,0.999999720292486),
 .UNSPECIFIED.);
#333=B_SPLINE_CURVE_WITH_KNOTS('',3,(#60191,#60192,#60193,#60194,#60195,
#60196,#60197,#60198,#60199,#60200,#60201,#60202,#60203,#60204,#60205,#60206,
#60207,#60208,#60209,#60210,#60211,#60212,#60213,#60214,#60215,#60216,#60217,
#60218,#60219,#60220,#60221,#60222,#60223,#60224,#60225,#60226,#60227,#60228,
#60229,#60230,#60231,#60232,#60233,#60234,#60235,#60236,#60237,#60238,#60239,
#60240,#60241,#60242,#60243,#60244,#60245,#60246,#60247,#60248,#60249,#60250,
#60251,#60252,#60253,#60254,#60255,#60256,#60257,#60258,#60259,#60260),
 .UNSPECIFIED.,.F.,.F.,(4,3,3,3,3,3,3,3,3,3,3,3,3,3,3,3,3,3,3,3,3,3,3,4),
(0.,0.0642450128226209,0.129222728498677,0.139648736860595,0.203363671729352,
0.250000000000001,0.300656432205033,0.369078216102518,0.437500000000002,
0.468750000000002,0.46971171597224,0.484375000000001,0.495154978438866,
0.500000000000001,0.563334744373279,0.625630806355903,0.644014764731035,
0.704246943422557,0.750000000000001,0.807879654393242,0.868482353955307,
0.928163350063891,0.961962300095513,0.999999992441419),.UNSPECIFIED.);
#334=B_SPLINE_CURVE_WITH_KNOTS('',3,(#60297,#60298,#60299,#60300,#60301,
#60302,#60303,#60304,#60305,#60306,#60307,#60308,#60309,#60310,#60311,#60312,
#60313,#60314,#60315,#60316,#60317,#60318,#60319,#60320,#60321,#60322,#60323,
#60324,#60325,#60326,#60327,#60328,#60329,#60330,#60331,#60332,#60333,#60334,
#60335,#60336,#60337,#60338,#60339,#60340,#60341,#60342,#60343,#60344,#60345,
#60346,#60347,#60348,#60349,#60350,#60351,#60352,#60353,#60354),
 .UNSPECIFIED.,.F.,.F.,(4,3,3,3,3,3,3,3,3,3,3,3,3,3,3,3,3,3,3,4),(6.60011716677258E-12,
0.0585629947700057,0.117996459937316,0.168707856042748,0.228541438031087,
0.25,0.3125,0.375000000000001,0.421054220391796,0.467108440783592,0.500000000000001,
0.563532899306448,0.626399529031098,0.688223245939294,0.75,0.771768815670398,
0.83260584940954,0.892881408073043,0.952306960013565,0.999999961863675),
 .UNSPECIFIED.);
#335=B_SPLINE_CURVE_WITH_KNOTS('',3,(#60355,#60356,#60357,#60358,#60359,
#60360,#60361,#60362,#60363,#60364,#60365,#60366,#60367,#60368,#60369,#60370,
#60371,#60372,#60373,#60374,#60375,#60376,#60377,#60378,#60379,#60380,#60381,
#60382,#60383,#60384,#60385,#60386,#60387,#60388,#60389,#60390,#60391,#60392,
#60393,#60394,#60395,#60396,#60397,#60398,#60399,#60400,#60401,#60402,#60403,
#60404,#60405,#60406,#60407,#60408,#60409,#60410,#60411,#60412),
 .UNSPECIFIED.,.F.,.F.,(4,3,3,3,3,3,3,3,3,3,3,3,3,3,3,3,3,3,3,4),(0.,0.0823874715591667,
0.156266197944322,0.223011563441643,0.25,0.307989093614892,0.364543396570697,
0.420407336747116,0.475427758760885,0.5,0.500020658777188,0.554932458503316,
0.610826173270344,0.667398897766358,0.725169989432572,0.75,0.817894591813742,
0.890404386237424,0.974097661819355,1.),.UNSPECIFIED.);
#336=B_SPLINE_CURVE_WITH_KNOTS('',3,(#60450,#60451,#60452,#60453,#60454,
#60455,#60456,#60457,#60458,#60459,#60460,#60461,#60462,#60463,#60464,#60465,
#60466,#60467,#60468,#60469,#60470,#60471,#60472,#60473,#60474,#60475,#60476,
#60477,#60478,#60479,#60480,#60481,#60482,#60483,#60484,#60485,#60486,#60487,
#60488,#60489,#60490,#60491,#60492,#60493,#60494,#60495,#60496,#60497,#60498,
#60499,#60500,#60501,#60502,#60503,#60504,#60505,#60506,#60507,#60508,#60509,
#60510,#60511,#60512,#60513,#60514,#60515,#60516,#60517,#60518,#60519,#60520,
#60521,#60522,#60523,#60524,#60525,#60526,#60527,#60528,#60529,#60530,#60531),
 .UNSPECIFIED.,.F.,.F.,(4,3,3,3,3,3,3,3,3,3,3,3,3,3,3,3,3,3,3,3,3,3,3,3,
3,3,3,4),(0.,0.075415314847338,0.125000000000002,0.138683869187328,0.187500000000003,
0.218750000000003,0.234375000000004,0.242187500000004,0.246093750000004,
0.250000000000004,0.321477738395407,0.389912144118573,0.457885661220333,
0.500000000000004,0.500062330010128,0.566092728183435,0.625000000000004,
0.678656853856775,0.687500000000004,0.718750000000004,0.734375000000004,
0.742187500000004,0.746093750000004,0.750000000000004,0.822132808280447,
0.861437880157647,0.936459487512057,0.999999999999982),.UNSPECIFIED.);
#337=B_SPLINE_CURVE_WITH_KNOTS('',3,(#60570,#60571,#60572,#60573,#60574,
#60575,#60576,#60577,#60578,#60579,#60580,#60581,#60582,#60583,#60584,#60585,
#60586,#60587,#60588,#60589,#60590,#60591),.UNSPECIFIED.,.F.,.F.,(4,3,3,
3,3,3,3,4),(4.23912252164219E-6,0.121979217178925,0.310989608589463,0.5,
0.679777216446932,0.707646284458543,0.884704706825873,0.99999999999933),
 .UNSPECIFIED.);
#338=B_SPLINE_CURVE_WITH_KNOTS('',3,(#60593,#60594,#60595,#60596,#60597,
#60598,#60599,#60600,#60601,#60602,#60603,#60604),.UNSPECIFIED.,.F.,.F.,
(4,2,2,2,2,4),(-0.133419885800988,-0.128305363731286,-0.107742733446663,
-0.0932105788792922,-0.0630589864485123,-1.03237217784953E-6),
 .UNSPECIFIED.);
#339=B_SPLINE_CURVE_WITH_KNOTS('',3,(#60605,#60606,#60607,#60608,#60609,
#60610,#60611,#60612,#60613,#60614,#60615,#60616,#60617,#60618,#60619,#60620,
#60621,#60622,#60623,#60624,#60625,#60626,#60627,#60628,#60629,#60630,#60631,
#60632,#60633,#60634,#60635,#60636,#60637,#60638,#60639,#60640,#60641,#60642,
#60643,#60644,#60645,#60646,#60647,#60648,#60649,#60650,#60651,#60652,#60653,
#60654,#60655,#60656,#60657,#60658,#60659,#60660,#60661,#60662),
 .UNSPECIFIED.,.F.,.F.,(4,3,3,3,3,3,3,3,3,3,3,3,3,3,3,3,3,3,3,4),(2.61381413586043E-6,
0.0670473710053725,0.0814149118918829,0.151202322002298,0.224512436629058,
0.24999999999998,0.273781868251335,0.350340974656353,0.430500053925807,
0.437499999999966,0.468749999999964,0.484374999999964,0.494602270260102,
0.495837805863796,0.499999999999964,0.607491325586912,0.693045153608403,
0.80555739922953,0.895474625281069,1.),.UNSPECIFIED.);
#340=B_SPLINE_CURVE_WITH_KNOTS('',3,(#60704,#60705,#60706,#60707,#60708,
#60709,#60710,#60711,#60712,#60713,#60714,#60715,#60716,#60717,#60718,#60719,
#60720,#60721,#60722,#60723,#60724,#60725,#60726,#60727,#60728,#60729,#60730,
#60731,#60732,#60733,#60734,#60735,#60736,#60737,#60738,#60739,#60740,#60741,
#60742,#60743,#60744,#60745,#60746,#60747,#60748,#60749,#60750,#60751,#60752,
#60753,#60754,#60755,#60756,#60757,#60758,#60759,#60760,#60761,#60762,#60763,
#60764,#60765,#60766,#60767,#60768,#60769,#60770,#60771,#60772,#60773,#60774,
#60775,#60776,#60777,#60778,#60779,#60780,#60781,#60782,#60783,#60784,#60785,
#60786,#60787,#60788,#60789,#60790,#60791),.UNSPECIFIED.,.F.,.F.,(4,3,3,
3,3,3,3,3,3,3,3,3,3,3,3,3,3,3,3,3,3,3,3,3,3,3,3,3,3,4),(3.50091154771304E-7,
0.0527824144532673,0.0818205493840706,0.138472328687778,0.195944420947396,
0.235749554746624,0.293011713332015,0.351192964442254,0.399875422218759,
0.437499999999992,0.468749999999991,0.484374999999991,0.49218749999999,
0.496093749999991,0.499508598803165,0.499999999999991,0.565860965729536,
0.629575211034318,0.693959315536848,0.725751294512647,0.781249999999995,
0.790730946026802,0.796874999999996,0.812499999999996,0.869044143359368,
0.874999999999997,0.884835921693697,0.938701676345939,0.993362228153319,
0.999999777713792),.UNSPECIFIED.);
#341=B_SPLINE_CURVE_WITH_KNOTS('',3,(#60865,#60866,#60867,#60868,#60869,
#60870,#60871,#60872,#60873,#60874,#60875,#60876,#60877,#60878,#60879,#60880,
#60881,#60882,#60883,#60884,#60885,#60886,#60887,#60888,#60889,#60890,#60891,
#60892,#60893,#60894,#60895,#60896,#60897,#60898,#60899,#60900,#60901,#60902,
#60903,#60904,#60905,#60906,#60907,#60908,#60909,#60910,#60911,#60912,#60913,
#60914,#60915,#60916,#60917,#60918,#60919,#60920,#60921,#60922,#60923,#60924,
#60925,#60926,#60927,#60928,#60929,#60930,#60931,#60932,#60933,#60934,#60935,
#60936,#60937,#60938,#60939,#60940,#60941,#60942,#60943,#60944,#60945,#60946,
#60947,#60948,#60949,#60950,#60951,#60952,#60953,#60954,#60955),
 .UNSPECIFIED.,.F.,.F.,(4,3,3,3,3,3,3,3,3,3,3,3,3,3,3,3,3,3,3,3,3,3,3,3,
3,3,3,3,3,3,4),(1.9887216213797E-7,0.0470902988611094,0.0950885656755635,
0.109526529164859,0.124999999999995,0.176685441702215,0.187499999999992,
0.195574874079998,0.203124999999992,0.218749999999991,0.249999999999991,
0.27062136400391,0.334103646587719,0.398264704624234,0.430414449322694,
0.437499999999987,0.468749999999987,0.484374999999987,0.492187499999987,
0.498034136225503,0.499999999999987,0.559924712613938,0.600124996010047,
0.658475318160386,0.715889407223646,0.764251057126962,0.821850440010763,
0.878616575074156,0.918179752465716,0.970963259453568,1.),.UNSPECIFIED.);
#342=B_SPLINE_CURVE_WITH_KNOTS('',3,(#60956,#60957,#60958,#60959,#60960,
#60961,#60962,#60963,#60964,#60965,#60966,#60967,#60968,#60969,#60970,#60971,
#60972,#60973,#60974,#60975,#60976,#60977,#60978,#60979,#60980,#60981,#60982,
#60983,#60984,#60985,#60986,#60987,#60988,#60989,#60990,#60991,#60992,#60993,
#60994,#60995,#60996,#60997,#60998,#60999,#61000,#61001,#61002,#61003,#61004,
#61005,#61006,#61007,#61008,#61009,#61010,#61011,#61012,#61013,#61014,#61015,
#61016,#61017,#61018,#61019),.UNSPECIFIED.,.F.,.F.,(4,3,3,3,3,3,3,3,3,3,
3,3,3,3,3,3,3,3,3,3,3,4),(0.,0.0259412938399118,0.127853460989982,0.228784505870627,
0.250000000000025,0.349135504880914,0.375000000000038,0.437500000000044,
0.468750000000048,0.48437500000005,0.492187500000051,0.498686700960381,
0.500000000000052,0.570456477027826,0.639131807094066,0.705384248701921,
0.750000000000026,0.812499999984393,0.870266491265459,0.926774908096166,
0.981742412633779,0.999999999937496),.UNSPECIFIED.);
#343=B_SPLINE_CURVE_WITH_KNOTS('',3,(#61057,#61058,#61059,#61060,#61061,
#61062,#61063,#61064,#61065,#61066,#61067,#61068,#61069,#61070,#61071,#61072,
#61073,#61074,#61075,#61076,#61077,#61078,#61079,#61080,#61081,#61082,#61083,
#61084,#61085,#61086,#61087),.UNSPECIFIED.,.F.,.F.,(4,3,3,3,3,3,3,3,3,3,
4),(0.,0.124999999999989,0.187499999999983,0.21874999999998,0.234374999999979,
0.242187499999979,0.249999999999979,0.374999999999983,0.499999999999987,
0.749999999999993,1.),.UNSPECIFIED.);
#344=B_SPLINE_CURVE_WITH_KNOTS('',3,(#61088,#61089,#61090,#61091,#61092,
#61093,#61094,#61095,#61096,#61097,#61098,#61099,#61100,#61101,#61102,#61103,
#61104,#61105,#61106,#61107,#61108,#61109,#61110,#61111,#61112),
 .UNSPECIFIED.,.F.,.F.,(4,3,3,3,3,3,3,3,4),(0.,0.167965175142067,0.230725444345264,
0.3333333333333,0.614592509477533,0.6666666666667,0.794930443258819,0.968172652596159,
0.999998645723269),.UNSPECIFIED.);
#345=B_SPLINE_CURVE_WITH_KNOTS('',3,(#61157,#61158,#61159,#61160,#61161,
#61162,#61163,#61164,#61165,#61166,#61167,#61168,#61169,#61170,#61171,#61172),
 .UNSPECIFIED.,.F.,.F.,(4,3,3,3,3,4),(0.,0.298197738937631,0.3333333333333,
0.6666666666667,0.972390787491876,0.999897516477361),.UNSPECIFIED.);
#346=B_SPLINE_CURVE_WITH_KNOTS('',3,(#61174,#61175,#61176,#61177,#61178,
#61179,#61180,#61181,#61182,#61183,#61184),.UNSPECIFIED.,.F.,.F.,(4,1,2,
2,2,4),(0.,0.124999999999994,0.218749999999991,0.24999999999999,0.499999999999994,
1.),.UNSPECIFIED.);
#347=B_SPLINE_CURVE_WITH_KNOTS('',3,(#61185,#61186,#61187,#61188,#61189,
#61190,#61191,#61192,#61193,#61194,#61195,#61196,#61197,#61198,#61199,#61200,
#61201,#61202,#61203,#61204,#61205,#61206,#61207,#61208,#61209,#61210,#61211,
#61212,#61213,#61214,#61215,#61216,#61217,#61218,#61219,#61220,#61221,#61222,
#61223,#61224,#61225,#61226,#61227,#61228,#61229,#61230,#61231,#61232,#61233,
#61234,#61235,#61236,#61237,#61238,#61239),.UNSPECIFIED.,.F.,.F.,(4,3,3,
3,3,3,3,3,3,3,3,3,3,3,3,3,3,3,4),(3.73125075129679E-10,0.0423471383370935,
0.110572976501087,0.182336544287981,0.210116916270959,0.249999999999991,
0.327328028218992,0.39972985545195,0.437499999999982,0.46874999999998,0.484374999999979,
0.494232017699017,0.499999999999978,0.591939017264748,0.696116117517602,
0.771382726348881,0.878464369045677,0.957256551971924,0.99995529208901),
 .UNSPECIFIED.);
#348=B_SPLINE_CURVE_WITH_KNOTS('',3,(#61285,#61286,#61287,#61288,#61289,
#61290,#61291,#61292,#61293,#61294,#61295,#61296,#61297,#61298,#61299,#61300,
#61301,#61302,#61303,#61304,#61305,#61306,#61307,#61308,#61309,#61310,#61311,
#61312,#61313,#61314,#61315,#61316,#61317,#61318,#61319,#61320,#61321,#61322,
#61323,#61324,#61325,#61326,#61327,#61328,#61329,#61330,#61331,#61332,#61333,
#61334,#61335,#61336,#61337,#61338,#61339,#61340,#61341,#61342,#61343,#61344,
#61345,#61346,#61347,#61348,#61349,#61350,#61351,#61352,#61353,#61354,#61355,
#61356,#61357),.UNSPECIFIED.,.F.,.F.,(4,3,3,3,3,3,3,3,3,3,3,3,3,3,3,3,3,
3,3,3,3,3,3,3,4),(1.45421596525061E-9,0.0431191253444328,0.0863267720282816,
0.129382358809736,0.1428571428571,0.153643952165499,0.204633581309079,0.255730997990358,
0.2857142857143,0.306393509483645,0.370923699621223,0.4285714285714,0.459412018039415,
0.526893093159749,0.5714285714286,0.612488429098831,0.677675308967365,0.7142857142857,
0.765391329883615,0.819870817141971,0.8571428571429,0.900979337073171,0.91813936937327,
0.961788839319927,0.999999999954867),.UNSPECIFIED.);
#349=B_SPLINE_CURVE_WITH_KNOTS('',3,(#61360,#61361,#61362,#61363,#61364,
#61365,#61366,#61367,#61368,#61369,#61370,#61371,#61372,#61373,#61374,#61375,
#61376,#61377,#61378,#61379,#61380,#61381,#61382,#61383,#61384,#61385,#61386,
#61387,#61388,#61389,#61390,#61391,#61392,#61393,#61394,#61395,#61396,#61397,
#61398,#61399,#61400,#61401,#61402,#61403,#61404,#61405,#61406,#61407,#61408,
#61409,#61410,#61411,#61412,#61413,#61414,#61415,#61416,#61417,#61418,#61419,
#61420,#61421,#61422,#61423,#61424,#61425,#61426,#61427,#61428,#61429,#61430,
#61431,#61432),.UNSPECIFIED.,.F.,.F.,(4,3,3,3,3,3,3,3,3,3,3,3,3,3,3,3,3,
3,3,3,3,3,3,3,4),(0.,0.0558892627811302,0.112669257545258,0.156953426523706,
0.215052236389246,0.25000000000002,0.309316256229949,0.324310867755753,
0.385391063272203,0.437500000000035,0.468750000000038,0.484375000000039,
0.492187500000039,0.498949324581199,0.500000000000039,0.504583614223561,
0.573408717889413,0.64134390510184,0.68014577642823,0.75000000000002,0.81592675256462,
0.847891248873937,0.914669189750963,0.980716833035571,1.),.UNSPECIFIED.);
#350=B_SPLINE_CURVE_WITH_KNOTS('',3,(#61531,#61532,#61533,#61534,#61535,
#61536,#61537,#61538,#61539,#61540,#61541,#61542,#61543,#61544,#61545,#61546,
#61547,#61548,#61549,#61550,#61551,#61552,#61553,#61554,#61555,#61556,#61557,
#61558,#61559,#61560,#61561,#61562,#61563,#61564,#61565,#61566,#61567,#61568,
#61569,#61570,#61571,#61572,#61573,#61574,#61575,#61576,#61577,#61578,#61579,
#61580,#61581,#61582,#61583,#61584,#61585,#61586,#61587,#61588,#61589,#61590,
#61591,#61592,#61593,#61594,#61595,#61596,#61597,#61598,#61599,#61600,#61601,
#61602,#61603,#61604,#61605,#61606,#61607,#61608,#61609,#61610,#61611,#61612,
#61613,#61614,#61615,#61616,#61617,#61618,#61619,#61620,#61621,#61622,#61623,
#61624,#61625,#61626,#61627,#61628,#61629,#61630,#61631,#61632,#61633,#61634,
#61635,#61636,#61637,#61638,#61639,#61640,#61641,#61642,#61643,#61644,#61645,
#61646,#61647,#61648,#61649,#61650,#61651,#61652,#61653,#61654,#61655,#61656,
#61657,#61658,#61659,#61660,#61661,#61662,#61663,#61664,#61665,#61666,#61667,
#61668,#61669,#61670,#61671,#61672,#61673,#61674,#61675,#61676,#61677,#61678,
#61679,#61680,#61681,#61682,#61683,#61684,#61685,#61686,#61687,#61688,#61689,
#61690,#61691,#61692,#61693,#61694,#61695,#61696),.UNSPECIFIED.,.F.,.F.,
(4,3,3,3,3,3,3,3,3,3,3,3,3,3,3,3,3,3,3,3,3,3,3,3,3,3,3,3,3,3,3,3,3,3,3,
3,3,3,3,3,3,3,3,3,3,3,3,3,3,3,3,3,3,3,3,4),(8.91470519372192E-8,0.0341843291030202,
0.0624999999999999,0.0799991073633813,0.0937499999999998,0.109375,0.1171875,
0.12109375,0.123046875,0.125,0.156854101554739,0.1875,0.21875,0.234375,
0.237493486952361,0.2421875,0.24609375,0.248046875,0.25,0.290848999557458,
0.312500000000001,0.328904221360791,0.343750000000002,0.359375000000002,
0.367187500000002,0.371093750000002,0.373046875000002,0.375000000000002,
0.425200709948369,0.437500000000002,0.468750000000002,0.484375000000002,
0.492187500000002,0.496093750000002,0.500000000000002,0.520161000661623,
0.57260995086379,0.616925907134883,0.625000000000001,0.651314116776,0.678193288479241,
0.687500000000001,0.709191597556237,0.750000000000001,0.781250000000001,
0.789062500000001,0.796875000000001,0.799101080805048,0.812500000000001,
0.858392460401059,0.875000000000001,0.885508810391372,0.932690672165831,
0.980791435666233,0.985732819345807,1.),.UNSPECIFIED.);
#351=B_SPLINE_CURVE_WITH_KNOTS('',3,(#61699,#61700,#61701,#61702,#61703,
#61704,#61705,#61706,#61707,#61708,#61709,#61710,#61711,#61712,#61713,#61714,
#61715,#61716,#61717,#61718,#61719,#61720,#61721,#61722,#61723,#61724,#61725,
#61726,#61727,#61728,#61729,#61730,#61731,#61732,#61733,#61734,#61735,#61736,
#61737,#61738,#61739,#61740,#61741,#61742,#61743,#61744,#61745,#61746,#61747,
#61748,#61749,#61750,#61751,#61752,#61753,#61754,#61755,#61756,#61757,#61758,
#61759,#61760,#61761,#61762,#61763,#61764,#61765,#61766,#61767,#61768,#61769,
#61770,#61771,#61772,#61773,#61774,#61775,#61776,#61777,#61778,#61779,#61780,
#61781,#61782,#61783,#61784,#61785,#61786,#61787,#61788,#61789,#61790,#61791,
#61792,#61793,#61794,#61795,#61796,#61797,#61798,#61799,#61800,#61801,#61802,
#61803,#61804,#61805,#61806,#61807,#61808,#61809,#61810,#61811,#61812,#61813,
#61814,#61815,#61816,#61817,#61818,#61819,#61820,#61821,#61822,#61823,#61824,
#61825,#61826,#61827,#61828,#61829,#61830,#61831,#61832,#61833,#61834,#61835,
#61836,#61837,#61838,#61839,#61840),.UNSPECIFIED.,.F.,.F.,(4,3,3,3,3,3,
3,3,3,3,3,3,3,3,3,3,3,3,3,3,3,3,3,3,3,3,3,3,3,3,3,3,3,3,3,3,3,3,3,3,3,3,
3,3,3,3,3,4),(2.34637985974789E-7,0.031595826091221,0.062896465800433,0.0937122471496095,
0.104172266518684,0.124999999999998,0.154837351378791,0.184674702757584,
0.213176019980234,0.218749999999996,0.234374999999996,0.242187499999996,
0.246093749999995,0.248046874999995,0.249999999999996,0.257790681019999,
0.295642689870312,0.334483658793269,0.354334778645037,0.39268306807659,
0.431398782256473,0.470481835057029,0.48237572788559,0.484374999999997,
0.496585735733692,0.499999999999997,0.540377615423201,0.580372331065526,
0.609453985246043,0.649164804655767,0.687499999999999,0.700831465154267,
0.718749999999999,0.734374999999999,0.742187499999999,0.746093749999999,
0.748046874999999,0.749999999999999,0.769091486017791,0.798966759489123,
0.828842032960455,0.858576939735652,0.874999999999999,0.896782274077063,
0.927914209698524,0.959582410600718,0.985641670858647,1.),.UNSPECIFIED.);
#352=B_SPLINE_CURVE_WITH_KNOTS('',3,(#61877,#61878,#61879,#61880,#61881,
#61882,#61883,#61884,#61885,#61886,#61887,#61888,#61889,#61890,#61891,#61892,
#61893,#61894,#61895,#61896,#61897,#61898,#61899,#61900,#61901,#61902,#61903,
#61904,#61905,#61906,#61907,#61908,#61909,#61910,#61911,#61912,#61913,#61914,
#61915,#61916,#61917,#61918,#61919,#61920,#61921,#61922,#61923,#61924,#61925,
#61926,#61927,#61928,#61929,#61930,#61931,#61932,#61933,#61934,#61935,#61936,
#61937),.UNSPECIFIED.,.F.,.F.,(4,3,3,3,3,3,3,3,3,3,3,3,3,3,3,3,3,3,3,3,
4),(3.81436972404066E-8,0.0594692341193173,0.119461353288053,0.180335257934325,
0.228233369909761,0.250000000000001,0.312500000000001,0.375000000000001,
0.420630665240657,0.466482701433567,0.5,0.532982727135479,0.595584458307783,
0.657507423778217,0.718468767547966,0.75,0.80983093432658,0.831293916785482,
0.890887278795621,0.949594741146851,1.),.UNSPECIFIED.);
#353=B_SPLINE_CURVE_WITH_KNOTS('',3,(#61938,#61939,#61940,#61941,#61942,
#61943,#61944,#61945,#61946,#61947,#61948,#61949,#61950,#61951,#61952,#61953,
#61954,#61955,#61956,#61957,#61958,#61959,#61960,#61961,#61962,#61963,#61964,
#61965,#61966,#61967,#61968,#61969,#61970,#61971,#61972,#61973,#61974,#61975,
#61976,#61977,#61978,#61979,#61980,#61981,#61982,#61983,#61984,#61985,#61986,
#61987,#61988,#61989,#61990,#61991,#61992,#61993,#61994,#61995),
 .UNSPECIFIED.,.F.,.F.,(4,3,3,3,3,3,3,3,3,3,3,3,3,3,3,3,3,3,3,4),(0.,0.0706357924192512,
0.136905894358846,0.198469767880529,0.25,0.307239195840158,0.363641873526663,
0.419667860479303,0.475290932764254,0.49995510889698,0.5,0.555615247434432,
0.61170547306681,0.668168214199068,0.725338437553129,0.75,0.8125,0.877100936211395,
0.947886389184427,1.),.UNSPECIFIED.);
#354=B_SPLINE_CURVE_WITH_KNOTS('',3,(#62038,#62039,#62040,#62041,#62042,
#62043,#62044,#62045,#62046,#62047,#62048,#62049,#62050,#62051,#62052,#62053,
#62054,#62055,#62056,#62057,#62058,#62059,#62060,#62061,#62062,#62063,#62064,
#62065,#62066,#62067,#62068,#62069,#62070,#62071,#62072,#62073,#62074,#62075,
#62076,#62077,#62078,#62079,#62080,#62081,#62082,#62083,#62084,#62085,#62086,
#62087,#62088,#62089,#62090,#62091,#62092,#62093,#62094,#62095,#62096,#62097,
#62098,#62099,#62100,#62101,#62102,#62103,#62104,#62105,#62106,#62107,#62108,
#62109,#62110,#62111,#62112,#62113,#62114,#62115,#62116,#62117,#62118,#62119,
#62120,#62121,#62122),.UNSPECIFIED.,.F.,.F.,(4,3,3,3,3,3,3,3,3,3,3,3,3,
3,3,3,3,3,3,3,3,3,3,3,3,3,3,3,4),(0.,0.070984038243982,0.124999999999996,
0.187499999999995,0.218749999999994,0.234374999999994,0.242187499999994,
0.244541813992091,0.246093749999993,0.249999999999993,0.318695715793694,
0.386222190629079,0.414616854789881,0.482181913540056,0.499999999999994,
0.565353689470601,0.585548104938381,0.624999999999995,0.687499999999995,
0.718749999999995,0.734374999999995,0.742187499999995,0.746093749999995,
0.749999999999995,0.755626562870562,0.823511777763023,0.893068528416106,
0.929166670310745,1.),.UNSPECIFIED.);
#355=B_SPLINE_CURVE_WITH_KNOTS('',3,(#62165,#62166,#62167,#62168,#62169,
#62170,#62171,#62172,#62173,#62174,#62175,#62176,#62177,#62178,#62179,#62180,
#62181,#62182,#62183,#62184,#62185,#62186,#62187,#62188,#62189,#62190,#62191,
#62192,#62193,#62194,#62195),.UNSPECIFIED.,.F.,.F.,(4,3,3,3,3,3,3,3,3,3,
4),(0.,0.125000000000036,0.187500000000053,0.21875000000006,0.234375000000062,
0.242187500000063,0.250000000000064,0.375000000000053,0.500000000000043,
0.750000000000021,1.),.UNSPECIFIED.);
#356=B_SPLINE_CURVE_WITH_KNOTS('',3,(#62196,#62197,#62198,#62199,#62200,
#62201,#62202,#62203,#62204,#62205,#62206,#62207,#62208,#62209,#62210,#62211),
 .UNSPECIFIED.,.F.,.F.,(4,3,3,3,3,4),(0.,0.305738962927125,0.3333333333333,
0.6666666666667,0.964886280950195,1.),.UNSPECIFIED.);
#357=B_SPLINE_CURVE_WITH_KNOTS('',3,(#62212,#62213,#62214,#62215,#62216,
#62217,#62218,#62219,#62220,#62221,#62222,#62223,#62224,#62225,#62226,#62227,
#62228,#62229,#62230,#62231,#62232,#62233,#62234,#62235,#62236,#62237,#62238,
#62239,#62240,#62241,#62242,#62243,#62244,#62245,#62246,#62247,#62248,#62249,
#62250,#62251,#62252,#62253,#62254,#62255,#62256,#62257,#62258,#62259,#62260,
#62261,#62262,#62263,#62264,#62265,#62266,#62267,#62268,#62269,#62270,#62271,
#62272,#62273,#62274,#62275),.UNSPECIFIED.,.F.,.F.,(4,3,3,3,3,3,3,3,3,3,
3,3,3,3,3,3,3,3,3,3,3,4),(0.,0.0446614606293701,0.151711825344438,0.230164819186069,
0.25,0.354548286934243,0.375000000000001,0.409260647438796,0.437500000000001,
0.46875,0.484375,0.493953369682669,0.500000000000001,0.580864109044975,
0.601341896293497,0.678602986469359,0.75,0.790540546335742,0.862585242307717,
0.931006462747741,0.957944183693305,1.),.UNSPECIFIED.);
#358=B_SPLINE_CURVE_WITH_KNOTS('',3,(#62318,#62319,#62320,#62321,#62322,
#62323,#62324,#62325,#62326,#62327,#62328,#62329,#62330,#62331,#62332,#62333,
#62334,#62335,#62336,#62337,#62338,#62339,#62340,#62341,#62342,#62343,#62344,
#62345,#62346,#62347,#62348,#62349,#62350,#62351,#62352,#62353,#62354,#62355,
#62356,#62357,#62358,#62359,#62360,#62361,#62362,#62363,#62364,#62365,#62366,
#62367,#62368,#62369,#62370,#62371,#62372,#62373,#62374,#62375,#62376,#62377,
#62378,#62379,#62380,#62381,#62382,#62383,#62384,#62385,#62386,#62387,#62388,
#62389,#62390,#62391,#62392,#62393,#62394,#62395,#62396,#62397,#62398,#62399,
#62400,#62401,#62402,#62403,#62404,#62405,#62406,#62407,#62408),
 .UNSPECIFIED.,.F.,.F.,(4,3,3,3,3,3,3,3,3,3,3,3,3,3,3,3,3,3,3,3,3,3,3,3,
3,3,3,3,3,3,4),(1.98906486742311E-7,0.0470898534984864,0.0950876880993247,
0.10952642980478,0.125000000000006,0.17668496847957,0.18750000000001,0.195574841561927,
0.20312500000001,0.21875000000001,0.250000000000011,0.270621656389179,0.334104136527559,
0.398265387134923,0.430414690770554,0.437500000000015,0.468750000000015,
0.484375000000015,0.492187500000015,0.498034130470392,0.500000000000015,
0.559924746618581,0.600124931584257,0.658475281491341,0.715889390715269,
0.7642505253901,0.821849983871512,0.878616196067142,0.918178937043819,0.970962456769612,
1.),.UNSPECIFIED.);
#359=B_SPLINE_CURVE_WITH_KNOTS('',3,(#62453,#62454,#62455,#62456,#62457,
#62458,#62459,#62460,#62461,#62462,#62463,#62464,#62465,#62466,#62467,#62468,
#62469,#62470,#62471,#62472,#62473,#62474,#62475,#62476,#62477,#62478,#62479,
#62480,#62481,#62482,#62483,#62484,#62485,#62486,#62487,#62488,#62489,#62490,
#62491,#62492,#62493,#62494,#62495,#62496,#62497,#62498,#62499,#62500,#62501,
#62502,#62503,#62504,#62505,#62506,#62507,#62508,#62509,#62510),
 .UNSPECIFIED.,.F.,.F.,(4,3,3,3,3,3,3,3,3,3,3,3,3,3,3,3,3,3,3,4),(0.,0.0625,
0.123433376418121,0.183427620822819,0.242367644898908,0.25,0.308040515079698,
0.365337471650276,0.42229797384171,0.479065208678401,0.535781347576013,
0.592773854696921,0.649986866374424,0.707857241876389,0.75,0.808902570121928,
0.869152639395624,0.930295239220506,0.992904488662291,1.),.UNSPECIFIED.);
#360=B_SPLINE_CURVE_WITH_KNOTS('',3,(#62512,#62513,#62514,#62515,#62516,
#62517,#62518,#62519,#62520,#62521,#62522,#62523,#62524,#62525,#62526,#62527),
 .UNSPECIFIED.,.F.,.F.,(4,3,3,3,3,4),(0.,0.298778860875572,0.3333333333333,
0.6666666666667,0.972465952980625,1.),.UNSPECIFIED.);
#361=B_SPLINE_CURVE_WITH_KNOTS('',3,(#62529,#62530,#62531,#62532,#62533,
#62534,#62535,#62536,#62537,#62538,#62539),.UNSPECIFIED.,.F.,.F.,(4,1,2,
2,2,4),(0.,0.125000000000002,0.218750000000005,0.250000000000005,0.500000000000003,
1.),.UNSPECIFIED.);
#362=B_SPLINE_CURVE_WITH_KNOTS('',3,(#62540,#62541,#62542,#62543,#62544,
#62545,#62546,#62547,#62548,#62549,#62550,#62551,#62552,#62553,#62554,#62555,
#62556,#62557,#62558,#62559,#62560,#62561,#62562,#62563,#62564,#62565,#62566,
#62567,#62568,#62569,#62570,#62571,#62572,#62573,#62574,#62575,#62576,#62577,
#62578,#62579,#62580,#62581,#62582,#62583,#62584,#62585,#62586,#62587,#62588,
#62589,#62590,#62591,#62592,#62593,#62594,#62595,#62596,#62597),
 .UNSPECIFIED.,.F.,.F.,(4,3,3,3,3,3,3,3,3,3,3,3,3,3,3,3,3,3,3,4),(6.11814853262804E-10,
0.0417521477615177,0.109880939803693,0.181543350593602,0.209151847901313,
0.250000000000004,0.32674556824041,0.375000000000005,0.39835952915245,0.437500000000006,
0.468750000000008,0.484375000000009,0.494227622931881,0.500000000000011,
0.590539736464595,0.694718942696452,0.769679430141417,0.876793017787304,
0.95521013021045,0.99999999997903),.UNSPECIFIED.);
#363=B_SPLINE_CURVE_WITH_KNOTS('',3,(#62639,#62640,#62641,#62642,#62643,
#62644,#62645,#62646,#62647,#62648,#62649,#62650,#62651,#62652,#62653,#62654,
#62655,#62656,#62657,#62658,#62659,#62660,#62661,#62662,#62663,#62664,#62665,
#62666,#62667,#62668,#62669,#62670,#62671,#62672,#62673,#62674,#62675,#62676,
#62677,#62678,#62679,#62680,#62681,#62682,#62683,#62684,#62685,#62686,#62687,
#62688,#62689,#62690,#62691,#62692,#62693,#62694,#62695,#62696,#62697,#62698,
#62699,#62700,#62701,#62702,#62703,#62704,#62705,#62706,#62707,#62708,#62709,
#62710,#62711,#62712,#62713,#62714,#62715,#62716,#62717,#62718,#62719,#62720,
#62721,#62722,#62723,#62724,#62725,#62726),.UNSPECIFIED.,.F.,.F.,(4,3,3,
3,3,3,3,3,3,3,3,3,3,3,3,3,3,3,3,3,3,3,3,3,3,3,3,3,3,4),(3.70263034175187E-11,
0.0527820564885111,0.081821354966552,0.138473187136047,0.195945331196402,
0.235750067891708,0.29301224024971,0.351193499636413,0.399875474066281,
0.437499999999966,0.468749999999963,0.484374999999962,0.492187499999962,
0.496093749999963,0.499508596624892,0.499999999999963,0.565860737136916,
0.629574800820601,0.69395872836067,0.725750995729374,0.781249999999981,
0.790730859889013,0.796874999999982,0.812499999999984,0.869043375183258,
0.874999999999989,0.884835790315371,0.938700861559312,0.993360752892644,
0.99999977775045),.UNSPECIFIED.);
#364=B_SPLINE_CURVE_WITH_KNOTS('',3,(#62729,#62730,#62731,#62732,#62733,
#62734,#62735,#62736,#62737,#62738,#62739,#62740,#62741,#62742,#62743,#62744,
#62745,#62746,#62747,#62748,#62749,#62750,#62751,#62752,#62753,#62754,#62755,
#62756,#62757,#62758,#62759,#62760,#62761,#62762,#62763,#62764,#62765,#62766,
#62767,#62768,#62769,#62770,#62771,#62772,#62773,#62774,#62775,#62776,#62777,
#62778,#62779,#62780,#62781,#62782,#62783,#62784,#62785,#62786),
 .UNSPECIFIED.,.F.,.F.,(4,3,3,3,3,3,3,3,3,3,3,3,3,3,3,3,3,3,3,4),(0.,0.0585633378234075,
0.117996984449599,0.168707880043306,0.228541703309256,0.250000000000001,
0.312500000000001,0.375000000000001,0.421054217354142,0.467108434708283,
0.500000000000001,0.563532905575853,0.626399541702303,0.688223265291581,
0.750000000000001,0.771768807379113,0.83260584823571,0.892881414097024,
0.952306973405338,0.999999961863691),.UNSPECIFIED.);
#365=B_SPLINE_CURVE_WITH_KNOTS('',3,(#62837,#62838,#62839,#62840,#62841,
#62842,#62843,#62844,#62845,#62846,#62847,#62848,#62849,#62850,#62851,#62852,
#62853,#62854,#62855,#62856,#62857,#62858,#62859,#62860,#62861,#62862,#62863,
#62864,#62865,#62866,#62867,#62868,#62869,#62870,#62871,#62872,#62873,#62874,
#62875,#62876,#62877,#62878,#62879,#62880,#62881,#62882,#62883,#62884,#62885,
#62886,#62887,#62888,#62889,#62890,#62891,#62892,#62893,#62894,#62895,#62896,
#62897,#62898,#62899,#62900,#62901,#62902,#62903,#62904,#62905,#62906,#62907,
#62908,#62909,#62910,#62911,#62912,#62913,#62914,#62915,#62916,#62917,#62918,
#62919,#62920,#62921,#62922,#62923,#62924,#62925,#62926,#62927,#62928,#62929,
#62930,#62931,#62932,#62933,#62934,#62935,#62936,#62937,#62938,#62939,#62940,
#62941,#62942,#62943,#62944,#62945,#62946,#62947,#62948,#62949,#62950,#62951,
#62952,#62953,#62954,#62955,#62956,#62957,#62958,#62959,#62960,#62961,#62962,
#62963,#62964,#62965,#62966,#62967,#62968,#62969,#62970,#62971,#62972,#62973,
#62974,#62975,#62976,#62977,#62978,#62979,#62980,#62981,#62982,#62983,#62984,
#62985,#62986,#62987,#62988,#62989,#62990,#62991,#62992,#62993,#62994,#62995,
#62996,#62997,#62998,#62999,#63000,#63001,#63002,#63003,#63004,#63005,#63006,
#63007,#63008,#63009,#63010,#63011,#63012,#63013,#63014,#63015,#63016,#63017,
#63018,#63019,#63020,#63021,#63022,#63023,#63024,#63025,#63026,#63027,#63028,
#63029,#63030,#63031,#63032,#63033,#63034,#63035,#63036,#63037,#63038,#63039,
#63040,#63041,#63042,#63043,#63044,#63045,#63046,#63047,#63048,#63049,#63050,
#63051,#63052,#63053,#63054,#63055,#63056,#63057,#63058,#63059,#63060,#63061,
#63062,#63063,#63064,#63065,#63066,#63067,#63068,#63069,#63070,#63071,#63072,
#63073,#63074,#63075,#63076,#63077,#63078,#63079,#63080),.UNSPECIFIED.,
 .F.,.F.,(4,3,3,3,3,3,3,3,3,3,3,3,3,3,3,3,3,3,3,3,3,3,3,3,3,3,3,3,3,3,3,
3,3,3,3,3,3,3,3,3,3,3,3,3,3,3,3,3,3,3,3,3,3,3,3,3,3,3,3,3,3,3,3,3,3,3,3,
3,3,3,3,3,3,3,3,3,3,3,3,3,3,4),(9.73806164256783E-8,0.0159281142913431,
0.0312500000000213,0.046875000000032,0.0546875000000373,0.0585937500000399,
0.0625000000000424,0.0648418039613322,0.0836785664054461,0.102452808361369,
0.109375000000073,0.117187500000078,0.121093750000081,0.123046875000082,
0.124023437500082,0.124511718750083,0.125000000000083,0.130859030271114,
0.14559909038106,0.160253323380513,0.17187500000009,0.179687500000091,0.183593750000092,
0.185546875000092,0.186523437500093,0.187500000000093,0.198325694518741,
0.209109868210274,0.213418238445796,0.224168357782371,0.234847785721346,
0.242187500000105,0.246093750000106,0.248046875000107,0.249023437500107,
0.249755859375107,0.250000000000107,0.286107610092526,0.331138076209162,
0.373109057199251,0.413997211211172,0.437500000000133,0.442041901806469,
0.468750000000137,0.484375000000139,0.49218750000014,0.496093750000141,
0.498046875000141,0.498820943136186,0.499023437500141,0.499511718750141,
0.500000000000141,0.527811010006352,0.555639881747458,0.580242634713494,
0.608313865295241,0.634725967382553,0.640625000000156,0.645735141626808,
0.648437500000157,0.665748936028716,0.677911470409284,0.695416726989991,
0.713007949879031,0.730688053588786,0.734375000000167,0.742187500000168,
0.746093750000168,0.748046875000168,0.749023437500168,0.749511718750168,
0.750000000000167,0.752509339484753,0.797992313705749,0.804152672765917,
0.850548065526046,0.858799535654424,0.906291712294993,0.920210727170671,
0.968985942526481,0.993036925597939,1.),.UNSPECIFIED.);
#366=B_SPLINE_CURVE_WITH_KNOTS('',3,(#63163,#63164,#63165,#63166,#63167,
#63168,#63169,#63170,#63171,#63172,#63173,#63174,#63175,#63176,#63177,#63178,
#63179,#63180,#63181,#63182,#63183,#63184,#63185,#63186,#63187,#63188,#63189,
#63190,#63191,#63192,#63193,#63194,#63195,#63196,#63197,#63198,#63199,#63200,
#63201,#63202,#63203,#63204,#63205,#63206,#63207,#63208,#63209,#63210,#63211,
#63212,#63213,#63214,#63215,#63216,#63217,#63218,#63219,#63220,#63221,#63222,
#63223,#63224,#63225,#63226,#63227,#63228,#63229,#63230,#63231,#63232,#63233,
#63234,#63235,#63236,#63237,#63238,#63239,#63240,#63241,#63242,#63243,#63244,
#63245,#63246,#63247,#63248,#63249,#63250,#63251,#63252,#63253,#63254,#63255,
#63256,#63257,#63258,#63259,#63260,#63261,#63262,#63263,#63264,#63265,#63266,
#63267,#63268,#63269,#63270,#63271,#63272,#63273,#63274,#63275,#63276,#63277,
#63278,#63279,#63280,#63281,#63282,#63283,#63284,#63285,#63286,#63287,#63288,
#63289,#63290,#63291,#63292,#63293,#63294,#63295,#63296,#63297,#63298,#63299,
#63300,#63301,#63302,#63303,#63304,#63305,#63306,#63307,#63308,#63309,#63310,
#63311,#63312,#63313,#63314,#63315,#63316,#63317,#63318,#63319),
 .UNSPECIFIED.,.F.,.F.,(4,3,3,3,3,3,3,3,3,3,3,3,3,3,3,3,3,3,3,3,3,3,3,3,
3,3,3,3,3,3,3,3,3,3,3,3,3,3,3,3,3,3,3,3,3,3,3,3,3,3,3,3,4),(1.72726438405786E-7,
0.0434573164719052,0.086333854898234,0.0932163022794985,0.124999999999983,
0.165840014184437,0.177272634924799,0.187499999999974,0.218749999999969,
0.234374999999967,0.242187499999966,0.246093749999966,0.249511718749965,
0.249999999999965,0.260112422138339,0.284903851802453,0.309600945382747,
0.312499999999968,0.336932311116222,0.343749999999969,0.359374999999969,
0.35974136967626,0.36718749999997,0.37109374999997,0.37304687499997,0.37402343749997,
0.37499999999997,0.42716199723274,0.437499999999972,0.446539738539256,0.468749999999974,
0.484374999999974,0.492187499999975,0.499058231412271,0.499999999999975,
0.529373583917037,0.595489913988851,0.601626215812586,0.62499999999998,
0.666788584072113,0.687499999999983,0.718749999999984,0.726756725922575,
0.734374999999985,0.746093749999985,0.749999999999985,0.777566925552718,
0.821932091724188,0.864145581838811,0.906142545834475,0.94972718006945,
0.995919147870662,0.999999956000501),.UNSPECIFIED.);
#367=B_SPLINE_CURVE_WITH_KNOTS('',3,(#63364,#63365,#63366,#63367,#63368,
#63369,#63370,#63371,#63372,#63373,#63374,#63375,#63376,#63377,#63378,#63379,
#63380,#63381,#63382,#63383,#63384,#63385,#63386,#63387,#63388,#63389,#63390,
#63391,#63392,#63393,#63394),.UNSPECIFIED.,.F.,.F.,(4,3,3,3,3,3,3,3,3,3,
4),(0.,0.125,0.187500000000001,0.218750000000001,0.234375000000002,0.242187500000001,
0.25,0.375,0.500000000000001,0.75,1.),.UNSPECIFIED.);
#368=B_SPLINE_CURVE_WITH_KNOTS('',3,(#63396,#63397,#63398,#63399,#63400,
#63401,#63402,#63403,#63404,#63405,#63406,#63407,#63408,#63409,#63410,#63411),
 .UNSPECIFIED.,.F.,.F.,(4,3,3,3,3,4),(0.000149798704371109,0.305896512638586,
0.3333333333333,0.6666666666667,0.965406965005641,1.),.UNSPECIFIED.);
#369=B_SPLINE_CURVE_WITH_KNOTS('',3,(#63414,#63415,#63416,#63417,#63418,
#63419,#63420,#63421,#63422,#63423,#63424,#63425,#63426,#63427,#63428,#63429,
#63430,#63431,#63432,#63433,#63434,#63435,#63436,#63437,#63438,#63439,#63440,
#63441,#63442,#63443,#63444,#63445,#63446,#63447,#63448,#63449,#63450,#63451,
#63452,#63453,#63454,#63455,#63456,#63457,#63458,#63459,#63460,#63461,#63462,
#63463,#63464,#63465,#63466,#63467,#63468,#63469,#63470,#63471,#63472,#63473,
#63474),.UNSPECIFIED.,.F.,.F.,(4,3,3,3,3,3,3,3,3,3,3,3,3,3,3,3,3,3,3,3,
4),(3.35491904938007E-5,0.0428738058325973,0.149949773961846,0.228787916593128,
0.249999999999993,0.353669955295993,0.408269673424094,0.437499999999988,
0.468749999999987,0.484374999999986,0.493967232192623,0.499999999999985,
0.580997102510811,0.600490344305326,0.677895850195905,0.749999999999992,
0.790086401711803,0.862285218947932,0.930853411259674,0.957922464653335,
1.),.UNSPECIFIED.);
#370=B_SPLINE_CURVE_WITH_KNOTS('',3,(#63519,#63520,#63521,#63522,#63523,
#63524,#63525,#63526,#63527,#63528,#63529,#63530,#63531,#63532,#63533,#63534,
#63535,#63536,#63537,#63538,#63539,#63540,#63541,#63542,#63543,#63544,#63545,
#63546,#63547,#63548,#63549,#63550,#63551,#63552,#63553,#63554,#63555,#63556,
#63557,#63558,#63559,#63560,#63561,#63562,#63563,#63564,#63565,#63566,#63567,
#63568,#63569,#63570,#63571,#63572,#63573,#63574,#63575,#63576,#63577,#63578,
#63579,#63580,#63581,#63582,#63583,#63584,#63585,#63586,#63587,#63588),
 .UNSPECIFIED.,.F.,.F.,(4,3,3,3,3,3,3,3,3,3,3,3,3,3,3,3,3,3,3,3,3,3,3,4),
(0.,0.0436825089787147,0.0764111191074181,0.120245150899802,0.125,0.179962620954868,
0.223835356148353,0.25,0.320059899745086,0.371520369824615,0.375,0.470560242042003,
0.5,0.519394870001365,0.625,0.667284556518977,0.74166723255934,0.75,0.808039637084786,
0.814941565949557,0.875,0.919746518923496,0.962447676465487,0.999999720259695),
 .UNSPECIFIED.);
#371=B_SPLINE_CURVE_WITH_KNOTS('',3,(#63589,#63590,#63591,#63592,#63593,
#63594,#63595,#63596,#63597,#63598,#63599,#63600,#63601,#63602,#63603,#63604,
#63605,#63606,#63607,#63608,#63609,#63610,#63611,#63612,#63613,#63614,#63615,
#63616,#63617,#63618,#63619,#63620,#63621,#63622,#63623,#63624,#63625,#63626,
#63627,#63628,#63629,#63630,#63631,#63632,#63633,#63634,#63635,#63636,#63637,
#63638,#63639,#63640,#63641,#63642,#63643,#63644,#63645,#63646,#63647,#63648,
#63649,#63650,#63651,#63652,#63653,#63654,#63655,#63656,#63657,#63658),
 .UNSPECIFIED.,.F.,.F.,(4,3,3,3,3,3,3,3,3,3,3,3,3,3,3,3,3,3,3,3,3,3,3,4),
(0.,0.0642455417156636,0.12922356065871,0.13964895033816,0.203364207353361,
0.250000000000001,0.300656467909375,0.369078233954689,0.437500000000003,
0.468750000000003,0.469711899594866,0.484375000000003,0.495154873957857,
0.500000000000003,0.56333468259713,0.625630678898964,0.644015076010612,
0.704247191865364,0.750000000000002,0.807879472775742,0.868482121788547,
0.928163066010689,0.961961794088669,0.999999992441328),.UNSPECIFIED.);
#372=B_SPLINE_CURVE_WITH_KNOTS('',3,(#63694,#63695,#63696,#63697,#63698,
#63699,#63700,#63701,#63702,#63703,#63704,#63705,#63706,#63707,#63708,#63709,
#63710,#63711,#63712,#63713,#63714,#63715,#63716,#63717,#63718,#63719,#63720,
#63721,#63722,#63723,#63724,#63725,#63726,#63727,#63728,#63729,#63730,#63731,
#63732,#63733,#63734,#63735,#63736,#63737,#63738,#63739,#63740,#63741,#63742,
#63743,#63744,#63745,#63746,#63747,#63748,#63749,#63750,#63751),
 .UNSPECIFIED.,.F.,.F.,(4,3,3,3,3,3,3,3,3,3,3,3,3,3,3,3,3,3,3,4),(0.,0.0706905706112055,
0.137002900415584,0.198600023213015,0.25,0.306961952173985,0.36310537274714,
0.418882023364704,0.474267462741273,0.5,0.500045996220446,0.555660447642905,
0.611744482007949,0.668197862686385,0.725353764962349,0.75,0.8125,0.877037176849364,
0.947733158289997,1.),.UNSPECIFIED.);
#373=B_SPLINE_CURVE_WITH_KNOTS('',3,(#63792,#63793,#63794,#63795,#63796,
#63797,#63798,#63799,#63800,#63801,#63802,#63803,#63804,#63805,#63806,#63807,
#63808,#63809,#63810,#63811,#63812,#63813,#63814,#63815,#63816,#63817,#63818,
#63819,#63820,#63821,#63822,#63823,#63824,#63825,#63826,#63827,#63828,#63829,
#63830,#63831,#63832,#63833,#63834,#63835,#63836,#63837,#63838,#63839,#63840,
#63841,#63842,#63843,#63844,#63845,#63846,#63847,#63848,#63849,#63850,#63851,
#63852,#63853,#63854,#63855,#63856,#63857,#63858,#63859,#63860,#63861,#63862,
#63863,#63864,#63865,#63866,#63867,#63868,#63869,#63870,#63871,#63872,#63873,
#63874,#63875,#63876),.UNSPECIFIED.,.F.,.F.,(4,3,3,3,3,3,3,3,3,3,3,3,3,
3,3,3,3,3,3,3,3,3,3,3,3,3,3,3,4),(0.,0.0706625665957282,0.124999999999996,
0.187499999999994,0.218749999999993,0.234374999999993,0.242187499999993,
0.244252489601095,0.246093749999993,0.249999999999993,0.317448736797841,
0.383780163038669,0.414395823559992,0.480730288139021,0.499999999999993,
0.565325738265915,0.585446949397997,0.624999999999993,0.687499999999993,
0.718749999999993,0.734374999999993,0.742187499999993,0.746093749999993,
0.749999999999993,0.755577493927536,0.823473673311783,0.893041632226348,
0.929181432390663,1.),.UNSPECIFIED.);
#374=B_SPLINE_CURVE_WITH_KNOTS('',3,(#64255,#64256,#64257,#64258,#64259,
#64260,#64261,#64262,#64263,#64264,#64265,#64266,#64267,#64268,#64269,#64270,
#64271,#64272),.UNSPECIFIED.,.F.,.F.,(4,2,2,2,2,2,2,2,4),(0.567634871268155,
0.624046753014798,0.75751040349095,0.849653931021769,0.941797458552588,
1.03394098608341,1.12608451361423,1.25954816409038,1.39301181456653),
 .UNSPECIFIED.);
#375=B_SPLINE_CURVE_WITH_KNOTS('',3,(#64273,#64274,#64275,#64276,#64277,
#64278,#64279,#64280,#64281,#64282,#64283,#64284,#64285,#64286,#64287,#64288,
#64289,#64290,#64291,#64292,#64293,#64294,#64295,#64296,#64297),
 .UNSPECIFIED.,.F.,.F.,(4,2,2,2,2,3,2,2,2,2,2,4),(1.39301181456653,1.54288207354412,
1.6927523325217,1.78817362481344,1.83588427095931,1.88359491710518,1.93130556325105,
1.97901620939691,2.07443750168865,2.22430776066624,2.37417801964382,2.45122978837333),
 .UNSPECIFIED.);
#376=B_SPLINE_CURVE_WITH_KNOTS('',3,(#64301,#64302,#64303,#64304,#64305,
#64306,#64307,#64308,#64309,#64310,#64311,#64312,#64313,#64314,#64315,#64316,
#64317,#64318,#64319,#64320,#64321,#64322,#64323,#64324,#64325,#64326,#64327,
#64328,#64329,#64330),.UNSPECIFIED.,.F.,.F.,(4,2,2,2,2,2,2,2,2,2,2,2,2,
2,4),(-3.98325608634761,-3.86919217467992,-3.49972652065679,-3.13026086663367,
-2.85088285941717,-2.57150485220067,-2.36940240571059,-2.16729995922052,
-1.96519751273044,-1.76309506624036,-1.48371705902386,-1.20433905180736,
-0.83487339778424,-0.465407743761119,-0.35134383209342),.UNSPECIFIED.);
#377=B_SPLINE_CURVE_WITH_KNOTS('',3,(#64366,#64367,#64368,#64369,#64370,
#64371,#64372,#64373,#64374,#64375,#64376,#64377,#64378,#64379,#64380,#64381,
#64382,#64383,#64384,#64385,#64386,#64387,#64388,#64389,#64390,#64391,#64392,
#64393,#64394,#64395),.UNSPECIFIED.,.F.,.F.,(4,2,2,2,2,2,2,2,2,2,2,2,2,
2,4),(-3.98325608634761,-3.86919217467992,-3.49972652065679,-3.13026086663367,
-2.85088285941717,-2.57150485220067,-2.36940240571059,-2.16729995922052,
-1.96519751273044,-1.76309506624036,-1.48371705902386,-1.20433905180736,
-0.83487339778424,-0.465407743761118,-0.35134383209342),.UNSPECIFIED.);
#378=B_SPLINE_CURVE_WITH_KNOTS('',3,(#64412,#64413,#64414,#64415,#64416,
#64417,#64418,#64419,#64420,#64421,#64422,#64423,#64424,#64425,#64426,#64427,
#64428,#64429,#64430,#64431,#64432,#64433,#64434,#64435,#64436,#64437,#64438,
#64439),.UNSPECIFIED.,.F.,.F.,(4,2,2,2,2,2,2,2,2,2,2,2,2,4),(0.490583102538645,
0.624046753014798,0.75751040349095,0.849653931021769,0.941797458552588,
1.03394098608341,1.12608451361423,1.25954816409038,1.39301181456653,1.54288207354412,
1.6927523325217,1.78817362481344,1.83588427095931,1.88359491710518),
 .UNSPECIFIED.);
#379=B_SPLINE_CURVE_WITH_KNOTS('',3,(#64440,#64441,#64442,#64443,#64444,
#64445,#64446,#64447,#64448,#64449,#64450,#64451),.UNSPECIFIED.,.F.,.F.,
(4,2,2,2,2,4),(0.,0.0477106461458692,0.0954212922917384,0.190842584583477,
0.340712843561061,0.490583102538645),.UNSPECIFIED.);
#380=B_SPLINE_CURVE_WITH_KNOTS('',3,(#64523,#64524,#64525,#64526,#64527,
#64528),.UNSPECIFIED.,.F.,.F.,(4,2,4),(0.575736753726219,0.638728583590876,
0.701720413455533),.UNSPECIFIED.);
#381=B_SPLINE_CURVE_WITH_KNOTS('',3,(#64534,#64535,#64536,#64537,#64538,
#64539,#64540),.UNSPECIFIED.,.F.,.F.,(4,3,4),(-0.0629918298646558,0.,0.0629918298646566),
 .UNSPECIFIED.);
#382=B_SPLINE_CURVE_WITH_KNOTS('',3,(#64547,#64548,#64549,#64550,#64551,
#64552,#64553,#64554,#64555,#64556,#64557,#64558,#64559,#64560,#64561,#64562,
#64563,#64564),.UNSPECIFIED.,.F.,.F.,(4,2,2,2,2,2,2,2,4),(0.,0.0151927838523538,
0.0303855677047076,0.0455818431537581,0.0607781186028086,0.0759788205112384,
0.0911795224196683,0.106372746681134,0.1215659709426),.UNSPECIFIED.);
#383=B_SPLINE_CURVE_WITH_KNOTS('',3,(#64575,#64576,#64577,#64578,#64579,
#64580,#64581,#64582,#64583,#64584,#64585,#64586,#64587,#64588,#64589,#64590,
#64591,#64592),.UNSPECIFIED.,.F.,.F.,(4,2,2,2,2,2,2,2,4),(0.316549052084077,
0.395686269484847,0.474823486885617,0.553960795526886,0.633098104168155,
0.712235412809424,0.791372721450692,0.870509938851462,0.949647156252232),
 .UNSPECIFIED.);
#384=B_SPLINE_CURVE_WITH_KNOTS('',3,(#64594,#64595,#64596,#64597,#64598,
#64599,#64600,#64601,#64602,#64603,#64604,#64605,#64606,#64607,#64608,#64609,
#64610,#64611,#64612,#64613,#64614,#64615,#64616,#64617,#64618,#64619,#64620,
#64621,#64622,#64623,#64624,#64625,#64626,#64627,#64628,#64629,#64630,#64631,
#64632,#64633,#64634,#64635,#64636,#64637,#64638,#64639,#64640,#64641,#64642,
#64643,#64644,#64645,#64646,#64647,#64648,#64649,#64650,#64651,#64652,#64653,
#64654),.UNSPECIFIED.,.F.,.F.,(4,3,3,3,3,3,3,3,3,3,3,3,3,3,3,3,3,3,3,3,
4),(0.,0.0530381009639862,0.106881832368641,0.160741065532074,0.214029097090197,
0.25,0.302729149752815,0.356241665072322,0.409762788184605,0.462708186762728,
0.5,0.552255845605983,0.60528221172878,0.6583187251977,0.710788396881531,
0.75,0.802421738286104,0.855626872469095,0.908846463732818,0.961502691977757,
1.),.UNSPECIFIED.);
#385=B_SPLINE_CURVE_WITH_KNOTS('',3,(#64655,#64656,#64657,#64658,#64659,
#64660,#64661,#64662,#64663,#64664),.UNSPECIFIED.,.F.,.F.,(4,2,2,2,4),(0.949647156252232,
1.028784373653,1.10792159105377,1.18705889969504,1.26619620833631),
 .UNSPECIFIED.);
#386=B_SPLINE_CURVE_WITH_KNOTS('',3,(#64719,#64720,#64721,#64722,#64723,
#64724,#64725,#64726,#64727,#64728,#64729,#64730,#64731,#64732,#64733,#64734),
 .UNSPECIFIED.,.F.,.F.,(4,2,2,2,2,2,2,4),(-0.779703847201594,-0.757646703299412,
-0.7035492015768,-0.649451699854188,-0.595298023055894,-0.5411443462576,
-0.487035463795603,-0.432926581333605),.UNSPECIFIED.);
#387=B_SPLINE_CURVE_WITH_KNOTS('',3,(#64957,#64958,#64959,#64960,#64961,
#64962,#64963,#64964,#64965,#64966,#64967,#64968,#64969,#64970,#64971,#64972),
 .UNSPECIFIED.,.F.,.F.,(4,2,2,2,2,2,2,4),(0.432932407296797,0.487041759940904,
0.541151112585012,0.595306935250484,0.649462757915956,0.703560301016107,
0.757657844116259,0.779715370662846),.UNSPECIFIED.);
#388=B_SPLINE_CURVE_WITH_KNOTS('',3,(#65004,#65005,#65006,#65007,#65008,
#65009,#65010,#65011,#65012,#65013,#65014,#65015,#65016,#65017,#65018,#65019,
#65020,#65021),.UNSPECIFIED.,.F.,.F.,(4,2,2,2,2,2,2,2,4),(0.121566783856533,
0.136760015420318,0.151953246984103,0.167154235901664,0.182355224819225,
0.19755162162294,0.212748018426654,0.22794079306986,0.243133567713066),
 .UNSPECIFIED.);
#389=B_SPLINE_CURVE_WITH_KNOTS('',3,(#65265,#65266,#65267,#65268,#65269,
#65270,#65271,#65272,#65273,#65274,#65275,#65276,#65277,#65278,#65279,#65280,
#65281,#65282),.UNSPECIFIED.,.F.,.F.,(4,2,2,2,2,2,2,2,4),(0.567634871261072,
0.624046753013484,0.757510403489333,0.849653931020164,0.941797458550995,
1.03394098608183,1.12608451361266,1.25954816408851,1.39301181456436),
 .UNSPECIFIED.);
#390=B_SPLINE_CURVE_WITH_KNOTS('',3,(#65283,#65284,#65285,#65286,#65287,
#65288,#65289,#65290,#65291,#65292,#65293,#65294,#65295,#65296,#65297,#65298,
#65299,#65300,#65301,#65302,#65303,#65304,#65305,#65306,#65307),
 .UNSPECIFIED.,.F.,.F.,(4,2,2,2,2,3,2,2,2,2,2,4),(1.39301181456436,1.54288207354147,
1.69275233251858,1.78817362481028,1.83588427095614,1.88359491710199,1.93130556324784,
1.97901620939369,2.0744375016854,2.22430776066251,2.37417801963962,2.45122978836306),
 .UNSPECIFIED.);
#391=B_SPLINE_CURVE_WITH_KNOTS('',3,(#65311,#65312,#65313,#65314,#65315,
#65316,#65317,#65318,#65319,#65320,#65321,#65322,#65323,#65324,#65325,#65326,
#65327,#65328,#65329,#65330,#65331,#65332,#65333,#65334,#65335,#65336,#65337,
#65338,#65339,#65340),.UNSPECIFIED.,.F.,.F.,(4,2,2,2,2,2,2,2,2,2,2,2,2,
2,4),(-3.98325608641923,-3.86919217466994,-3.49972652064847,-3.130260866627,
-2.85088285941104,-2.57150485219509,-2.36940240570498,-2.16729995921487,
-1.96519751272476,-1.76309506623465,-1.4837170590187,-1.20433905180275,
-0.834873397781281,-0.465407743759808,-0.351343832010516),.UNSPECIFIED.);
#392=B_SPLINE_CURVE_WITH_KNOTS('',3,(#65376,#65377,#65378,#65379,#65380,
#65381,#65382,#65383,#65384,#65385,#65386,#65387,#65388,#65389,#65390,#65391,
#65392,#65393,#65394,#65395,#65396,#65397,#65398,#65399,#65400,#65401,#65402,
#65403,#65404,#65405),.UNSPECIFIED.,.F.,.F.,(4,2,2,2,2,2,2,2,2,2,2,2,2,
2,4),(-3.98325608641923,-3.86919217466994,-3.49972652064847,-3.130260866627,
-2.85088285941104,-2.57150485219509,-2.36940240570498,-2.16729995921487,
-1.96519751272476,-1.76309506623465,-1.4837170590187,-1.20433905180275,
-0.834873397781281,-0.465407743759808,-0.351343832010517),.UNSPECIFIED.);
#393=B_SPLINE_CURVE_WITH_KNOTS('',3,(#65422,#65423,#65424,#65425,#65426,
#65427,#65428,#65429,#65430,#65431,#65432,#65433,#65434,#65435,#65436,#65437,
#65438,#65439,#65440,#65441,#65442,#65443,#65444,#65445,#65446,#65447,#65448,
#65449),.UNSPECIFIED.,.F.,.F.,(4,2,2,2,2,2,2,2,2,2,2,2,2,4),(0.490583102537635,
0.624046753013484,0.757510403489333,0.849653931020164,0.941797458550995,
1.03394098608183,1.12608451361266,1.25954816408851,1.39301181456436,1.54288207354147,
1.69275233251858,1.78817362481028,1.83588427095614,1.88359491710199),
 .UNSPECIFIED.);
#394=B_SPLINE_CURVE_WITH_KNOTS('',3,(#65450,#65451,#65452,#65453,#65454,
#65455,#65456,#65457,#65458,#65459,#65460,#65461),.UNSPECIFIED.,.F.,.F.,
(4,2,2,2,2,4),(0.,0.0477106461458525,0.095421292291705,0.19084258458341,
0.340712843560522,0.490583102537635),.UNSPECIFIED.);
#395=B_SPLINE_CURVE_WITH_KNOTS('',3,(#65538,#65539,#65540,#65541,#65542,
#65543,#65544,#65545,#65546,#65547,#65548,#65549,#65550,#65551,#65552,#65553,
#65554,#65555),.UNSPECIFIED.,.F.,.F.,(4,2,2,2,2,2,2,2,4),(0.,0.0151927838523538,
0.0303855677047076,0.0455818431537581,0.0607781186028085,0.0759788205112385,
0.0911795224196684,0.106372746681134,0.1215659709426),.UNSPECIFIED.);
#396=B_SPLINE_CURVE_WITH_KNOTS('',3,(#65565,#65566,#65567,#65568,#65569,
#65570,#65571,#65572,#65573,#65574,#65575,#65576,#65577,#65578,#65579,#65580,
#65581,#65582),.UNSPECIFIED.,.F.,.F.,(4,2,2,2,2,2,2,2,4),(0.316549052084077,
0.395686269484847,0.474823486885617,0.553960795526886,0.633098104168155,
0.712235412809424,0.791372721450693,0.870509938851463,0.949647156252233),
 .UNSPECIFIED.);
#397=B_SPLINE_CURVE_WITH_KNOTS('',3,(#65584,#65585,#65586,#65587,#65588,
#65589,#65590,#65591,#65592,#65593,#65594,#65595,#65596,#65597,#65598,#65599,
#65600,#65601,#65602,#65603,#65604,#65605,#65606,#65607,#65608,#65609,#65610,
#65611,#65612,#65613,#65614,#65615,#65616,#65617,#65618,#65619,#65620,#65621,
#65622,#65623,#65624,#65625,#65626,#65627,#65628,#65629,#65630,#65631,#65632,
#65633,#65634,#65635,#65636,#65637,#65638,#65639,#65640,#65641,#65642,#65643,
#65644),.UNSPECIFIED.,.F.,.F.,(4,3,3,3,3,3,3,3,3,3,3,3,3,3,3,3,3,3,3,3,
4),(0.,0.0530381007183943,0.106881831871485,0.160741064784848,0.214029096098922,
0.25,0.302729149593727,0.356241664754916,0.409762787712598,0.462708186143729,
0.5,0.552255845606725,0.605282211731377,0.658318725202785,0.710788396890028,
0.75,0.802421738286123,0.855626872467919,0.908846463729713,0.961502691971665,
1.),.UNSPECIFIED.);
#398=B_SPLINE_CURVE_WITH_KNOTS('',3,(#65645,#65646,#65647,#65648,#65649,
#65650,#65651,#65652,#65653,#65654),.UNSPECIFIED.,.F.,.F.,(4,2,2,2,4),(0.949647156252233,
1.028784373653,1.10792159105377,1.18705889969504,1.26619620833631),
 .UNSPECIFIED.);
#399=B_SPLINE_CURVE_WITH_KNOTS('',3,(#65695,#65696,#65697,#65698,#65699,
#65700,#65701,#65702,#65703,#65704,#65705,#65706,#65707,#65708,#65709,#65710),
 .UNSPECIFIED.,.F.,.F.,(4,2,2,2,2,2,2,4),(-0.779703847201593,-0.757646703299412,
-0.7035492015768,-0.649451699854188,-0.595298023055894,-0.5411443462576,
-0.487035463795603,-0.432926581333605),.UNSPECIFIED.);
#400=B_SPLINE_CURVE_WITH_KNOTS('',3,(#65933,#65934,#65935,#65936,#65937,
#65938,#65939,#65940,#65941,#65942,#65943,#65944,#65945,#65946,#65947,#65948),
 .UNSPECIFIED.,.F.,.F.,(4,2,2,2,2,2,2,4),(0.432932407296797,0.487041759940904,
0.541151112585012,0.595306935250484,0.649462757915956,0.703560301016107,
0.757657844116259,0.779715370662845),.UNSPECIFIED.);
#401=B_SPLINE_CURVE_WITH_KNOTS('',3,(#65980,#65981,#65982,#65983,#65984,
#65985,#65986,#65987,#65988,#65989,#65990,#65991,#65992,#65993,#65994,#65995,
#65996,#65997),.UNSPECIFIED.,.F.,.F.,(4,2,2,2,2,2,2,2,4),(0.121566783856533,
0.136760015420318,0.151953246984103,0.167154235901664,0.182355224819225,
0.197551621622939,0.212748018426654,0.22794079306986,0.243133567713066),
 .UNSPECIFIED.);
#402=(
BOUNDED_SURFACE()
B_SPLINE_SURFACE(2,2,((#37592,#37593,#37594,#37595,#37596,#37597,#37598,
#37599,#37600),(#37601,#37602,#37603,#37604,#37605,#37606,#37607,#37608,
#37609),(#37610,#37611,#37612,#37613,#37614,#37615,#37616,#37617,#37618)),
 .UNSPECIFIED.,.F.,.T.,.F.)
B_SPLINE_SURFACE_WITH_KNOTS((3,3),(3,2,2,2,3),(0.,1.43998883071719),(-3.14159265358979,
-1.5707963267949,0.,1.5707963267949,3.14159265358979),.UNSPECIFIED.)
GEOMETRIC_REPRESENTATION_ITEM()
RATIONAL_B_SPLINE_SURFACE(((1.,0.707106781186548,1.,0.707106781186548,1.,
0.707106781186548,1.,0.707106781186548,1.),(0.751809411556116,0.531609533071198,
0.751809411556116,0.531609533071198,0.751809411556116,0.531609533071198,
0.751809411556116,0.531609533071198,0.751809411556116),(1.,0.707106781186548,
1.,0.707106781186548,1.,0.707106781186548,1.,0.707106781186548,1.)))
REPRESENTATION_ITEM('')
SURFACE()
);
#403=(
BOUNDED_SURFACE()
B_SPLINE_SURFACE(2,2,((#39525,#39526,#39527,#39528,#39529,#39530,#39531,
#39532,#39533),(#39534,#39535,#39536,#39537,#39538,#39539,#39540,#39541,
#39542),(#39543,#39544,#39545,#39546,#39547,#39548,#39549,#39550,#39551)),
 .UNSPECIFIED.,.F.,.T.,.F.)
B_SPLINE_SURFACE_WITH_KNOTS((3,3),(3,2,2,2,3),(-0.371257902576148,0.541962924803503),
(-3.14159265358979,-1.5707963267949,0.,1.5707963267949,3.14159265358979),
 .UNSPECIFIED.)
GEOMETRIC_REPRESENTATION_ITEM()
RATIONAL_B_SPLINE_SURFACE(((1.,0.707106781186548,1.,0.707106781186548,1.,
0.707106781186548,1.,0.707106781186548,1.),(0.897552147568833,0.634665210014471,
0.897552147568833,0.634665210014471,0.897552147568833,0.634665210014471,
0.897552147568833,0.634665210014471,0.897552147568833),(1.,0.707106781186548,
1.,0.707106781186548,1.,0.707106781186548,1.,0.707106781186548,1.)))
REPRESENTATION_ITEM('')
SURFACE()
);
#404=(
BOUNDED_SURFACE()
B_SPLINE_SURFACE(3,3,((#41245,#41246,#41247,#41248,#41249,#41250,#41251,
#41252,#41253,#41254),(#41255,#41256,#41257,#41258,#41259,#41260,#41261,
#41262,#41263,#41264),(#41265,#41266,#41267,#41268,#41269,#41270,#41271,
#41272,#41273,#41274),(#41275,#41276,#41277,#41278,#41279,#41280,#41281,
#41282,#41283,#41284)),.UNSPECIFIED.,.F.,.F.,.F.)
B_SPLINE_SURFACE_WITH_KNOTS((4,4),(4,1,1,1,1,1,1,4),(0.0528476000136677,
0.947690598086684),(0.244373136783768,0.2805071298931,0.3579201174355,0.444129632276,
0.5371346267334,0.6323291307028,0.7265386296373,0.765696187608126),
 .UNSPECIFIED.)
GEOMETRIC_REPRESENTATION_ITEM()
RATIONAL_B_SPLINE_SURFACE(((1.20375116505837,1.20375116505837,1.20375116505837,
1.20375116505837,1.20375116505837,1.20375116505837,1.20375116505837,1.20375116505837,
1.20375116505837,1.20375116505837),(0.93191945338362,0.93191945338362,0.93191945338362,
0.93191945338362,0.93191945338362,0.93191945338362,0.93191945338362,0.93191945338362,
0.93191945338362,0.93191945338362),(0.932083043370885,0.932083043370885,
0.932083043370885,0.932083043370885,0.932083043370885,0.932083043370885,
0.932083043370885,0.932083043370885,0.932083043370885,0.932083043370885),
(1.20424193502017,1.20424193502017,1.20424193502017,1.20424193502017,1.20424193502017,
1.20424193502017,1.20424193502017,1.20424193502017,1.20424193502017,1.20424193502017)))
REPRESENTATION_ITEM('')
SURFACE()
);
#405=(
BOUNDED_SURFACE()
B_SPLINE_SURFACE(3,3,((#41381,#41382,#41383,#41384,#41385,#41386,#41387,
#41388,#41389,#41390,#41391),(#41392,#41393,#41394,#41395,#41396,#41397,
#41398,#41399,#41400,#41401,#41402),(#41403,#41404,#41405,#41406,#41407,
#41408,#41409,#41410,#41411,#41412,#41413),(#41414,#41415,#41416,#41417,
#41418,#41419,#41420,#41421,#41422,#41423,#41424)),.UNSPECIFIED.,.F.,.F.,
 .F.)
B_SPLINE_SURFACE_WITH_KNOTS((4,4),(4,1,1,1,1,1,1,1,4),(0.0434902459051769,
0.938286205395966),(-0.009351371223931,0.,0.1428542653358,0.2856978653279,
0.4287777392072,0.5720428464823,0.7151350525691,0.8578442953538,0.9437353734563),
 .UNSPECIFIED.)
GEOMETRIC_REPRESENTATION_ITEM()
RATIONAL_B_SPLINE_SURFACE(((1.1284425403519,1.1284425403519,1.1284425403519,
1.1284425403519,1.1284425403519,1.1284425403519,1.1284425403519,1.1284425403519,
1.1284425403519,1.1284425403519,1.1284425403519),(0.960604043871938,0.960604043871938,
0.960604043871938,0.960604043871938,0.960604043871938,0.960604043871938,
0.960604043871938,0.960604043871938,0.960604043871938,0.960604043871938,
0.960604043871938),(0.957254046432989,0.957254046432989,0.957254046432989,
0.957254046432989,0.957254046432989,0.957254046432989,0.957254046432989,
0.957254046432989,0.957254046432989,0.957254046432989,0.957254046432989),
(1.11839254803506,1.11839254803506,1.11839254803506,1.11839254803506,1.11839254803506,
1.11839254803506,1.11839254803506,1.11839254803506,1.11839254803506,1.11839254803506,
1.11839254803506)))
REPRESENTATION_ITEM('')
SURFACE()
);
#406=(
BOUNDED_SURFACE()
B_SPLINE_SURFACE(3,3,((#41574,#41575,#41576,#41577,#41578,#41579),(#41580,
#41581,#41582,#41583,#41584,#41585),(#41586,#41587,#41588,#41589,#41590,
#41591),(#41592,#41593,#41594,#41595,#41596,#41597)),.UNSPECIFIED.,.F.,
 .F.,.F.)
B_SPLINE_SURFACE_WITH_KNOTS((4,4),(4,1,1,4),(0.0606720802216265,0.938680242176544),
(-1.E-5,0.,0.333611620483,0.663356363542809),.UNSPECIFIED.)
GEOMETRIC_REPRESENTATION_ITEM()
RATIONAL_B_SPLINE_SURFACE(((1.17463054346692,1.17463054346692,1.17463054346692,
1.17463054346692,1.17463054346692,1.17463054346692),(0.941961451143934,
0.941961451143934,0.941961451143934,0.941961451143934,0.941961451143934,
0.941961451143934),(0.941789945358675,0.941789945358675,0.941789945358675,
0.941789945358675,0.941789945358675,0.941789945358675),(1.17411602611115,
1.17411602611115,1.17411602611115,1.17411602611115,1.17411602611115,1.17411602611115)))
REPRESENTATION_ITEM('')
SURFACE()
);
#407=(
BOUNDED_SURFACE()
B_SPLINE_SURFACE(3,3,((#41607,#41608,#41609,#41610,#41611,#41612,#41613,
#41614,#41615,#41616,#41617,#41618,#41619,#41620,#41621,#41622),(#41623,
#41624,#41625,#41626,#41627,#41628,#41629,#41630,#41631,#41632,#41633,#41634,
#41635,#41636,#41637,#41638),(#41639,#41640,#41641,#41642,#41643,#41644,
#41645,#41646,#41647,#41648,#41649,#41650,#41651,#41652,#41653,#41654),
(#41655,#41656,#41657,#41658,#41659,#41660,#41661,#41662,#41663,#41664,
#41665,#41666,#41667,#41668,#41669,#41670)),.UNSPECIFIED.,.F.,.F.,.F.)
B_SPLINE_SURFACE_WITH_KNOTS((4,4),(4,1,1,1,1,1,1,1,1,1,1,1,1,4),(0.0593643638306098,
0.933020867605329),(-0.009395290949116,0.,0.07535321742101,0.1579192703631,
0.2496876536101,0.3528405416605,0.4595218951032,0.5578812194224,0.6478328330201,
0.7283139538965,0.8001426333254,0.8679421244813,0.9343337877222,0.9520744430181),
 .UNSPECIFIED.)
GEOMETRIC_REPRESENTATION_ITEM()
RATIONAL_B_SPLINE_SURFACE(((1.07784072066994,1.07784072066994,1.07784072066994,
1.07784072066994,1.07784072066994,1.07784072066994,1.07784072066994,1.07784072066994,
1.07784072066994,1.07784072066994,1.07784072066994,1.07784072066994,1.07784072066994,
1.07784072066994,1.07784072066994,1.07784072066994),(0.97494988708073,0.97494988708073,
0.97494988708073,0.97494988708073,0.97494988708073,0.97494988708073,0.97494988708073,
0.97494988708073,0.97494988708073,0.97494988708073,0.97494988708073,0.97494988708073,
0.97494988708073,0.97494988708073,0.97494988708073,0.97494988708073),(0.974060842004898,
0.974060842004898,0.974060842004898,0.974060842004898,0.974060842004898,
0.974060842004898,0.974060842004898,0.974060842004898,0.974060842004898,
0.974060842004898,0.974060842004898,0.974060842004898,0.974060842004898,
0.974060842004898,0.974060842004898,0.974060842004898),(1.07517358544245,
1.07517358544245,1.07517358544245,1.07517358544245,1.07517358544245,1.07517358544245,
1.07517358544245,1.07517358544245,1.07517358544245,1.07517358544245,1.07517358544245,
1.07517358544245,1.07517358544245,1.07517358544245,1.07517358544245,1.07517358544245)))
REPRESENTATION_ITEM('')
SURFACE()
);
#408=(
BOUNDED_SURFACE()
B_SPLINE_SURFACE(3,3,((#42137,#42138,#42139,#42140,#42141,#42142,#42143,
#42144,#42145,#42146,#42147),(#42148,#42149,#42150,#42151,#42152,#42153,
#42154,#42155,#42156,#42157,#42158),(#42159,#42160,#42161,#42162,#42163,
#42164,#42165,#42166,#42167,#42168,#42169),(#42170,#42171,#42172,#42173,
#42174,#42175,#42176,#42177,#42178,#42179,#42180)),.UNSPECIFIED.,.F.,.F.,
 .F.)
B_SPLINE_SURFACE_WITH_KNOTS((4,4),(4,1,1,1,1,1,1,1,4),(0.0575625808515044,
0.953111018999273),(0.2692265737876,0.2759902041141,0.3429705801967,0.4189932324171,
0.4999148778522,0.5808546987381,0.6569197472851,0.7239409538869,0.730783171096),
 .UNSPECIFIED.)
GEOMETRIC_REPRESENTATION_ITEM()
RATIONAL_B_SPLINE_SURFACE(((1.19946799478327,1.19946799478327,1.19946799478327,
1.19946799478327,1.19946799478327,1.19946799478327,1.19946799478327,1.19946799478327,
1.19946799478327,1.19946799478327,1.19946799478327),(0.930302619135532,
0.930302619135532,0.930302619135532,0.930302619135532,0.930302619135532,
0.930302619135532,0.930302619135532,0.930302619135532,0.930302619135532,
0.930302619135532,0.930302619135532),(0.933549364764414,0.933549364764414,
0.933549364764414,0.933549364764414,0.933549364764414,0.933549364764414,
0.933549364764414,0.933549364764414,0.933549364764414,0.933549364764414,
0.933549364764414),(1.20920823166992,1.20920823166992,1.20920823166992,
1.20920823166992,1.20920823166992,1.20920823166992,1.20920823166992,1.20920823166992,
1.20920823166992,1.20920823166992,1.20920823166992)))
REPRESENTATION_ITEM('')
SURFACE()
);
#409=(
BOUNDED_SURFACE()
B_SPLINE_SURFACE(3,3,((#42337,#42338,#42339,#42340,#42341,#42342,#42343,
#42344,#42345,#42346),(#42347,#42348,#42349,#42350,#42351,#42352,#42353,
#42354,#42355,#42356),(#42357,#42358,#42359,#42360,#42361,#42362,#42363,
#42364,#42365,#42366),(#42367,#42368,#42369,#42370,#42371,#42372,#42373,
#42374,#42375,#42376)),.UNSPECIFIED.,.F.,.F.,.F.)
B_SPLINE_SURFACE_WITH_KNOTS((4,4),(4,1,1,1,1,1,1,4),(0.0524700928528923,
0.946598976508213),(0.233280457741109,0.275500869742,0.3703985451353,0.466098394046,
0.5590144004915,0.6447566117018,0.7216147879488,0.755011631638526),
 .UNSPECIFIED.)
GEOMETRIC_REPRESENTATION_ITEM()
RATIONAL_B_SPLINE_SURFACE(((1.20409350814067,1.20409350814067,1.20409350814067,
1.20409350814067,1.20409350814067,1.20409350814067,1.20409350814067,1.20409350814067,
1.20409350814067,1.20409350814067),(0.932251861089728,0.932251861089728,
0.932251861089728,0.932251861089728,0.932251861089728,0.932251861089728,
0.932251861089728,0.932251861089728,0.932251861089728,0.932251861089728),
(0.931969124993072,0.931969124993072,0.931969124993072,0.931969124993072,
0.931969124993072,0.931969124993072,0.931969124993072,0.931969124993072,
0.931969124993072,0.931969124993072),(1.2032452998507,1.2032452998507,1.2032452998507,
1.2032452998507,1.2032452998507,1.2032452998507,1.2032452998507,1.2032452998507,
1.2032452998507,1.2032452998507)))
REPRESENTATION_ITEM('')
SURFACE()
);
#410=(
BOUNDED_SURFACE()
B_SPLINE_SURFACE(3,3,((#42496,#42497,#42498,#42499,#42500,#42501,#42502,
#42503,#42504,#42505),(#42506,#42507,#42508,#42509,#42510,#42511,#42512,
#42513,#42514,#42515),(#42516,#42517,#42518,#42519,#42520,#42521,#42522,
#42523,#42524,#42525),(#42526,#42527,#42528,#42529,#42530,#42531,#42532,
#42533,#42534,#42535)),.UNSPECIFIED.,.F.,.F.,.F.)
B_SPLINE_SURFACE_WITH_KNOTS((4,4),(4,1,1,1,1,1,1,4),(0.0418821802266755,
0.963270218260783),(0.03308221537298,0.1426814328896,0.2856167511242,0.4287842354877,
0.5720769404683,0.7151870379729,0.857915162902,0.9460833465879),
 .UNSPECIFIED.)
GEOMETRIC_REPRESENTATION_ITEM()
RATIONAL_B_SPLINE_SURFACE(((1.13002895600752,1.13002895600752,1.13002895600752,
1.13002895600752,1.13002895600752,1.13002895600752,1.13002895600752,1.13002895600752,
1.13002895600752,1.13002895600752),(0.955682067510927,0.955682067510927,
0.955682067510927,0.955682067510927,0.955682067510927,0.955682067510927,
0.955682067510927,0.955682067510927,0.955682067510927,0.955682067510927),
(0.956662497223339,0.956662497223339,0.956662497223339,0.956662497223339,
0.956662497223339,0.956662497223339,0.956662497223339,0.956662497223339,
0.956662497223339,0.956662497223339),(1.13297024514475,1.13297024514475,
1.13297024514475,1.13297024514475,1.13297024514475,1.13297024514475,1.13297024514475,
1.13297024514475,1.13297024514475,1.13297024514475)))
REPRESENTATION_ITEM('')
SURFACE()
);
#411=(
BOUNDED_SURFACE()
B_SPLINE_SURFACE(3,3,((#42631,#42632,#42633,#42634,#42635,#42636,#42637,
#42638,#42639),(#42640,#42641,#42642,#42643,#42644,#42645,#42646,#42647,
#42648),(#42649,#42650,#42651,#42652,#42653,#42654,#42655,#42656,#42657),
(#42658,#42659,#42660,#42661,#42662,#42663,#42664,#42665,#42666)),
 .UNSPECIFIED.,.F.,.F.,.F.)
B_SPLINE_SURFACE_WITH_KNOTS((4,4),(4,1,1,1,1,1,4),(0.0492017316995449,0.946591168401197),
(0.241730229047189,0.3218312100746,0.4122894827558,0.509878641653,0.6104690130364,
0.7106140327391,0.769990672175726),.UNSPECIFIED.)
GEOMETRIC_REPRESENTATION_ITEM()
RATIONAL_B_SPLINE_SURFACE(((1.20708757459828,1.20708757459828,1.20708757459828,
1.20708757459828,1.20708757459828,1.20708757459828,1.20708757459828,1.20708757459828,
1.20708757459828),(0.93225924600194,0.93225924600194,0.93225924600194,0.93225924600194,
0.93225924600194,0.93225924600194,0.93225924600194,0.93225924600194,0.93225924600194),
(0.930976820674631,0.930976820674631,0.930976820674631,0.930976820674631,
0.930976820674631,0.930976820674631,0.930976820674631,0.930976820674631,
0.930976820674631),(1.20324029861636,1.20324029861636,1.20324029861636,
1.20324029861636,1.20324029861636,1.20324029861636,1.20324029861636,1.20324029861636,
1.20324029861636)))
REPRESENTATION_ITEM('')
SURFACE()
);
#412=(
BOUNDED_SURFACE()
B_SPLINE_SURFACE(3,3,((#42817,#42818,#42819,#42820,#42821,#42822,#42823,
#42824,#42825,#42826),(#42827,#42828,#42829,#42830,#42831,#42832,#42833,
#42834,#42835,#42836),(#42837,#42838,#42839,#42840,#42841,#42842,#42843,
#42844,#42845,#42846),(#42847,#42848,#42849,#42850,#42851,#42852,#42853,
#42854,#42855,#42856)),.UNSPECIFIED.,.F.,.F.,.F.)
B_SPLINE_SURFACE_WITH_KNOTS((4,4),(4,1,1,1,1,1,1,4),(0.0418840519216512,
0.963268772425882),(0.05391635149789,0.1420848326441,0.2848129595133,0.427923059503,
0.5712157657557,0.7143832503701,0.8573185672175,0.9669169090855),
 .UNSPECIFIED.)
GEOMETRIC_REPRESENTATION_ITEM()
RATIONAL_B_SPLINE_SURFACE(((1.13002789794623,1.13002789794623,1.13002789794623,
1.13002789794623,1.13002789794623,1.13002789794623,1.13002789794623,1.13002789794623,
1.13002789794623,1.13002789794623),(0.955682343566337,0.955682343566337,
0.955682343566337,0.955682343566337,0.955682343566337,0.955682343566337,
0.955682343566337,0.955682343566337,0.955682343566337,0.955682343566337),
(0.956662850817025,0.956662850817025,0.956662850817025,0.956662850817025,
0.956662850817025,0.956662850817025,0.956662850817025,0.956662850817025,
0.956662850817025,0.956662850817025),(1.13296941969829,1.13296941969829,
1.13296941969829,1.13296941969829,1.13296941969829,1.13296941969829,1.13296941969829,
1.13296941969829,1.13296941969829,1.13296941969829)))
REPRESENTATION_ITEM('')
SURFACE()
);
#413=(
BOUNDED_SURFACE()
B_SPLINE_SURFACE(3,3,((#43010,#43011,#43012,#43013,#43014,#43015),(#43016,
#43017,#43018,#43019,#43020,#43021),(#43022,#43023,#43024,#43025,#43026,
#43027),(#43028,#43029,#43030,#43031,#43032,#43033)),.UNSPECIFIED.,.F.,
 .F.,.F.)
B_SPLINE_SURFACE_WITH_KNOTS((4,4),(4,1,1,4),(0.0606070590319605,0.939489995881052),
(0.199119631240235,0.3331969354622,0.6668030645378,0.800880373959484),
 .UNSPECIFIED.)
GEOMETRIC_REPRESENTATION_ITEM()
RATIONAL_B_SPLINE_SURFACE(((1.17469014875841,1.17469014875841,1.17469014875841,
1.17469014875841,1.17469014875841,1.17469014875841),(0.94174422623015,0.94174422623015,
0.94174422623015,0.94174422623015,0.94174422623015,0.94174422623015),(0.941769953255028,
0.941769953255028,0.941769953255028,0.941769953255028,0.941769953255028,
0.941769953255028),(1.17476732983304,1.17476732983304,1.17476732983304,
1.17476732983304,1.17476732983304,1.17476732983304)))
REPRESENTATION_ITEM('')
SURFACE()
);
#414=(
BOUNDED_SURFACE()
B_SPLINE_SURFACE(3,3,((#43270,#43271,#43272,#43273,#43274,#43275,#43276,
#43277,#43278,#43279,#43280,#43281,#43282,#43283,#43284,#43285,#43286,#43287,
#43288,#43289),(#43290,#43291,#43292,#43293,#43294,#43295,#43296,#43297,
#43298,#43299,#43300,#43301,#43302,#43303,#43304,#43305,#43306,#43307,#43308,
#43309),(#43310,#43311,#43312,#43313,#43314,#43315,#43316,#43317,#43318,
#43319,#43320,#43321,#43322,#43323,#43324,#43325,#43326,#43327,#43328,#43329),
(#43330,#43331,#43332,#43333,#43334,#43335,#43336,#43337,#43338,#43339,
#43340,#43341,#43342,#43343,#43344,#43345,#43346,#43347,#43348,#43349)),
 .UNSPECIFIED.,.F.,.F.,.F.)
B_SPLINE_SURFACE_WITH_KNOTS((4,4),(4,1,1,1,1,1,1,1,1,1,1,1,1,1,1,1,1,4),
(0.0633076807246293,0.940122691260961),(-0.009153831274742,0.,0.07546678292497,
0.1557183846407,0.2404004052355,0.3291524428378,0.4125156378631,0.4856754559561,
0.5506573173948,0.6094478462087,0.663816257157,0.7128070375475,0.7565080779544,
0.796844405971,0.8357673160271,0.8748875859849,0.9149298599826,0.9275319405944),
 .UNSPECIFIED.)
GEOMETRIC_REPRESENTATION_ITEM()
RATIONAL_B_SPLINE_SURFACE(((1.07645082325527,1.07645082325527,1.07645082325527,
1.07645082325527,1.07645082325527,1.07645082325527,1.07645082325527,1.07645082325527,
1.07645082325527,1.07645082325527,1.07645082325527,1.07645082325527,1.07645082325527,
1.07645082325527,1.07645082325527,1.07645082325527,1.07645082325527,1.07645082325527,
1.07645082325527,1.07645082325527),(0.974116026818099,0.974116026818099,
0.974116026818099,0.974116026818099,0.974116026818099,0.974116026818099,
0.974116026818099,0.974116026818099,0.974116026818099,0.974116026818099,
0.974116026818099,0.974116026818099,0.974116026818099,0.974116026818099,
0.974116026818099,0.974116026818099,0.974116026818099,0.974116026818099,
0.974116026818099,0.974116026818099),(0.97451796475398,0.97451796475398,
0.97451796475398,0.97451796475398,0.97451796475398,0.97451796475398,0.97451796475398,
0.97451796475398,0.97451796475398,0.97451796475398,0.97451796475398,0.97451796475398,
0.97451796475398,0.97451796475398,0.97451796475398,0.97451796475398,0.97451796475398,
0.97451796475398,0.97451796475398,0.97451796475398),(1.07765663706292,1.07765663706292,
1.07765663706292,1.07765663706292,1.07765663706292,1.07765663706292,1.07765663706292,
1.07765663706292,1.07765663706292,1.07765663706292,1.07765663706292,1.07765663706292,
1.07765663706292,1.07765663706292,1.07765663706292,1.07765663706292,1.07765663706292,
1.07765663706292,1.07765663706292,1.07765663706292)))
REPRESENTATION_ITEM('')
SURFACE()
);
#415=(
BOUNDED_SURFACE()
B_SPLINE_SURFACE(3,3,((#43511,#43512,#43513,#43514,#43515,#43516,#43517,
#43518,#43519,#43520),(#43521,#43522,#43523,#43524,#43525,#43526,#43527,
#43528,#43529,#43530),(#43531,#43532,#43533,#43534,#43535,#43536,#43537,
#43538,#43539,#43540),(#43541,#43542,#43543,#43544,#43545,#43546,#43547,
#43548,#43549,#43550)),.UNSPECIFIED.,.F.,.F.,.F.)
B_SPLINE_SURFACE_WITH_KNOTS((4,4),(4,1,1,1,1,1,1,4),(0.0487270144504504,
0.946595210845177),(0.230696742769469,0.2874600436204,0.3870132096883,0.4873166151045,
0.5850151613027,0.6759386432829,0.7570631359977,0.759743251677477),
 .UNSPECIFIED.)
GEOMETRIC_REPRESENTATION_ITEM()
RATIONAL_B_SPLINE_SURFACE(((1.20752815540325,1.20752815540325,1.20752815540325,
1.20752815540325,1.20752815540325,1.20752815540325,1.20752815540325,1.20752815540325,
1.20752815540325,1.20752815540325),(0.932258068988716,0.932258068988716,
0.932258068988716,0.932258068988716,0.932258068988716,0.932258068988716,
0.932258068988716,0.932258068988716,0.932258068988716,0.932258068988716),
(0.930831381054436,0.930831381054436,0.930831381054436,0.930831381054436,
0.930831381054436,0.930831381054436,0.930831381054436,0.930831381054436,
0.930831381054436,0.930831381054436),(1.20324809160041,1.20324809160041,
1.20324809160041,1.20324809160041,1.20324809160041,1.20324809160041,1.20324809160041,
1.20324809160041,1.20324809160041,1.20324809160041)))
REPRESENTATION_ITEM('')
SURFACE()
);
#416=(
BOUNDED_SURFACE()
B_SPLINE_SURFACE(3,3,((#43670,#43671,#43672,#43673,#43674,#43675,#43676,
#43677,#43678,#43679,#43680),(#43681,#43682,#43683,#43684,#43685,#43686,
#43687,#43688,#43689,#43690,#43691),(#43692,#43693,#43694,#43695,#43696,
#43697,#43698,#43699,#43700,#43701,#43702),(#43703,#43704,#43705,#43706,
#43707,#43708,#43709,#43710,#43711,#43712,#43713)),.UNSPECIFIED.,.F.,.F.,
 .F.)
B_SPLINE_SURFACE_WITH_KNOTS((4,4),(4,1,1,1,1,1,1,1,4),(0.0595203655455625,
0.937477016075647),(0.05105962744621,0.1243082719354,0.2492351900332,0.374483525782,
0.4998948479171,0.6253218237211,0.750616579156,0.8756124488067,0.9160299520784),
 .UNSPECIFIED.)
GEOMETRIC_REPRESENTATION_ITEM()
RATIONAL_B_SPLINE_SURFACE(((1.1195805667017,1.1195805667017,1.1195805667017,
1.1195805667017,1.1195805667017,1.1195805667017,1.1195805667017,1.1195805667017,
1.1195805667017,1.1195805667017,1.1195805667017),(0.960683241153594,0.960683241153594,
0.960683241153594,0.960683241153594,0.960683241153594,0.960683241153594,
0.960683241153594,0.960683241153594,0.960683241153594,0.960683241153594,
0.960683241153594),(0.960141663299918,0.960141663299918,0.960141663299918,
0.960141663299918,0.960141663299918,0.960141663299918,0.960141663299918,
0.960141663299918,0.960141663299918,0.960141663299918,0.960141663299918),
(1.11795583314067,1.11795583314067,1.11795583314067,1.11795583314067,1.11795583314067,
1.11795583314067,1.11795583314067,1.11795583314067,1.11795583314067,1.11795583314067,
1.11795583314067)))
REPRESENTATION_ITEM('')
SURFACE()
);
#417=(
BOUNDED_SURFACE()
B_SPLINE_SURFACE(3,3,((#43947,#43948,#43949,#43950,#43951,#43952,#43953,
#43954,#43955,#43956,#43957),(#43958,#43959,#43960,#43961,#43962,#43963,
#43964,#43965,#43966,#43967,#43968),(#43969,#43970,#43971,#43972,#43973,
#43974,#43975,#43976,#43977,#43978,#43979),(#43980,#43981,#43982,#43983,
#43984,#43985,#43986,#43987,#43988,#43989,#43990)),.UNSPECIFIED.,.F.,.F.,
 .F.)
B_SPLINE_SURFACE_WITH_KNOTS((4,4),(4,1,1,1,1,1,1,1,4),(0.0574729628393945,
0.952962452837741),(0.269222366519,0.2762332346986,0.3429031113093,0.4188966873867,
0.4999818942308,0.5810709354785,0.657074202193,0.7237529548095,0.7307669759034),
 .UNSPECIFIED.)
GEOMETRIC_REPRESENTATION_ITEM()
RATIONAL_B_SPLINE_SURFACE(((1.19955084132791,1.19955084132791,1.19955084132791,
1.19955084132791,1.19955084132791,1.19955084132791,1.19955084132791,1.19955084132791,
1.19955084132791,1.19955084132791,1.19955084132791),(0.930345924831433,
0.930345924831433,0.930345924831433,0.930345924831433,0.930345924831433,
0.930345924831433,0.930345924831433,0.930345924831433,0.930345924831433,
0.930345924831433,0.930345924831433),(0.933520041857134,0.933520041857134,
0.933520041857134,0.933520041857134,0.933520041857134,0.933520041857134,
0.933520041857134,0.933520041857134,0.933520041857134,0.933520041857134,
0.933520041857134),(1.20907319240501,1.20907319240501,1.20907319240501,
1.20907319240501,1.20907319240501,1.20907319240501,1.20907319240501,1.20907319240501,
1.20907319240501,1.20907319240501,1.20907319240501)))
REPRESENTATION_ITEM('')
SURFACE()
);
#418=(
BOUNDED_SURFACE()
B_SPLINE_SURFACE(3,3,((#44088,#44089,#44090,#44091,#44092,#44093,#44094,
#44095,#44096,#44097),(#44098,#44099,#44100,#44101,#44102,#44103,#44104,
#44105,#44106,#44107),(#44108,#44109,#44110,#44111,#44112,#44113,#44114,
#44115,#44116,#44117),(#44118,#44119,#44120,#44121,#44122,#44123,#44124,
#44125,#44126,#44127)),.UNSPECIFIED.,.F.,.F.,.F.)
B_SPLINE_SURFACE_WITH_KNOTS((4,4),(4,1,1,1,1,1,1,4),(0.0479830632576071,
0.946593353952545),(0.239518392653729,0.2430457985497,0.3242077675677,0.4151597485037,
0.5128629249771,0.6131453793564,0.7126591925481,0.77004587812324),
 .UNSPECIFIED.)
GEOMETRIC_REPRESENTATION_ITEM()
RATIONAL_B_SPLINE_SURFACE(((1.20821093244647,1.20821093244647,1.20821093244647,
1.20821093244647,1.20821093244647,1.20821093244647,1.20821093244647,1.20821093244647,
1.20821093244647,1.20821093244647),(0.932261852779893,0.932261852779893,
0.932261852779893,0.932261852779893,0.932261852779893,0.932261852779893,
0.932261852779893,0.932261852779893,0.932261852779893,0.932261852779893),
(0.930606347689597,0.930606347689597,0.930606347689597,0.930606347689597,
0.930606347689597,0.930606347689597,0.930606347689597,0.930606347689597,
0.930606347689597,0.930606347689597),(1.20324441717558,1.20324441717558,
1.20324441717558,1.20324441717558,1.20324441717558,1.20324441717558,1.20324441717558,
1.20324441717558,1.20324441717558,1.20324441717558)))
REPRESENTATION_ITEM('')
SURFACE()
);
#419=(
BOUNDED_SURFACE()
B_SPLINE_SURFACE(3,3,((#44278,#44279,#44280,#44281,#44282,#44283,#44284,
#44285,#44286,#44287,#44288),(#44289,#44290,#44291,#44292,#44293,#44294,
#44295,#44296,#44297,#44298,#44299),(#44300,#44301,#44302,#44303,#44304,
#44305,#44306,#44307,#44308,#44309,#44310),(#44311,#44312,#44313,#44314,
#44315,#44316,#44317,#44318,#44319,#44320,#44321)),.UNSPECIFIED.,.F.,.F.,
 .F.)
B_SPLINE_SURFACE_WITH_KNOTS((4,4),(4,1,1,1,1,1,1,1,4),(0.0434902455975137,
0.937490443114784),(-0.009351371223931,0.,0.1428542653358,0.2856978653279,
0.4287777392072,0.5720428464823,0.7151350525691,0.8578442953538,0.9437353734563),
 .UNSPECIFIED.)
GEOMETRIC_REPRESENTATION_ITEM()
RATIONAL_B_SPLINE_SURFACE(((1.1284425406159,1.1284425406159,1.1284425406159,
1.1284425406159,1.1284425406159,1.1284425406159,1.1284425406159,1.1284425406159,
1.1284425406159,1.1284425406159,1.1284425406159),(0.960753306416933,0.960753306416933,
0.960753306416933,0.960753306416933,0.960753306416933,0.960753306416933,
0.960753306416933,0.960753306416933,0.960753306416933,0.960753306416933,
0.960753306416933),(0.95726013489752,0.95726013489752,0.95726013489752,
0.95726013489752,0.95726013489752,0.95726013489752,0.95726013489752,0.95726013489752,
0.95726013489752,0.95726013489752,0.95726013489752),(1.11796302605766,1.11796302605766,
1.11796302605766,1.11796302605766,1.11796302605766,1.11796302605766,1.11796302605766,
1.11796302605766,1.11796302605766,1.11796302605766,1.11796302605766)))
REPRESENTATION_ITEM('')
SURFACE()
);
#420=(
BOUNDED_SURFACE()
B_SPLINE_SURFACE(3,3,((#44471,#44472,#44473,#44474,#44475,#44476),(#44477,
#44478,#44479,#44480,#44481,#44482),(#44483,#44484,#44485,#44486,#44487,
#44488),(#44489,#44490,#44491,#44492,#44493,#44494)),.UNSPECIFIED.,.F.,
 .F.,.F.)
B_SPLINE_SURFACE_WITH_KNOTS((4,4),(4,1,1,4),(0.0606720802291994,0.938680242177155),
(-1.E-5,0.,0.333611620483,0.663356363538714),.UNSPECIFIED.)
GEOMETRIC_REPRESENTATION_ITEM()
RATIONAL_B_SPLINE_SURFACE(((1.1746305434609,1.1746305434609,1.1746305434609,
1.1746305434609,1.1746305434609,1.1746305434609),(0.941961451143769,0.941961451143769,
0.941961451143769,0.941961451143769,0.941961451143769,0.941961451143769),
(0.941789945360679,0.941789945360679,0.941789945360679,0.941789945360679,
0.941789945360679,0.941789945360679),(1.17411602611163,1.17411602611163,
1.17411602611163,1.17411602611163,1.17411602611163,1.17411602611163)))
REPRESENTATION_ITEM('')
SURFACE()
);
#421=(
BOUNDED_SURFACE()
B_SPLINE_SURFACE(3,3,((#44504,#44505,#44506,#44507,#44508,#44509,#44510,
#44511,#44512,#44513,#44514,#44515,#44516,#44517,#44518,#44519),(#44520,
#44521,#44522,#44523,#44524,#44525,#44526,#44527,#44528,#44529,#44530,#44531,
#44532,#44533,#44534,#44535),(#44536,#44537,#44538,#44539,#44540,#44541,
#44542,#44543,#44544,#44545,#44546,#44547,#44548,#44549,#44550,#44551),
(#44552,#44553,#44554,#44555,#44556,#44557,#44558,#44559,#44560,#44561,
#44562,#44563,#44564,#44565,#44566,#44567)),.UNSPECIFIED.,.F.,.F.,.F.)
B_SPLINE_SURFACE_WITH_KNOTS((4,4),(4,1,1,1,1,1,1,1,1,1,1,1,1,4),(0.0593643652551394,
0.933020867259932),(-0.009395290949111,0.,0.07535321742145,0.157919270364,
0.2496876536115,0.3528405416624,0.4595218951051,0.5578812194241,0.6478328330216,
0.7283139538977,0.8001426333264,0.867942124482,0.9343337877226,0.9520744430181),
 .UNSPECIFIED.)
GEOMETRIC_REPRESENTATION_ITEM()
RATIONAL_B_SPLINE_SURFACE(((1.07784072016664,1.07784072016664,1.07784072016664,
1.07784072016664,1.07784072016664,1.07784072016664,1.07784072016664,1.07784072016664,
1.07784072016664,1.07784072016664,1.07784072016664,1.07784072016664,1.07784072016664,
1.07784072016664,1.07784072016664,1.07784072016664),(0.974949887118508,
0.974949887118508,0.974949887118508,0.974949887118508,0.974949887118508,
0.974949887118508,0.974949887118508,0.974949887118508,0.974949887118508,
0.974949887118508,0.974949887118508,0.974949887118508,0.974949887118508,
0.974949887118508,0.974949887118508,0.974949887118508),(0.974060842170469,
0.974060842170469,0.974060842170469,0.974060842170469,0.974060842170469,
0.974060842170469,0.974060842170469,0.974060842170469,0.974060842170469,
0.974060842170469,0.974060842170469,0.974060842170469,0.974060842170469,
0.974060842170469,0.974060842170469,0.974060842170469),(1.07517358532252,
1.07517358532252,1.07517358532252,1.07517358532252,1.07517358532252,1.07517358532252,
1.07517358532252,1.07517358532252,1.07517358532252,1.07517358532252,1.07517358532252,
1.07517358532252,1.07517358532252,1.07517358532252,1.07517358532252,1.07517358532252)))
REPRESENTATION_ITEM('')
SURFACE()
);
#422=(
BOUNDED_SURFACE()
B_SPLINE_SURFACE(3,3,((#45034,#45035,#45036,#45037,#45038,#45039,#45040,
#45041,#45042),(#45043,#45044,#45045,#45046,#45047,#45048,#45049,#45050,
#45051),(#45052,#45053,#45054,#45055,#45056,#45057,#45058,#45059,#45060),
(#45061,#45062,#45063,#45064,#45065,#45066,#45067,#45068,#45069)),
 .UNSPECIFIED.,.F.,.F.,.F.)
B_SPLINE_SURFACE_WITH_KNOTS((4,4),(4,1,1,1,1,1,4),(0.0580455558123085,0.958568124373128),
(0.2691839650007,0.3316562569637,0.4169046927584,0.4999998690309,0.5830948871324,
0.6683429718279,0.7308256938231),.UNSPECIFIED.)
GEOMETRIC_REPRESENTATION_ITEM()
RATIONAL_B_SPLINE_SURFACE(((1.19903368770339,1.19903368770339,1.19903368770339,
1.19903368770339,1.19903368770339,1.19903368770339,1.19903368770339,1.19903368770339,
1.19903368770339),(0.928667469287341,0.928667469287341,0.928667469287341,
0.928667469287341,0.928667469287341,0.928667469287341,0.928667469287341,
0.928667469287341,0.928667469287341),(0.933749189750596,0.933749189750596,
0.933749189750596,0.933749189750596,0.933749189750596,0.933749189750596,
0.933749189750596,0.933749189750596,0.933749189750596),(1.21427884909316,
1.21427884909316,1.21427884909316,1.21427884909316,1.21427884909316,1.21427884909316,
1.21427884909316,1.21427884909316,1.21427884909316)))
REPRESENTATION_ITEM('')
SURFACE()
);
#423=(
BOUNDED_SURFACE()
B_SPLINE_SURFACE(3,3,((#45154,#45155,#45156,#45157,#45158,#45159,#45160,
#45161,#45162),(#45163,#45164,#45165,#45166,#45167,#45168,#45169,#45170,
#45171),(#45172,#45173,#45174,#45175,#45176,#45177,#45178,#45179,#45180),
(#45181,#45182,#45183,#45184,#45185,#45186,#45187,#45188,#45189)),
 .UNSPECIFIED.,.F.,.F.,.F.)
B_SPLINE_SURFACE_WITH_KNOTS((4,4),(4,1,1,1,1,1,4),(0.0491576309218551,0.946591024024462),
(0.229965585781331,0.2892821336432,0.3893944751953,0.4899684739877,0.5875628745582,
0.6780458172145,0.758314174711455),.UNSPECIFIED.)
GEOMETRIC_REPRESENTATION_ITEM()
RATIONAL_B_SPLINE_SURFACE(((1.20712810422792,1.20712810422792,1.20712810422792,
1.20712810422792,1.20712810422792,1.20712810422792,1.20712810422792,1.20712810422792,
1.20712810422792),(0.932259413774452,0.932259413774452,0.932259413774453,
0.932259413774452,0.932259413774452,0.932259413774452,0.932259413774452,
0.932259413774452,0.932259413774452),(0.930963437921561,0.930963437921561,
0.930963437921561,0.930963437921561,0.930963437921561,0.930963437921561,
0.930963437921561,0.930963437921561,0.930963437921561),(1.20324017666925,
1.20324017666925,1.20324017666925,1.20324017666925,1.20324017666925,1.20324017666925,
1.20324017666925,1.20324017666925,1.20324017666925)))
REPRESENTATION_ITEM('')
SURFACE()
);
#424=(
BOUNDED_SURFACE()
B_SPLINE_SURFACE(3,3,((#45306,#45307,#45308,#45309,#45310,#45311,#45312,
#45313,#45314,#45315),(#45316,#45317,#45318,#45319,#45320,#45321,#45322,
#45323,#45324,#45325),(#45326,#45327,#45328,#45329,#45330,#45331,#45332,
#45333,#45334,#45335),(#45336,#45337,#45338,#45339,#45340,#45341,#45342,
#45343,#45344,#45345)),.UNSPECIFIED.,.F.,.F.,.F.)
B_SPLINE_SURFACE_WITH_KNOTS((4,4),(4,1,1,1,1,1,1,4),(0.0418802231131534,
0.963270149250729),(0.03308221537293,0.1426814329309,0.2856167516997,0.4287842359667,
0.5720769404573,0.7151870370047,0.8579151611867,0.9460833465934),
 .UNSPECIFIED.)
GEOMETRIC_REPRESENTATION_ITEM()
RATIONAL_B_SPLINE_SURFACE(((1.13003006699672,1.13003006699672,1.13003006699672,
1.13003006699672,1.13003006699672,1.13003006699672,1.13003006699672,1.13003006699672,
1.13003006699672,1.13003006699672),(0.95568207640514,0.95568207640514,0.95568207640514,
0.95568207640514,0.95568207640514,0.95568207640514,0.95568207640514,0.95568207640514,
0.95568207640514,0.95568207640514),(0.956662122582739,0.956662122582739,
0.956662122582739,0.956662122582739,0.956662122582739,0.956662122582739,
0.956662122582739,0.956662122582739,0.956662122582739,0.956662122582739),
(1.13297020552952,1.13297020552952,1.13297020552952,1.13297020552952,1.13297020552952,
1.13297020552952,1.13297020552952,1.13297020552952,1.13297020552952,1.13297020552952)))
REPRESENTATION_ITEM('')
SURFACE()
);
#425=(
BOUNDED_SURFACE()
B_SPLINE_SURFACE(3,3,((#45441,#45442,#45443,#45444,#45445,#45446,#45447,
#45448,#45449),(#45450,#45451,#45452,#45453,#45454,#45455,#45456,#45457,
#45458),(#45459,#45460,#45461,#45462,#45463,#45464,#45465,#45466,#45467),
(#45468,#45469,#45470,#45471,#45472,#45473,#45474,#45475,#45476)),
 .UNSPECIFIED.,.F.,.F.,.F.)
B_SPLINE_SURFACE_WITH_KNOTS((4,4),(4,1,1,1,1,1,4),(0.0540934813622643,0.946591460873296),
(0.245865408070653,0.3024523093122,0.4027483393081,0.5068291243807,0.6089769737371,
0.7095485234591,0.76504862578338),.UNSPECIFIED.)
GEOMETRIC_REPRESENTATION_ITEM()
RATIONAL_B_SPLINE_SURFACE(((1.20261761447037,1.20261761447037,1.20261761447037,
1.20261761447037,1.20261761447037,1.20261761447037,1.20261761447037,1.20261761447037,
1.20261761447037),(0.932253305705167,0.932253305705168,0.932253305705168,
0.932253305705168,0.932253305705168,0.932253305705168,0.932253305705168,
0.932253305705168,0.932253305705168),(0.932460954535495,0.932460954535495,
0.932460954535495,0.932460954535495,0.932460954535495,0.932460954535495,
0.932460954535495,0.932460954535495,0.932460954535495),(1.20324056096136,
1.20324056096136,1.20324056096136,1.20324056096136,1.20324056096136,1.20324056096136,
1.20324056096136,1.20324056096136,1.20324056096136)))
REPRESENTATION_ITEM('')
SURFACE()
);
#426=(
BOUNDED_SURFACE()
B_SPLINE_SURFACE(3,3,((#45633,#45634,#45635,#45636,#45637,#45638,#45639,
#45640,#45641,#45642),(#45643,#45644,#45645,#45646,#45647,#45648,#45649,
#45650,#45651,#45652),(#45653,#45654,#45655,#45656,#45657,#45658,#45659,
#45660,#45661,#45662),(#45663,#45664,#45665,#45666,#45667,#45668,#45669,
#45670,#45671,#45672)),.UNSPECIFIED.,.F.,.F.,.F.)
B_SPLINE_SURFACE_WITH_KNOTS((4,4),(4,1,1,1,1,1,1,4),(0.0418829371158205,
0.963268707799286),(0.05391635148624,0.1420848319079,0.2848129590977,0.4279230594983,
0.5712157659613,0.7143832506171,0.8573185672352,0.9669169090856),
 .UNSPECIFIED.)
GEOMETRIC_REPRESENTATION_ITEM()
RATIONAL_B_SPLINE_SURFACE(((1.1300285307818,1.1300285307818,1.1300285307818,
1.1300285307818,1.1300285307818,1.1300285307818,1.1300285307818,1.1300285307818,
1.1300285307818,1.1300285307818),(0.955682353422669,0.955682353422669,0.955682353422669,
0.955682353422669,0.955682353422669,0.955682353422669,0.955682353422669,
0.955682353422669,0.955682353422669,0.955682353422669),(0.956662637361894,
0.956662637361894,0.956662637361894,0.956662637361894,0.956662637361894,
0.956662637361894,0.956662637361894,0.956662637361894,0.956662637361894,
0.956662637361894),(1.13296938259948,1.13296938259948,1.13296938259948,
1.13296938259948,1.13296938259948,1.13296938259948,1.13296938259948,1.13296938259948,
1.13296938259948,1.13296938259948)))
REPRESENTATION_ITEM('')
SURFACE()
);
#427=(
BOUNDED_SURFACE()
B_SPLINE_SURFACE(3,3,((#45826,#45827,#45828,#45829,#45830,#45831),(#45832,
#45833,#45834,#45835,#45836,#45837),(#45838,#45839,#45840,#45841,#45842,
#45843),(#45844,#45845,#45846,#45847,#45848,#45849)),.UNSPECIFIED.,.F.,
 .F.,.F.)
B_SPLINE_SURFACE_WITH_KNOTS((4,4),(4,1,1,4),(0.0606070590317961,0.939490000441598),
(0.199119625235361,0.3331969354622,0.6668030645378,0.800880379918004),
 .UNSPECIFIED.)
GEOMETRIC_REPRESENTATION_ITEM()
RATIONAL_B_SPLINE_SURFACE(((1.17469014875854,1.17469014875854,1.17469014875854,
1.17469014875854,1.17469014875854,1.17469014875854),(0.941744225021387,
0.941744225021387,0.941744225021387,0.941744225021387,0.941744225021387,
0.941744225021387),(0.941769953255252,0.941769953255252,0.941769953255252,
0.941769953255252,0.941769953255252,0.941769953255252),(1.17476733346014,
1.17476733346014,1.17476733346014,1.17476733346014,1.17476733346014,1.17476733346014)))
REPRESENTATION_ITEM('')
SURFACE()
);
#428=(
BOUNDED_SURFACE()
B_SPLINE_SURFACE(3,3,((#46086,#46087,#46088,#46089,#46090,#46091,#46092,
#46093,#46094,#46095,#46096,#46097,#46098,#46099,#46100,#46101,#46102,#46103,
#46104,#46105),(#46106,#46107,#46108,#46109,#46110,#46111,#46112,#46113,
#46114,#46115,#46116,#46117,#46118,#46119,#46120,#46121,#46122,#46123,#46124,
#46125),(#46126,#46127,#46128,#46129,#46130,#46131,#46132,#46133,#46134,
#46135,#46136,#46137,#46138,#46139,#46140,#46141,#46142,#46143,#46144,#46145),
(#46146,#46147,#46148,#46149,#46150,#46151,#46152,#46153,#46154,#46155,
#46156,#46157,#46158,#46159,#46160,#46161,#46162,#46163,#46164,#46165)),
 .UNSPECIFIED.,.F.,.F.,.F.)
B_SPLINE_SURFACE_WITH_KNOTS((4,4),(4,1,1,1,1,1,1,1,1,1,1,1,1,1,1,1,1,4),
(0.0633076755623825,0.940122691277643),(-0.009153831274746,0.,0.07546678292519,
0.1557183846411,0.2404004052361,0.3291524428384,0.4125156378636,0.4856754559566,
0.5506573173952,0.6094478462092,0.6638162571575,0.7128070375479,0.7565080779548,
0.7968444059713,0.8357673160275,0.8748875859852,0.9149298599828,0.9275319405944),
 .UNSPECIFIED.)
GEOMETRIC_REPRESENTATION_ITEM()
RATIONAL_B_SPLINE_SURFACE(((1.07645082506276,1.07645082506276,1.07645082506276,
1.07645082506276,1.07645082506276,1.07645082506276,1.07645082506276,1.07645082506276,
1.07645082506276,1.07645082506276,1.07645082506276,1.07645082506276,1.07645082506276,
1.07645082506276,1.07645082506276,1.07645082506276,1.07645082506276,1.07645082506276,
1.07645082506276,1.07645082506276),(0.974116026811419,0.974116026811419,
0.974116026811419,0.974116026811419,0.974116026811419,0.974116026811419,
0.974116026811419,0.974116026811419,0.974116026811419,0.974116026811419,
0.974116026811419,0.974116026811419,0.974116026811419,0.974116026811419,
0.974116026811419,0.974116026811419,0.974116026811419,0.974116026811419,
0.974116026811419,0.974116026811419),(0.974517964146766,0.974517964146766,
0.974517964146766,0.974517964146766,0.974517964146766,0.974517964146766,
0.974517964146766,0.974517964146766,0.974517964146766,0.974517964146766,
0.974517964146766,0.974517964146766,0.974517964146766,0.974517964146766,
0.974517964146766,0.974517964146766,0.974517964146766,0.974517964146766,
0.974517964146766,0.974517964146766),(1.0776566370688,1.0776566370688,1.0776566370688,
1.0776566370688,1.0776566370688,1.0776566370688,1.0776566370688,1.0776566370688,
1.0776566370688,1.0776566370688,1.0776566370688,1.0776566370688,1.0776566370688,
1.0776566370688,1.0776566370688,1.0776566370688,1.0776566370688,1.0776566370688,
1.0776566370688,1.0776566370688)))
REPRESENTATION_ITEM('')
SURFACE()
);
#429=(
BOUNDED_SURFACE()
B_SPLINE_SURFACE(3,3,((#46327,#46328,#46329,#46330,#46331,#46332,#46333,
#46334,#46335),(#46336,#46337,#46338,#46339,#46340,#46341,#46342,#46343,
#46344),(#46345,#46346,#46347,#46348,#46349,#46350,#46351,#46352,#46353),
(#46354,#46355,#46356,#46357,#46358,#46359,#46360,#46361,#46362)),
 .UNSPECIFIED.,.F.,.F.,.F.)
B_SPLINE_SURFACE_WITH_KNOTS((4,4),(4,1,1,1,1,1,4),(0.0550234586932618,0.946595623648369),
(0.237043609063762,0.2885350173546,0.3884487037489,0.4899228139079,0.5932141819403,
0.693729972196,0.754343676236394),.UNSPECIFIED.)
GEOMETRIC_REPRESENTATION_ITEM()
RATIONAL_B_SPLINE_SURFACE(((1.20177749083624,1.20177749083624,1.20177749083624,
1.20177749083624,1.20177749083624,1.20177749083624,1.20177749083624,1.20177749083624,
1.20177749083624),(0.932251380814184,0.932251380814184,0.932251380814185,
0.932251380814185,0.932251380814185,0.932251380814185,0.932251380814185,
0.932251380814185,0.932251380814185),(0.932741726849128,0.932741726849128,
0.932741726849128,0.932741726849128,0.932741726849128,0.932741726849128,
0.932741726849128,0.932741726849128,0.932741726849128),(1.20324852894107,
1.20324852894107,1.20324852894107,1.20324852894107,1.20324852894107,1.20324852894107,
1.20324852894107,1.20324852894107,1.20324852894107)))
REPRESENTATION_ITEM('')
SURFACE()
);
#430=(
BOUNDED_SURFACE()
B_SPLINE_SURFACE(3,3,((#46488,#46489,#46490,#46491,#46492,#46493,#46494,
#46495,#46496,#46497,#46498),(#46499,#46500,#46501,#46502,#46503,#46504,
#46505,#46506,#46507,#46508,#46509),(#46510,#46511,#46512,#46513,#46514,
#46515,#46516,#46517,#46518,#46519,#46520),(#46521,#46522,#46523,#46524,
#46525,#46526,#46527,#46528,#46529,#46530,#46531)),.UNSPECIFIED.,.F.,.F.,
 .F.)
B_SPLINE_SURFACE_WITH_KNOTS((4,4),(4,1,1,1,1,1,1,1,4),(0.0595061205631346,
0.935560325927021),(0.05105962744621,0.1243082719354,0.2492351900332,0.374483525782,
0.4998948479171,0.6253218237211,0.750616579156,0.8756124488067,0.9160299520784),
 .UNSPECIFIED.)
GEOMETRIC_REPRESENTATION_ITEM()
RATIONAL_B_SPLINE_SURFACE(((1.11958830128056,1.11958830128056,1.11958830128056,
1.11958830128056,1.11958830128056,1.11958830128056,1.11958830128056,1.11958830128056,
1.11958830128056,1.11958830128056,1.11958830128056),(0.961030162882069,
0.961030162882069,0.961030162882069,0.961030162882069,0.961030162882069,
0.961030162882069,0.961030162882069,0.961030162882069,0.961030162882069,
0.961030162882069,0.961030162882069),(0.960142233336703,0.960142233336703,
0.960142233336703,0.960142233336703,0.960142233336703,0.960142233336703,
0.960142233336703,0.960142233336703,0.960142233336703,0.960142233336703,
0.960142233336703),(1.11692451264446,1.11692451264446,1.11692451264446,
1.11692451264446,1.11692451264446,1.11692451264446,1.11692451264446,1.11692451264446,
1.11692451264446,1.11692451264446,1.11692451264446)))
REPRESENTATION_ITEM('')
SURFACE()
);
#431=(
BOUNDED_SURFACE()
B_SPLINE_SURFACE(3,3,((#46765,#46766,#46767,#46768,#46769,#46770,#46771,
#46772,#46773),(#46774,#46775,#46776,#46777,#46778,#46779,#46780,#46781,
#46782),(#46783,#46784,#46785,#46786,#46787,#46788,#46789,#46790,#46791),
(#46792,#46793,#46794,#46795,#46796,#46797,#46798,#46799,#46800)),
 .UNSPECIFIED.,.F.,.F.,.F.)
B_SPLINE_SURFACE_WITH_KNOTS((4,4),(4,1,1,1,1,1,4),(0.055545193241446,0.960521967825338),
(0.2692083078063,0.3340264203125,0.4179413584375,0.5000270643821,0.5821139624052,
0.6660288146751,0.730780783099),.UNSPECIFIED.)
GEOMETRIC_REPRESENTATION_ITEM()
RATIONAL_B_SPLINE_SURFACE(((1.20129409867085,1.20129409867085,1.20129409867085,
1.20129409867085,1.20129409867085,1.20129409867085,1.20129409867085,1.20129409867085,
1.20129409867085),(0.928050743159333,0.928050743159333,0.928050743159333,
0.928050743159333,0.928050743159333,0.928050743159333,0.928050743159333,
0.928050743159333,0.928050743159333),(0.932989653636476,0.932989653636476,
0.932989653636476,0.932989653636476,0.932989653636476,0.932989653636476,
0.932989653636476,0.932989653636476,0.932989653636476),(1.21611083010228,
1.21611083010228,1.21611083010228,1.21611083010228,1.21611083010228,1.21611083010228,
1.21611083010228,1.21611083010228,1.21611083010228)))
REPRESENTATION_ITEM('')
SURFACE()
);
#432=(
BOUNDED_SURFACE()
B_SPLINE_SURFACE(3,3,((#46871,#46872,#46873,#46874,#46875,#46876,#46877,
#46878,#46879),(#46880,#46881,#46882,#46883,#46884,#46885,#46886,#46887,
#46888),(#46889,#46890,#46891,#46892,#46893,#46894,#46895,#46896,#46897),
(#46898,#46899,#46900,#46901,#46902,#46903,#46904,#46905,#46906)),
 .UNSPECIFIED.,.F.,.F.,.F.)
B_SPLINE_SURFACE_WITH_KNOTS((4,4),(4,1,1,1,1,1,4),(0.0527983372245638,0.946599001588779),
(0.244210271093049,0.3259550556335,0.4264563043828,0.5263661020306,0.6246508850818,
0.7212192975236,0.765147692445861),.UNSPECIFIED.)
GEOMETRIC_REPRESENTATION_ITEM()
RATIONAL_B_SPLINE_SURFACE(((1.20379704514701,1.20379704514701,1.20379704514701,
1.20379704514701,1.20379704514701,1.20379704514701,1.20379704514701,1.20379704514701,
1.20379704514701),(0.93225074659745,0.93225074659745,0.93225074659745,0.93225074659745,
0.93225074659745,0.93225074659745,0.93225074659745,0.93225074659745,0.93225074659745),
(0.932067774989629,0.932067774989629,0.932067774989629,0.932067774989629,
0.932067774989629,0.932067774989629,0.932067774989629,0.932067774989629,
0.932067774989629),(1.20324813032355,1.20324813032355,1.20324813032355,
1.20324813032355,1.20324813032355,1.20324813032355,1.20324813032355,1.20324813032355,
1.20324813032355)))
REPRESENTATION_ITEM('')
SURFACE()
);
#433=(
BOUNDED_SURFACE()
B_SPLINE_SURFACE(3,3,((#47062,#47063,#47064,#47065,#47066,#47067,#47068,
#47069,#47070,#47071,#47072),(#47073,#47074,#47075,#47076,#47077,#47078,
#47079,#47080,#47081,#47082,#47083),(#47084,#47085,#47086,#47087,#47088,
#47089,#47090,#47091,#47092,#47093,#47094),(#47095,#47096,#47097,#47098,
#47099,#47100,#47101,#47102,#47103,#47104,#47105)),.UNSPECIFIED.,.F.,.F.,
 .F.)
B_SPLINE_SURFACE_WITH_KNOTS((4,4),(4,1,1,1,1,1,1,1,4),(0.0422658727921174,
0.937259435667498),(-0.009351371223903,0.,0.1428542653358,0.2856978653279,
0.4287777392072,0.5720428464823,0.7151350525691,0.8578442953538,0.9437353734563),
 .UNSPECIFIED.)
GEOMETRIC_REPRESENTATION_ITEM()
RATIONAL_B_SPLINE_SURFACE(((1.12913243791303,1.12913243791303,1.12913243791303,
1.12913243791303,1.12913243791303,1.12913243791303,1.12913243791303,1.12913243791303,
1.12913243791303,1.12913243791303,1.12913243791303),(0.960806629223671,
0.960806629223671,0.960806629223671,0.960806629223671,0.960806629223671,
0.960806629223671,0.960806629223671,0.960806629223671,0.960806629223671,
0.960806629223671,0.960806629223671),(0.957041977642826,0.957041977642826,
0.957041977642826,0.957041977642826,0.957041977642826,0.957041977642826,
0.957041977642826,0.957041977642826,0.957041977642826,0.957041977642826,
0.957041977642826),(1.11783848317049,1.11783848317049,1.11783848317049,
1.11783848317049,1.11783848317049,1.11783848317049,1.11783848317049,1.11783848317049,
1.11783848317049,1.11783848317049,1.11783848317049)))
REPRESENTATION_ITEM('')
SURFACE()
);
#434=(
BOUNDED_SURFACE()
B_SPLINE_SURFACE(3,3,((#47255,#47256,#47257,#47258,#47259,#47260),(#47261,
#47262,#47263,#47264,#47265,#47266),(#47267,#47268,#47269,#47270,#47271,
#47272),(#47273,#47274,#47275,#47276,#47277,#47278)),.UNSPECIFIED.,.F.,
 .F.,.F.)
B_SPLINE_SURFACE_WITH_KNOTS((4,4),(4,1,1,4),(0.0606720802170434,0.938680239730501),
(-1.E-5,0.,0.333614254626,0.663356363343292),.UNSPECIFIED.)
GEOMETRIC_REPRESENTATION_ITEM()
RATIONAL_B_SPLINE_SURFACE(((1.17463054347057,1.17463054347057,1.17463054347057,
1.17463054347057,1.17463054347057,1.17463054347057),(0.941961451792129,
0.941961451792129,0.941961451792129,0.941961451792129,0.941961451792129,
0.941961451792129),(0.941789945358418,0.941789945358418,0.941789945358418,
0.941789945358418,0.941789945358418,0.941789945358418),(1.17411602416943,
1.17411602416943,1.17411602416943,1.17411602416943,1.17411602416943,1.17411602416943)))
REPRESENTATION_ITEM('')
SURFACE()
);
#435=(
BOUNDED_SURFACE()
B_SPLINE_SURFACE(3,3,((#47288,#47289,#47290,#47291,#47292,#47293,#47294,
#47295,#47296,#47297,#47298,#47299,#47300,#47301,#47302,#47303),(#47304,
#47305,#47306,#47307,#47308,#47309,#47310,#47311,#47312,#47313,#47314,#47315,
#47316,#47317,#47318,#47319),(#47320,#47321,#47322,#47323,#47324,#47325,
#47326,#47327,#47328,#47329,#47330,#47331,#47332,#47333,#47334,#47335),
(#47336,#47337,#47338,#47339,#47340,#47341,#47342,#47343,#47344,#47345,
#47346,#47347,#47348,#47349,#47350,#47351)),.UNSPECIFIED.,.F.,.F.,.F.)
B_SPLINE_SURFACE_WITH_KNOTS((4,4),(4,1,1,1,1,1,1,1,1,1,1,1,1,4),(0.0600759826757179,
0.933027467697898),(-0.009395290946096,0.,0.0753532717085,0.1579194084299,
0.2496878347785,0.3528404724376,0.4595208130976,0.5578799794626,0.6478320754114,
0.7283136662239,0.8001425287391,0.8679420769042,0.9343337648423,0.9520744430431),
 .UNSPECIFIED.)
GEOMETRIC_REPRESENTATION_ITEM()
RATIONAL_B_SPLINE_SURFACE(((1.07758950148,1.07758950148,1.07758950148,1.07758950148,
1.07758950148,1.07758950148,1.07758950148,1.07758950148,1.07758950148,1.07758950148,
1.07758950148,1.07758950148,1.07758950148,1.07758950148,1.07758950148,1.07758950148),
(0.974947730216909,0.974947730216909,0.974947730216909,0.974947730216909,
0.974947730216909,0.974947730216909,0.974947730216909,0.974947730216909,
0.974947730216909,0.974947730216909,0.974947730216909,0.974947730216909,
0.974947730216909,0.974947730216909,0.974947730216909,0.974947730216909),
(0.974143188930937,0.974143188930937,0.974143188930937,0.974143188930937,
0.974143188930937,0.974143188930937,0.974143188930937,0.974143188930937,
0.974143188930937,0.974143188930937,0.974143188930937,0.974143188930937,
0.974143188930937,0.974143188930937,0.974143188930937,0.974143188930937),
(1.07517587762208,1.07517587762208,1.07517587762208,1.07517587762208,1.07517587762208,
1.07517587762208,1.07517587762208,1.07517587762208,1.07517587762208,1.07517587762208,
1.07517587762208,1.07517587762208,1.07517587762208,1.07517587762208,1.07517587762208,
1.07517587762208)))
REPRESENTATION_ITEM('')
SURFACE()
);
#436=(
BOUNDED_SURFACE()
B_SPLINE_SURFACE(3,3,((#47818,#47819,#47820,#47821,#47822,#47823,#47824,
#47825,#47826,#47827,#47828),(#47829,#47830,#47831,#47832,#47833,#47834,
#47835,#47836,#47837,#47838,#47839),(#47840,#47841,#47842,#47843,#47844,
#47845,#47846,#47847,#47848,#47849,#47850),(#47851,#47852,#47853,#47854,
#47855,#47856,#47857,#47858,#47859,#47860,#47861)),.UNSPECIFIED.,.F.,.F.,
 .F.)
B_SPLINE_SURFACE_WITH_KNOTS((4,4),(4,1,1,1,1,1,1,1,4),(0.0572310664754211,
0.950572798231042),(0.2692300395995,0.2751075328761,0.3418387429095,0.417931198782,
0.4999456991685,0.5819697696493,0.6580841324447,0.7248361845443,0.7307799588033),
 .UNSPECIFIED.)
GEOMETRIC_REPRESENTATION_ITEM()
RATIONAL_B_SPLINE_SURFACE(((1.19976708046968,1.19976708046968,1.19976708046968,
1.19976708046968,1.19976708046968,1.19976708046968,1.19976708046968,1.19976708046968,
1.19976708046968,1.19976708046968,1.19976708046968),(0.931063691256385,
0.931063691256385,0.931063691256385,0.931063691256385,0.931063691256385,
0.931063691256385,0.931063691256385,0.931063691256385,0.931063691256385,
0.931063691256385,0.931063691256385),(0.933431658763609,0.933431658763609,
0.933431658763609,0.933431658763609,0.933431658763609,0.933431658763609,
0.933431658763609,0.933431658763609,0.933431658763609,0.933431658763609,
0.933431658763609),(1.20687098299135,1.20687098299135,1.20687098299135,
1.20687098299135,1.20687098299135,1.20687098299135,1.20687098299135,1.20687098299135,
1.20687098299135,1.20687098299135,1.20687098299135)))
REPRESENTATION_ITEM('')
SURFACE()
);
#437=(
BOUNDED_SURFACE()
B_SPLINE_SURFACE(3,3,((#48021,#48022,#48023,#48024,#48025,#48026,#48027,
#48028,#48029),(#48030,#48031,#48032,#48033,#48034,#48035,#48036,#48037,
#48038),(#48039,#48040,#48041,#48042,#48043,#48044,#48045,#48046,#48047),
(#48048,#48049,#48050,#48051,#48052,#48053,#48054,#48055,#48056)),
 .UNSPECIFIED.,.F.,.F.,.F.)
B_SPLINE_SURFACE_WITH_KNOTS((4,4),(4,1,1,1,1,1,4),(0.0524039687756051,0.946596210479273),
(0.233297759115741,0.279643029582,0.3765118146602,0.4751376597475,0.5753331138272,
0.6758913779353,0.755181913864713),.UNSPECIFIED.)
GEOMETRIC_REPRESENTATION_ITEM()
RATIONAL_B_SPLINE_SURFACE(((1.2041545053254,1.2041545053254,1.2041545053254,
1.2041545053254,1.2041545053254,1.2041545053254,1.2041545053254,1.2041545053254,
1.2041545053254),(0.932252519254702,0.932252519254703,0.932252519254703,
0.932252519254703,0.932252519254703,0.932252519254703,0.932252519254703,
0.932252519254703,0.932252519254703),(0.931948837779277,0.931948837779277,
0.931948837779277,0.931948837779277,0.931948837779277,0.931948837779277,
0.931948837779277,0.931948837779277,0.931948837779277),(1.20324346089913,
1.20324346089913,1.20324346089913,1.20324346089913,1.20324346089913,1.20324346089913,
1.20324346089913,1.20324346089913,1.20324346089913)))
REPRESENTATION_ITEM('')
SURFACE()
);
#438=(
BOUNDED_SURFACE()
B_SPLINE_SURFACE(3,3,((#48157,#48158,#48159,#48160,#48161,#48162,#48163,
#48164,#48165,#48166),(#48167,#48168,#48169,#48170,#48171,#48172,#48173,
#48174,#48175,#48176),(#48177,#48178,#48179,#48180,#48181,#48182,#48183,
#48184,#48185,#48186),(#48187,#48188,#48189,#48190,#48191,#48192,#48193,
#48194,#48195,#48196)),.UNSPECIFIED.,.F.,.F.,.F.)
B_SPLINE_SURFACE_WITH_KNOTS((4,4),(4,1,1,1,1,1,1,4),(0.0418820588917568,
0.963270218620141),(0.03308221537277,0.1426814329706,0.285616752253,0.4287842364271,
0.5720769404467,0.7151870360741,0.8579151595379,0.9460833466108),
 .UNSPECIFIED.)
GEOMETRIC_REPRESENTATION_ITEM()
RATIONAL_B_SPLINE_SURFACE(((1.13002902488611,1.13002902488611,1.13002902488611,
1.13002902488611,1.13002902488611,1.13002902488611,1.13002902488611,1.13002902488611,
1.13002902488611,1.13002902488611),(0.955682067184747,0.955682067184747,
0.955682067184747,0.955682067184747,0.955682067184747,0.955682067184747,
0.955682067184747,0.955682067184747,0.955682067184747,0.955682067184747),
(0.956662474006688,0.956662474006688,0.956662474006688,0.956662474006688,
0.956662474006688,0.956662474006688,0.956662474006688,0.956662474006688,
0.956662474006688,0.956662474006688),(1.13297024535194,1.13297024535194,
1.13297024535194,1.13297024535194,1.13297024535194,1.13297024535194,1.13297024535194,
1.13297024535194,1.13297024535194,1.13297024535194)))
REPRESENTATION_ITEM('')
SURFACE()
);
#439=(
BOUNDED_SURFACE()
B_SPLINE_SURFACE(3,3,((#48292,#48293,#48294,#48295,#48296,#48297,#48298,
#48299,#48300),(#48301,#48302,#48303,#48304,#48305,#48306,#48307,#48308,
#48309),(#48310,#48311,#48312,#48313,#48314,#48315,#48316,#48317,#48318),
(#48319,#48320,#48321,#48322,#48323,#48324,#48325,#48326,#48327)),
 .UNSPECIFIED.,.F.,.F.,.F.)
B_SPLINE_SURFACE_WITH_KNOTS((4,4),(4,1,1,1,1,1,4),(0.0550113442417672,0.946590905096635),
(0.245672692603397,0.293915687091,0.3999811782267,0.5047555052941,0.607503035598,
0.7085304952283,0.764913517676986),.UNSPECIFIED.)
GEOMETRIC_REPRESENTATION_ITEM()
RATIONAL_B_SPLINE_SURFACE(((1.20178444363563,1.20178444363563,1.20178444363563,
1.20178444363563,1.20178444363563,1.20178444363563,1.20178444363563,1.20178444363563,
1.20178444363563),(0.932254148400803,0.932254148400803,0.932254148400803,
0.932254148400803,0.932254148400803,0.932254148400803,0.932254148400803,
0.932254148400803,0.932254148400803),(0.932739390812751,0.932739390812751,
0.932739390812751,0.932739390812751,0.932739390812751,0.932739390812751,
0.932739390812751,0.932739390812751,0.932739390812751),(1.20324017087147,
1.20324017087147,1.20324017087147,1.20324017087147,1.20324017087147,1.20324017087147,
1.20324017087147,1.20324017087147,1.20324017087147)))
REPRESENTATION_ITEM('')
SURFACE()
);
#440=(
BOUNDED_SURFACE()
B_SPLINE_SURFACE(3,3,((#48486,#48487,#48488,#48489,#48490,#48491,#48492,
#48493,#48494,#48495),(#48496,#48497,#48498,#48499,#48500,#48501,#48502,
#48503,#48504,#48505),(#48506,#48507,#48508,#48509,#48510,#48511,#48512,
#48513,#48514,#48515),(#48516,#48517,#48518,#48519,#48520,#48521,#48522,
#48523,#48524,#48525)),.UNSPECIFIED.,.F.,.F.,.F.)
B_SPLINE_SURFACE_WITH_KNOTS((4,4),(4,1,1,1,1,1,1,4),(0.0418824149398342,
0.963268707201785),(0.05391635144762,0.142084832232,0.2848129592807,0.4279230595004,
0.5712157658708,0.7143832505083,0.8573185672274,0.966916909086),
 .UNSPECIFIED.)
GEOMETRIC_REPRESENTATION_ITEM()
RATIONAL_B_SPLINE_SURFACE(((1.13002882720305,1.13002882720305,1.13002882720305,
1.13002882720305,1.13002882720305,1.13002882720305,1.13002882720305,1.13002882720305,
1.13002882720305,1.13002882720305),(0.955682352424675,0.955682352424675,
0.955682352424675,0.955682352424675,0.955682352424675,0.955682352424675,
0.955682352424675,0.955682352424675,0.955682352424675,0.955682352424675),
(0.956662537442487,0.956662537442487,0.956662537442487,0.956662537442487,
0.956662537442487,0.956662537442487,0.956662537442487,0.956662537442487,
0.956662537442487,0.956662537442487),(1.13296938225648,1.13296938225648,
1.13296938225648,1.13296938225648,1.13296938225648,1.13296938225648,1.13296938225648,
1.13296938225648,1.13296938225648,1.13296938225648)))
REPRESENTATION_ITEM('')
SURFACE()
);
#441=(
BOUNDED_SURFACE()
B_SPLINE_SURFACE(3,3,((#48679,#48680,#48681,#48682,#48683,#48684),(#48685,
#48686,#48687,#48688,#48689,#48690),(#48691,#48692,#48693,#48694,#48695,
#48696),(#48697,#48698,#48699,#48700,#48701,#48702)),.UNSPECIFIED.,.F.,
 .F.,.F.)
B_SPLINE_SURFACE_WITH_KNOTS((4,4),(4,1,1,4),(0.0606070589585487,0.939489994809047),
(0.199119633361316,0.3331969354622,0.6668030645378,0.800880372533487),
 .UNSPECIFIED.)
GEOMETRIC_REPRESENTATION_ITEM()
RATIONAL_B_SPLINE_SURFACE(((1.17469014881678,1.17469014881678,1.17469014881678,
1.17469014881678,1.17469014881678,1.17469014881678),(0.941744226514278,
0.941744226514278,0.941744226514278,0.941744226514278,0.941744226514278,
0.941744226514278),(0.941769953235504,0.941769953235505,0.941769953235504,
0.941769953235504,0.941769953235504,0.941769953235504),(1.17476732898046,
1.17476732898046,1.17476732898046,1.17476732898046,1.17476732898046,1.17476732898046)))
REPRESENTATION_ITEM('')
SURFACE()
);
#442=(
BOUNDED_SURFACE()
B_SPLINE_SURFACE(3,3,((#48972,#48973,#48974,#48975,#48976,#48977,#48978,
#48979,#48980,#48981,#48982,#48983,#48984,#48985,#48986,#48987,#48988,#48989,
#48990,#48991),(#48992,#48993,#48994,#48995,#48996,#48997,#48998,#48999,
#49000,#49001,#49002,#49003,#49004,#49005,#49006,#49007,#49008,#49009,#49010,
#49011),(#49012,#49013,#49014,#49015,#49016,#49017,#49018,#49019,#49020,
#49021,#49022,#49023,#49024,#49025,#49026,#49027,#49028,#49029,#49030,#49031),
(#49032,#49033,#49034,#49035,#49036,#49037,#49038,#49039,#49040,#49041,
#49042,#49043,#49044,#49045,#49046,#49047,#49048,#49049,#49050,#49051)),
 .UNSPECIFIED.,.F.,.F.,.F.)
B_SPLINE_SURFACE_WITH_KNOTS((4,4),(4,1,1,1,1,1,1,1,1,1,1,1,1,1,1,1,1,4),
(0.0633076715126945,0.939196073757282),(-0.009153831276904,0.,0.07546659124057,
0.1557180876065,0.2404001363499,0.3291523816843,0.4125158427863,0.4856758619718,
0.550657876718,0.6094485282688,0.6638170257842,0.7128077767047,0.7565087359809,
0.7968449582087,0.83576776035,0.8748879264935,0.9149300941035,0.92753194056),
 .UNSPECIFIED.)
GEOMETRIC_REPRESENTATION_ITEM()
RATIONAL_B_SPLINE_SURFACE(((1.07645082698873,1.07645082698873,1.07645082698873,
1.07645082698873,1.07645082698873,1.07645082698873,1.07645082698873,1.07645082698873,
1.07645082698873,1.07645082698873,1.07645082698873,1.07645082698873,1.07645082698873,
1.07645082698873,1.07645082698873,1.07645082698873,1.07645082698873,1.07645082698873,
1.07645082698873,1.07645082698873),(0.974224173983562,0.974224173983562,
0.974224173983562,0.974224173983562,0.974224173983562,0.974224173983562,
0.974224173983562,0.974224173983562,0.974224173983562,0.974224173983562,
0.974224173983562,0.974224173983562,0.974224173983562,0.974224173983562,
0.974224173983562,0.974224173983562,0.974224173983562,0.974224173983562,
0.974224173983562,0.974224173983562),(0.974517228706797,0.974517228706797,
0.974517228706797,0.974517228706797,0.974517228706797,0.974517228706797,
0.974517228706797,0.974517228706797,0.974517228706797,0.974517228706797,
0.974517228706797,0.974517228706797,0.974517228706797,0.974517228706797,
0.974517228706797,0.974517228706797,0.974517228706797,0.974517228706797,
0.974517228706797,0.974517228706797),(1.07732999115843,1.07732999115843,
1.07732999115843,1.07732999115843,1.07732999115843,1.07732999115843,1.07732999115843,
1.07732999115843,1.07732999115843,1.07732999115843,1.07732999115843,1.07732999115843,
1.07732999115843,1.07732999115843,1.07732999115843,1.07732999115843,1.07732999115843,
1.07732999115843,1.07732999115843,1.07732999115843)))
REPRESENTATION_ITEM('')
SURFACE()
);
#443=(
BOUNDED_SURFACE()
B_SPLINE_SURFACE(3,3,((#49213,#49214,#49215,#49216,#49217,#49218,#49219,
#49220,#49221),(#49222,#49223,#49224,#49225,#49226,#49227,#49228,#49229,
#49230),(#49231,#49232,#49233,#49234,#49235,#49236,#49237,#49238,#49239),
(#49240,#49241,#49242,#49243,#49244,#49245,#49246,#49247,#49248)),
 .UNSPECIFIED.,.F.,.F.,.F.)
B_SPLINE_SURFACE_WITH_KNOTS((4,4),(4,1,1,1,1,1,4),(0.055506584836218,0.946593944947033),
(0.236411568203208,0.2913697515911,0.3923800891028,0.4951121067649,0.5998777813914,
0.7059484945911,0.755322160627775),.UNSPECIFIED.)
GEOMETRIC_REPRESENTATION_ITEM()
RATIONAL_B_SPLINE_SURFACE(((1.2013399063862,1.2013399063862,1.2013399063862,
1.2013399063862,1.2013399063862,1.2013399063862,1.2013399063862,1.2013399063862,
1.2013399063862),(0.93225238705743,0.93225238705743,0.93225238705743,0.93225238705743,
0.93225238705743,0.93225238705743,0.93225238705743,0.93225238705743,0.93225238705743),
(0.932888196643544,0.932888196643544,0.932888196643544,0.932888196643544,
0.932888196643544,0.932888196643544,0.932888196643544,0.932888196643544,
0.932888196643544),(1.20324733514454,1.20324733514454,1.20324733514454,
1.20324733514454,1.20324733514454,1.20324733514454,1.20324733514454,1.20324733514454,
1.20324733514454)))
REPRESENTATION_ITEM('')
SURFACE()
);
#444=(
BOUNDED_SURFACE()
B_SPLINE_SURFACE(3,3,((#49371,#49372,#49373,#49374,#49375,#49376,#49377,
#49378,#49379,#49380,#49381),(#49382,#49383,#49384,#49385,#49386,#49387,
#49388,#49389,#49390,#49391,#49392),(#49393,#49394,#49395,#49396,#49397,
#49398,#49399,#49400,#49401,#49402,#49403),(#49404,#49405,#49406,#49407,
#49408,#49409,#49410,#49411,#49412,#49413,#49414)),.UNSPECIFIED.,.F.,.F.,
 .F.)
B_SPLINE_SURFACE_WITH_KNOTS((4,4),(4,1,1,1,1,1,1,1,4),(0.0595080337692124,
0.938373838344971),(0.05105962744621,0.1243082719354,0.2492351900332,0.374483525782,
0.4998948479171,0.6253218237211,0.750616579156,0.8756124488067,0.9160299520784),
 .UNSPECIFIED.)
GEOMETRIC_REPRESENTATION_ITEM()
RATIONAL_B_SPLINE_SURFACE(((1.11958726248623,1.11958726248623,1.11958726248623,
1.11958726248623,1.11958726248623,1.11958726248623,1.11958726248623,1.11958726248623,
1.11958726248623,1.11958726248623,1.11958726248623),(0.960520940102268,
0.960520940102268,0.960520940102268,0.960520940102268,0.960520940102268,
0.960520940102268,0.960520940102268,0.960520940102268,0.960520940102268,
0.960520940102268,0.960520940102268),(0.960138500876397,0.960138500876397,
0.960138500876397,0.960138500876397,0.960138500876397,0.960138500876397,
0.960138500876397,0.960138500876397,0.960138500876397,0.960138500876397,
0.960138500876397),(1.11843994480862,1.11843994480862,1.11843994480862,
1.11843994480862,1.11843994480862,1.11843994480862,1.11843994480862,1.11843994480862,
1.11843994480862,1.11843994480862,1.11843994480862)))
REPRESENTATION_ITEM('')
SURFACE()
);
#445=(
BOUNDED_SURFACE()
B_SPLINE_SURFACE(3,3,((#49648,#49649,#49650,#49651,#49652,#49653,#49654,
#49655,#49656),(#49657,#49658,#49659,#49660,#49661,#49662,#49663,#49664,
#49665),(#49666,#49667,#49668,#49669,#49670,#49671,#49672,#49673,#49674),
(#49675,#49676,#49677,#49678,#49679,#49680,#49681,#49682,#49683)),
 .UNSPECIFIED.,.F.,.F.,.F.)
B_SPLINE_SURFACE_WITH_KNOTS((4,4),(4,1,1,1,1,1,4),(0.0580450064981613,0.95970901530257),
(0.2691730573356,0.3323186552644,0.4172250302096,0.5000005102551,0.5827761716977,
0.6676829731686,0.7308158292446),.UNSPECIFIED.)
GEOMETRIC_REPRESENTATION_ITEM()
RATIONAL_B_SPLINE_SURFACE(((1.1990364284185,1.1990364284185,1.1990364284185,
1.1990364284185,1.1990364284185,1.1990364284185,1.1990364284185,1.1990364284185,
1.1990364284185),(0.928324121230913,0.928324121230913,0.928324121230913,
0.928324121230913,0.928324121230913,0.928324121230913,0.928324121230913,
0.928324121230913,0.928324121230913),(0.933761589156609,0.933761589156609,
0.933761589156609,0.933761589156609,0.933761589156609,0.933761589156609,
0.933761589156609,0.933761589156609,0.933761589156609),(1.21534883219559,
1.21534883219559,1.21534883219559,1.21534883219559,1.21534883219559,1.21534883219559,
1.21534883219559,1.21534883219559,1.21534883219559)))
REPRESENTATION_ITEM('')
SURFACE()
);
#446=(
BOUNDED_SURFACE()
B_SPLINE_SURFACE(3,3,((#49766,#49767,#49768,#49769,#49770,#49771,#49772,
#49773,#49774,#49775),(#49776,#49777,#49778,#49779,#49780,#49781,#49782,
#49783,#49784,#49785),(#49786,#49787,#49788,#49789,#49790,#49791,#49792,
#49793,#49794,#49795),(#49796,#49797,#49798,#49799,#49800,#49801,#49802,
#49803,#49804,#49805)),.UNSPECIFIED.,.F.,.F.,.F.)
B_SPLINE_SURFACE_WITH_KNOTS((4,4),(4,1,1,1,1,1,1,4),(0.0528241875078419,
0.947906039093121),(0.244350846833031,0.2800690513799,0.3573786635911,0.443483668411,
0.5364412743718,0.6317122802247,0.7260664139081,0.765913579734812),
 .UNSPECIFIED.)
GEOMETRIC_REPRESENTATION_ITEM()
RATIONAL_B_SPLINE_SURFACE(((1.20377260436513,1.20377260436513,1.20377260436513,
1.20377260436513,1.20377260436513,1.20377260436513,1.20377260436513,1.20377260436513,
1.20377260436513,1.20377260436513),(0.931853961596766,0.931853961596766,
0.931853961596766,0.931853961596766,0.931853961596766,0.931853961596766,
0.931853961596766,0.931853961596766,0.931853961596766,0.931853961596766),
(0.932075979671873,0.932075979671873,0.932075979671873,0.932075979671873,
0.932075979671873,0.932075979671873,0.932075979671873,0.932075979671873,
0.932075979671873,0.932075979671873),(1.20443865859045,1.20443865859045,
1.20443865859045,1.20443865859045,1.20443865859045,1.20443865859045,1.20443865859045,
1.20443865859045,1.20443865859045,1.20443865859045)))
REPRESENTATION_ITEM('')
SURFACE()
);
#447=(
BOUNDED_SURFACE()
B_SPLINE_SURFACE(3,3,((#49902,#49903,#49904,#49905,#49906,#49907,#49908,
#49909,#49910,#49911,#49912),(#49913,#49914,#49915,#49916,#49917,#49918,
#49919,#49920,#49921,#49922,#49923),(#49924,#49925,#49926,#49927,#49928,
#49929,#49930,#49931,#49932,#49933,#49934),(#49935,#49936,#49937,#49938,
#49939,#49940,#49941,#49942,#49943,#49944,#49945)),.UNSPECIFIED.,.F.,.F.,
 .F.)
B_SPLINE_SURFACE_WITH_KNOTS((4,4),(4,1,1,1,1,1,1,1,4),(0.0434902476857429,
0.938303096471174),(-0.009351371213968,0.,0.1428545029,0.2856984060337,
0.4287781897902,0.5720429752755,0.7151346717899,0.857843506892,0.9437353739471),
 .UNSPECIFIED.)
GEOMETRIC_REPRESENTATION_ITEM()
RATIONAL_B_SPLINE_SURFACE(((1.12844253935412,1.12844253935412,1.12844253935412,
1.12844253935412,1.12844253935412,1.12844253935412,1.12844253935412,1.12844253935412,
1.12844253935412,1.12844253935412,1.12844253935412),(0.960600875567781,
0.960600875567781,0.960600875567781,0.960600875567781,0.960600875567781,
0.960600875567781,0.960600875567781,0.960600875567781,0.960600875567781,
0.960600875567781,0.960600875567781),(0.957253920334955,0.957253920334955,
0.957253920334955,0.957253920334955,0.957253920334955,0.957253920334955,
0.957253920334955,0.957253920334955,0.957253920334955,0.957253920334955,
0.957253920334955),(1.11840167365564,1.11840167365564,1.11840167365564,
1.11840167365564,1.11840167365564,1.11840167365564,1.11840167365564,1.11840167365564,
1.11840167365564,1.11840167365564,1.11840167365564)))
REPRESENTATION_ITEM('')
SURFACE()
);
#448=(
BOUNDED_SURFACE()
B_SPLINE_SURFACE(3,3,((#50095,#50096,#50097,#50098,#50099,#50100),(#50101,
#50102,#50103,#50104,#50105,#50106),(#50107,#50108,#50109,#50110,#50111,
#50112),(#50113,#50114,#50115,#50116,#50117,#50118)),.UNSPECIFIED.,.F.,
 .F.,.F.)
B_SPLINE_SURFACE_WITH_KNOTS((4,4),(4,1,1,4),(0.0606720801613996,0.938680242177229),
(-1.E-5,0.,0.3336142546261,0.6633563633615),.UNSPECIFIED.)
GEOMETRIC_REPRESENTATION_ITEM()
RATIONAL_B_SPLINE_SURFACE(((1.1746305435148,1.1746305435148,1.1746305435148,
1.1746305435148,1.1746305435148,1.1746305435148),(0.941961451143776,0.941961451143776,
0.941961451143776,0.941961451143776,0.941961451143776,0.941961451143776),
(0.941789945342739,0.941789945342739,0.941789945342739,0.941789945342739,
0.941789945342739,0.941789945342739),(1.17411602611169,1.17411602611169,
1.17411602611169,1.17411602611169,1.17411602611169,1.17411602611169)))
REPRESENTATION_ITEM('')
SURFACE()
);
#449=(
BOUNDED_SURFACE()
B_SPLINE_SURFACE(3,3,((#50128,#50129,#50130,#50131,#50132,#50133,#50134,
#50135,#50136,#50137,#50138,#50139,#50140,#50141,#50142,#50143),(#50144,
#50145,#50146,#50147,#50148,#50149,#50150,#50151,#50152,#50153,#50154,#50155,
#50156,#50157,#50158,#50159),(#50160,#50161,#50162,#50163,#50164,#50165,
#50166,#50167,#50168,#50169,#50170,#50171,#50172,#50173,#50174,#50175),
(#50176,#50177,#50178,#50179,#50180,#50181,#50182,#50183,#50184,#50185,
#50186,#50187,#50188,#50189,#50190,#50191)),.UNSPECIFIED.,.F.,.F.,.F.)
B_SPLINE_SURFACE_WITH_KNOTS((4,4),(4,1,1,1,1,1,1,1,1,1,1,1,1,4),(0.0600759832204326,
0.9330208779252),(-0.009395290945745,0.,0.07535327170826,0.1579194084293,
0.2496878347776,0.3528404724363,0.4595208130962,0.5578799794614,0.6478320754105,
0.7283136662232,0.8001425287387,0.867942076904,0.9343337648423,0.9520744430431),
 .UNSPECIFIED.)
GEOMETRIC_REPRESENTATION_ITEM()
RATIONAL_B_SPLINE_SURFACE(((1.07758950128785,1.07758950128785,1.07758950128785,
1.07758950128785,1.07758950128785,1.07758950128785,1.07758950128785,1.07758950128785,
1.07758950128785,1.07758950128785,1.07758950128785,1.07758950128785,1.07758950128785,
1.07758950128785,1.07758950128785,1.07758950128785),(0.974948505042402,
0.974948505042402,0.974948505042402,0.974948505042402,0.974948505042402,
0.974948505042402,0.974948505042402,0.974948505042402,0.974948505042402,
0.974948505042402,0.974948505042402,0.974948505042402,0.974948505042402,
0.974948505042402,0.974948505042402,0.974948505042402),(0.974143201146493,
0.974143201146493,0.974143201146493,0.974143201146493,0.974143201146493,
0.974143201146493,0.974143201146493,0.974143201146493,0.974143201146493,
0.974143201146493,0.974143201146493,0.974143201146493,0.974143201146493,
0.974143201146493,0.974143201146493,0.974143201146493),(1.07517358960013,
1.07517358960013,1.07517358960013,1.07517358960013,1.07517358960013,1.07517358960013,
1.07517358960013,1.07517358960013,1.07517358960013,1.07517358960013,1.07517358960013,
1.07517358960013,1.07517358960013,1.07517358960013,1.07517358960013,1.07517358960013)))
REPRESENTATION_ITEM('')
SURFACE()
);
#450=(
BOUNDED_SURFACE()
B_SPLINE_SURFACE(3,3,((#50658,#50659,#50660,#50661,#50662,#50663,#50664,
#50665,#50666,#50667,#50668),(#50669,#50670,#50671,#50672,#50673,#50674,
#50675,#50676,#50677,#50678,#50679),(#50680,#50681,#50682,#50683,#50684,
#50685,#50686,#50687,#50688,#50689,#50690),(#50691,#50692,#50693,#50694,
#50695,#50696,#50697,#50698,#50699,#50700,#50701)),.UNSPECIFIED.,.F.,.F.,
 .F.)
B_SPLINE_SURFACE_WITH_KNOTS((4,4),(4,1,1,1,1,1,1,1,4),(0.0575632716498308,
0.953112794434742),(0.2692267298686,0.2759856699154,0.3429685143453,0.4189932536889,
0.4999153618947,0.580855541603,0.656922437546,0.7239458783794,0.7307829892477),
 .UNSPECIFIED.)
GEOMETRIC_REPRESENTATION_ITEM()
RATIONAL_B_SPLINE_SURFACE(((1.19946737217014,1.19946737217014,1.19946737217014,
1.19946737217014,1.19946737217014,1.19946737217014,1.19946737217014,1.19946737217014,
1.19946737217014,1.19946737217014,1.19946737217014),(0.930302090429665,
0.930302090429665,0.930302090429665,0.930302090429665,0.930302090429665,
0.930302090429665,0.930302090429665,0.930302090429665,0.930302090429665,
0.930302090429665,0.930302090429665),(0.933549590186578,0.933549590186578,
0.933549590186578,0.933549590186578,0.933549590186578,0.933549590186578,
0.933549590186578,0.933549590186578,0.933549590186578,0.933549590186578,
0.933549590186578),(1.20920987144088,1.20920987144088,1.20920987144088,
1.20920987144088,1.20920987144088,1.20920987144088,1.20920987144088,1.20920987144088,
1.20920987144088,1.20920987144088,1.20920987144088)))
REPRESENTATION_ITEM('')
SURFACE()
);
#451=(
BOUNDED_SURFACE()
B_SPLINE_SURFACE(3,3,((#50855,#50856,#50857,#50858,#50859,#50860,#50861,
#50862,#50863,#50864),(#50865,#50866,#50867,#50868,#50869,#50870,#50871,
#50872,#50873,#50874),(#50875,#50876,#50877,#50878,#50879,#50880,#50881,
#50882,#50883,#50884),(#50885,#50886,#50887,#50888,#50889,#50890,#50891,
#50892,#50893,#50894)),.UNSPECIFIED.,.F.,.F.,.F.)
B_SPLINE_SURFACE_WITH_KNOTS((4,4),(4,1,1,1,1,1,1,4),(0.0524368674708791,
0.9465986338923),(0.233245719424266,0.2759694154114,0.371008392869,0.4667717162199,
0.5596326028965,0.6452726458233,0.7220332580943,0.755043759390866),
 .UNSPECIFIED.)
GEOMETRIC_REPRESENTATION_ITEM()
RATIONAL_B_SPLINE_SURFACE(((1.20412390665185,1.20412390665185,1.20412390665185,
1.20412390665185,1.20412390665185,1.20412390665185,1.20412390665185,1.20412390665185,
1.20412390665185,1.20412390665185),(0.932251955821422,0.932251955821422,
0.932251955821421,0.932251955821422,0.932251955821422,0.932251955821422,
0.932251955821422,0.932251955821422,0.932251955821422,0.932251955821422),
(0.931959013768214,0.931959013768214,0.931959013768214,0.931959013768214,
0.931959013768214,0.931959013768214,0.931959013768214,0.931959013768214,
0.931959013768214,0.931959013768214),(1.20324508049223,1.20324508049223,
1.20324508049223,1.20324508049223,1.20324508049223,1.20324508049223,1.20324508049223,
1.20324508049223,1.20324508049223,1.20324508049223)))
REPRESENTATION_ITEM('')
SURFACE()
);
#452=(
BOUNDED_SURFACE()
B_SPLINE_SURFACE(3,3,((#51014,#51015,#51016,#51017,#51018,#51019,#51020,
#51021,#51022,#51023),(#51024,#51025,#51026,#51027,#51028,#51029,#51030,
#51031,#51032,#51033),(#51034,#51035,#51036,#51037,#51038,#51039,#51040,
#51041,#51042,#51043),(#51044,#51045,#51046,#51047,#51048,#51049,#51050,
#51051,#51052,#51053)),.UNSPECIFIED.,.F.,.F.,.F.)
B_SPLINE_SURFACE_WITH_KNOTS((4,4),(4,1,1,1,1,1,1,4),(0.0376044687776927,
0.9632701597044),(0.03308221537891,0.1426814398896,0.2856169915253,0.4287844228248,
0.5720769018248,0.7151865898555,0.857914409195,0.9460833470288),
 .UNSPECIFIED.)
GEOMETRIC_REPRESENTATION_ITEM()
RATIONAL_B_SPLINE_SURFACE(((1.13246860461612,1.13246860461612,1.13246860461612,
1.13246860461612,1.13246860461612,1.13246860461612,1.13246860461612,1.13246860461612,
1.13246860461612,1.13246860461612),(0.955676754150111,0.955676754150111,
0.955676754150111,0.955676754150111,0.955676754150111,0.955676754150111,
0.955676754150111,0.955676754150111,0.955676754150111,0.955676754150111),
(0.955843956444876,0.955843956444876,0.955843956444876,0.955843956444876,
0.955843956444876,0.955843956444876,0.955843956444876,0.955843956444876,
0.955843956444876,0.955843956444876),(1.13297021150041,1.13297021150041,
1.13297021150041,1.13297021150041,1.13297021150041,1.13297021150041,1.13297021150041,
1.13297021150041,1.13297021150041,1.13297021150041)))
REPRESENTATION_ITEM('')
SURFACE()
);
#453=(
BOUNDED_SURFACE()
B_SPLINE_SURFACE(3,3,((#51149,#51150,#51151,#51152,#51153,#51154,#51155,
#51156,#51157,#51158,#51159),(#51160,#51161,#51162,#51163,#51164,#51165,
#51166,#51167,#51168,#51169,#51170),(#51171,#51172,#51173,#51174,#51175,
#51176,#51177,#51178,#51179,#51180,#51181),(#51182,#51183,#51184,#51185,
#51186,#51187,#51188,#51189,#51190,#51191,#51192)),.UNSPECIFIED.,.F.,.F.,
 .F.)
B_SPLINE_SURFACE_WITH_KNOTS((4,4),(4,1,1,1,1,1,1,1,4),(0.0522071605228554,
0.949229841408476),(0.244546321466786,0.2921614493104,0.3746006374515,0.4619240874495,
0.5486822225607,0.6295887174107,0.7017044698897,0.765848500065,0.768100603477379),
 .UNSPECIFIED.)
GEOMETRIC_REPRESENTATION_ITEM()
RATIONAL_B_SPLINE_SURFACE(((1.20432661363983,1.20432661363983,1.20432661363983,
1.20432661363983,1.20432661363983,1.20432661363983,1.20432661363983,1.20432661363983,
1.20432661363983,1.20432661363983,1.20432661363983),(0.931453995492728,
0.931453995492728,0.931453995492728,0.931453995492728,0.931453995492728,
0.931453995492728,0.931453995492728,0.931453995492728,0.931453995492728,
0.931453995492728,0.931453995492728),(0.931891830184036,0.931891830184036,
0.931891830184036,0.931891830184036,0.931891830184036,0.931891830184036,
0.931891830184036,0.931891830184036,0.931891830184036,0.931891830184036,
0.931891830184036),(1.20564011771375,1.20564011771375,1.20564011771375,
1.20564011771375,1.20564011771375,1.20564011771375,1.20564011771375,1.20564011771375,
1.20564011771375,1.20564011771375,1.20564011771375)))
REPRESENTATION_ITEM('')
SURFACE()
);
#454=(
BOUNDED_SURFACE()
B_SPLINE_SURFACE(3,3,((#51289,#51290,#51291,#51292,#51293,#51294,#51295,
#51296,#51297,#51298),(#51299,#51300,#51301,#51302,#51303,#51304,#51305,
#51306,#51307,#51308),(#51309,#51310,#51311,#51312,#51313,#51314,#51315,
#51316,#51317,#51318),(#51319,#51320,#51321,#51322,#51323,#51324,#51325,
#51326,#51327,#51328)),.UNSPECIFIED.,.F.,.F.,.F.)
B_SPLINE_SURFACE_WITH_KNOTS((4,4),(4,1,1,1,1,1,1,4),(0.0418851650492697,
0.963268717220642),(0.05391635099551,0.1420855915678,0.2848134105773,0.4279230981834,
0.5712155769628,0.7143830082179,0.8573185600922,0.9669169090932),
 .UNSPECIFIED.)
GEOMETRIC_REPRESENTATION_ITEM()
RATIONAL_B_SPLINE_SURFACE(((1.13002726603044,1.13002726603044,1.13002726603044,
1.13002726603044,1.13002726603044,1.13002726603044,1.13002726603044,1.13002726603044,
1.13002726603044,1.13002726603044),(0.955682356393539,0.955682356393539,
0.955682356393539,0.955682356393539,0.955682356393539,0.955682356393539,
0.955682356393539,0.955682356393539,0.955682356393539,0.955682356393539),
(0.956663063707594,0.956663063707594,0.956663063707594,0.956663063707594,
0.956663063707594,0.956663063707594,0.956663063707594,0.956663063707594,
0.956663063707594,0.956663063707594),(1.13296938797261,1.13296938797261,
1.13296938797261,1.13296938797261,1.13296938797261,1.13296938797261,1.13296938797261,
1.13296938797261,1.13296938797261,1.13296938797261)))
REPRESENTATION_ITEM('')
SURFACE()
);
#455=(
BOUNDED_SURFACE()
B_SPLINE_SURFACE(3,3,((#51482,#51483,#51484,#51485,#51486,#51487),(#51488,
#51489,#51490,#51491,#51492,#51493),(#51494,#51495,#51496,#51497,#51498,
#51499),(#51500,#51501,#51502,#51503,#51504,#51505)),.UNSPECIFIED.,.F.,
 .F.,.F.)
B_SPLINE_SURFACE_WITH_KNOTS((4,4),(4,1,1,4),(0.0606070589527452,0.939490000441276),
(0.199119625235957,0.3331969354622,0.6668030645378,0.800880379917306),
 .UNSPECIFIED.)
GEOMETRIC_REPRESENTATION_ITEM()
RATIONAL_B_SPLINE_SURFACE(((1.1746901488214,1.1746901488214,1.1746901488214,
1.1746901488214,1.1746901488214,1.1746901488214),(0.941744225021468,0.941744225021468,
0.941744225021468,0.941744225021468,0.941744225021468,0.941744225021468),
(0.941769953234294,0.941769953234295,0.941769953234294,0.941769953234294,
0.941769953234294,0.941769953234294),(1.17476733345988,1.17476733345988,
1.17476733345988,1.17476733345988,1.17476733345988,1.17476733345988)))
REPRESENTATION_ITEM('')
SURFACE()
);
#456=(
BOUNDED_SURFACE()
B_SPLINE_SURFACE(3,3,((#51772,#51773,#51774,#51775,#51776,#51777,#51778,
#51779,#51780,#51781,#51782,#51783,#51784,#51785,#51786,#51787,#51788,#51789,
#51790,#51791),(#51792,#51793,#51794,#51795,#51796,#51797,#51798,#51799,
#51800,#51801,#51802,#51803,#51804,#51805,#51806,#51807,#51808,#51809,#51810,
#51811),(#51812,#51813,#51814,#51815,#51816,#51817,#51818,#51819,#51820,
#51821,#51822,#51823,#51824,#51825,#51826,#51827,#51828,#51829,#51830,#51831),
(#51832,#51833,#51834,#51835,#51836,#51837,#51838,#51839,#51840,#51841,
#51842,#51843,#51844,#51845,#51846,#51847,#51848,#51849,#51850,#51851)),
 .UNSPECIFIED.,.F.,.F.,.F.)
B_SPLINE_SURFACE_WITH_KNOTS((4,4),(4,1,1,1,1,1,1,1,1,1,1,1,1,1,1,1,1,4),
(0.0633076699555623,0.939196073758018),(-0.00915383127714,0.,0.07546659123987,
0.1557180876053,0.2404001363484,0.3291523816828,0.4125158427852,0.485675861971,
0.5506578767173,0.6094485282683,0.6638170257839,0.7128077767044,0.7565087359807,
0.7968449582086,0.8357677603499,0.8748879264935,0.9149300941034,0.92753194056),
 .UNSPECIFIED.)
GEOMETRIC_REPRESENTATION_ITEM()
RATIONAL_B_SPLINE_SURFACE(((1.07645082753394,1.07645082753394,1.07645082753394,
1.07645082753394,1.07645082753394,1.07645082753394,1.07645082753394,1.07645082753394,
1.07645082753394,1.07645082753394,1.07645082753394,1.07645082753394,1.07645082753394,
1.07645082753394,1.07645082753394,1.07645082753394,1.07645082753394,1.07645082753394,
1.07645082753394,1.07645082753394),(0.974224173982434,0.974224173982434,
0.974224173982434,0.974224173982434,0.974224173982434,0.974224173982434,
0.974224173982434,0.974224173982434,0.974224173982434,0.974224173982434,
0.974224173982434,0.974224173982434,0.974224173982434,0.974224173982434,
0.974224173982434,0.974224173982434,0.974224173982434,0.974224173982434,
0.974224173982434,0.974224173982434),(0.97451722852402,0.97451722852402,
0.97451722852402,0.97451722852402,0.97451722852402,0.97451722852402,0.97451722852402,
0.97451722852402,0.97451722852402,0.97451722852402,0.97451722852402,0.97451722852402,
0.97451722852402,0.97451722852402,0.97451722852402,0.97451722852402,0.97451722852402,
0.97451722852402,0.97451722852402,0.97451722852402),(1.07732999115869,1.07732999115869,
1.07732999115869,1.07732999115869,1.07732999115869,1.07732999115869,1.07732999115869,
1.07732999115869,1.07732999115869,1.07732999115869,1.07732999115869,1.07732999115869,
1.07732999115869,1.07732999115869,1.07732999115869,1.07732999115869,1.07732999115869,
1.07732999115869,1.07732999115869,1.07732999115869)))
REPRESENTATION_ITEM('')
SURFACE()
);
#457=(
BOUNDED_SURFACE()
B_SPLINE_SURFACE(3,3,((#52013,#52014,#52015,#52016,#52017,#52018,#52019,
#52020,#52021,#52022),(#52023,#52024,#52025,#52026,#52027,#52028,#52029,
#52030,#52031,#52032),(#52033,#52034,#52035,#52036,#52037,#52038,#52039,
#52040,#52041,#52042),(#52043,#52044,#52045,#52046,#52047,#52048,#52049,
#52050,#52051,#52052)),.UNSPECIFIED.,.F.,.F.,.F.)
B_SPLINE_SURFACE_WITH_KNOTS((4,4),(4,1,1,1,1,1,1,4),(0.0534066136803702,
0.94724602026267),(0.235043827368409,0.2946028323238,0.3657508320856,0.445876802538,
0.5324642225534,0.6203243693421,0.7038886951953,0.755256380853433),
 .UNSPECIFIED.)
GEOMETRIC_REPRESENTATION_ITEM()
RATIONAL_B_SPLINE_SURFACE(((1.20323901910316,1.20323901910316,1.20323901910316,
1.20323901910316,1.20323901910316,1.20323901910316,1.20323901910316,1.20323901910316,
1.20323901910316,1.20323901910316),(0.932055656646419,0.932055656646419,
0.932055656646419,0.932055656646419,0.932055656646419,0.932055656646419,
0.932055656646419,0.932055656646419,0.932055656646419,0.932055656646419),
(0.932253804976139,0.932253804976139,0.932253804976139,0.932253804976139,
0.932253804976139,0.932253804976139,0.932253804976139,0.932253804976139,
0.932253804976139,0.932253804976139),(1.20383346409232,1.20383346409232,
1.20383346409232,1.20383346409232,1.20383346409232,1.20383346409232,1.20383346409232,
1.20383346409232,1.20383346409232,1.20383346409232)))
REPRESENTATION_ITEM('')
SURFACE()
);
#458=(
BOUNDED_SURFACE()
B_SPLINE_SURFACE(3,3,((#52172,#52173,#52174,#52175,#52176,#52177,#52178,
#52179,#52180,#52181,#52182),(#52183,#52184,#52185,#52186,#52187,#52188,
#52189,#52190,#52191,#52192,#52193),(#52194,#52195,#52196,#52197,#52198,
#52199,#52200,#52201,#52202,#52203,#52204),(#52205,#52206,#52207,#52208,
#52209,#52210,#52211,#52212,#52213,#52214,#52215)),.UNSPECIFIED.,.F.,.F.,
 .F.)
B_SPLINE_SURFACE_WITH_KNOTS((4,4),(4,1,1,1,1,1,1,1,4),(0.0595062761581278,
0.935433221282967),(0.05105962729005,0.1243084941807,0.2492353165502,0.3744835129416,
0.4998949769261,0.6253220276845,0.7506164023093,0.8756120170229,0.9160299525995),
 .UNSPECIFIED.)
GEOMETRIC_REPRESENTATION_ITEM()
RATIONAL_B_SPLINE_SURFACE(((1.11958821674223,1.11958821674223,1.11958821674223,
1.11958821674223,1.11958821674223,1.11958821674223,1.11958821674223,1.11958821674223,
1.11958821674223,1.11958821674223,1.11958821674223),(0.961053167403458,
0.961053167403458,0.961053167403458,0.961053167403458,0.961053167403458,
0.961053167403458,0.961053167403458,0.961053167403458,0.961053167403458,
0.961053167403458,0.961053167403458),(0.960142522166725,0.960142522166725,
0.960142522166725,0.960142522166725,0.960142522166725,0.960142522166725,
0.960142522166725,0.960142522166725,0.960142522166725,0.960142522166725,
0.960142522166725),(1.11685628103203,1.11685628103203,1.11685628103203,
1.11685628103203,1.11685628103203,1.11685628103203,1.11685628103203,1.11685628103203,
1.11685628103203,1.11685628103203,1.11685628103203)))
REPRESENTATION_ITEM('')
SURFACE()
);
#459=(
BOUNDED_SURFACE()
B_SPLINE_SURFACE(3,3,((#52449,#52450,#52451,#52452,#52453,#52454,#52455,
#52456,#52457,#52458,#52459),(#52460,#52461,#52462,#52463,#52464,#52465,
#52466,#52467,#52468,#52469,#52470),(#52471,#52472,#52473,#52474,#52475,
#52476,#52477,#52478,#52479,#52480,#52481),(#52482,#52483,#52484,#52485,
#52486,#52487,#52488,#52489,#52490,#52491,#52492)),.UNSPECIFIED.,.F.,.F.,
 .F.)
B_SPLINE_SURFACE_WITH_KNOTS((4,4),(4,1,1,1,1,1,1,1,4),(0.0575588785903921,
0.953164053882501),(0.2692226783974,0.2757404474013,0.3428253937552,0.4189611174942,
0.4999467364448,0.5809436838552,0.6571062155613,0.7242167269719,0.7307666831887),
 .UNSPECIFIED.)
GEOMETRIC_REPRESENTATION_ITEM()
RATIONAL_B_SPLINE_SURFACE(((1.19947338866439,1.19947338866439,1.19947338866439,
1.19947338866439,1.19947338866439,1.19947338866439,1.19947338866439,1.19947338866439,
1.19947338866439,1.19947338866439,1.19947338866439),(0.93028593361712,0.93028593361712,
0.93028593361712,0.93028593361712,0.93028593361712,0.93028593361712,0.93028593361712,
0.93028593361712,0.93028593361712,0.93028593361712,0.93028593361712),(0.933547925736913,
0.933547925736913,0.933547925736913,0.933547925736913,0.933547925736913,
0.933547925736913,0.933547925736913,0.933547925736913,0.933547925736913,
0.933547925736913,0.933547925736913),(1.20925936502377,1.20925936502377,
1.20925936502377,1.20925936502377,1.20925936502377,1.20925936502377,1.20925936502377,
1.20925936502377,1.20925936502377,1.20925936502377,1.20925936502377)))
REPRESENTATION_ITEM('')
SURFACE()
);
#460=(
BOUNDED_SURFACE()
B_SPLINE_SURFACE(3,3,((#52578,#52579,#52580,#52581,#52582,#52583,#52584,
#52585,#52586,#52587),(#52588,#52589,#52590,#52591,#52592,#52593,#52594,
#52595,#52596,#52597),(#52598,#52599,#52600,#52601,#52602,#52603,#52604,
#52605,#52606,#52607),(#52608,#52609,#52610,#52611,#52612,#52613,#52614,
#52615,#52616,#52617)),.UNSPECIFIED.,.F.,.F.,.F.)
B_SPLINE_SURFACE_WITH_KNOTS((4,4),(4,1,1,1,1,1,1,4),(0.0479830627277209,
0.946593353629165),(0.239518392063012,0.2430457920758,0.3242077589869,0.4151597383417,
0.5128629145943,0.6131453701819,0.7126591855993,0.770045878654716),
 .UNSPECIFIED.)
GEOMETRIC_REPRESENTATION_ITEM()
RATIONAL_B_SPLINE_SURFACE(((1.20821093302208,1.20821093302208,1.20821093302208,
1.20821093302208,1.20821093302208,1.20821093302208,1.20821093302208,1.20821093302208,
1.20821093302208,1.20821093302208),(0.932261852852764,0.932261852852764,
0.932261852852764,0.932261852852764,0.932261852852764,0.932261852852764,
0.932261852852764,0.932261852852764,0.932261852852764,0.932261852852764),
(0.93060634750094,0.93060634750094,0.93060634750094,0.93060634750094,0.93060634750094,
0.93060634750094,0.93060634750094,0.93060634750094,0.93060634750094,0.93060634750094),
(1.20324441696661,1.20324441696661,1.20324441696661,1.20324441696661,1.20324441696661,
1.20324441696661,1.20324441696661,1.20324441696661,1.20324441696661,1.20324441696661)))
REPRESENTATION_ITEM('')
SURFACE()
);
#461=(
BOUNDED_SURFACE()
B_SPLINE_SURFACE(3,3,((#52768,#52769,#52770,#52771,#52772,#52773,#52774,
#52775,#52776,#52777,#52778),(#52779,#52780,#52781,#52782,#52783,#52784,
#52785,#52786,#52787,#52788,#52789),(#52790,#52791,#52792,#52793,#52794,
#52795,#52796,#52797,#52798,#52799,#52800),(#52801,#52802,#52803,#52804,
#52805,#52806,#52807,#52808,#52809,#52810,#52811)),.UNSPECIFIED.,.F.,.F.,
 .F.)
B_SPLINE_SURFACE_WITH_KNOTS((4,4),(4,1,1,1,1,1,1,1,4),(0.0434902481459629,
0.937490443608701),(-0.009351371213944,0.,0.1428545029,0.2856984060337,
0.4287781897902,0.5720429752755,0.7151346717899,0.857843506892,0.9437353739471),
 .UNSPECIFIED.)
GEOMETRIC_REPRESENTATION_ITEM()
RATIONAL_B_SPLINE_SURFACE(((1.128442539186,1.128442539186,1.128442539186,
1.128442539186,1.128442539186,1.128442539186,1.128442539186,1.128442539186,
1.128442539186,1.128442539186,1.128442539186),(0.960753306302974,0.960753306302974,
0.960753306302974,0.960753306302974,0.960753306302974,0.960753306302974,
0.960753306302974,0.960753306302974,0.960753306302974,0.960753306302974,
0.960753306302974),(0.957260135350247,0.957260135350247,0.957260135350247,
0.957260135350247,0.957260135350247,0.957260135350247,0.957260135350247,
0.957260135350247,0.957260135350247,0.957260135350247,0.957260135350247),
(1.11796302632782,1.11796302632782,1.11796302632782,1.11796302632782,1.11796302632782,
1.11796302632782,1.11796302632782,1.11796302632782,1.11796302632782,1.11796302632782,
1.11796302632782)))
REPRESENTATION_ITEM('')
SURFACE()
);
#462=(
BOUNDED_SURFACE()
B_SPLINE_SURFACE(3,3,((#52961,#52962,#52963,#52964,#52965,#52966),(#52967,
#52968,#52969,#52970,#52971,#52972),(#52973,#52974,#52975,#52976,#52977,
#52978),(#52979,#52980,#52981,#52982,#52983,#52984)),.UNSPECIFIED.,.F.,
 .F.,.F.)
B_SPLINE_SURFACE_WITH_KNOTS((4,4),(4,1,1,4),(0.0606720801571754,0.938680242177121),
(-1.E-5,0.,0.3336142546261,0.663356363362649),.UNSPECIFIED.)
GEOMETRIC_REPRESENTATION_ITEM()
RATIONAL_B_SPLINE_SURFACE(((1.17463054351816,1.17463054351816,1.17463054351816,
1.17463054351816,1.17463054351816,1.17463054351816),(0.941961451143807,
0.941961451143807,0.941961451143807,0.941961451143807,0.941961451143807,
0.941961451143807),(0.941789945341621,0.941789945341621,0.941789945341621,
0.941789945341621,0.941789945341621,0.941789945341621),(1.1741160261116,
1.1741160261116,1.1741160261116,1.1741160261116,1.1741160261116,1.1741160261116)))
REPRESENTATION_ITEM('')
SURFACE()
);
#463=(
BOUNDED_SURFACE()
B_SPLINE_SURFACE(3,3,((#52994,#52995,#52996,#52997,#52998,#52999,#53000,
#53001,#53002,#53003,#53004,#53005,#53006,#53007,#53008,#53009),(#53010,
#53011,#53012,#53013,#53014,#53015,#53016,#53017,#53018,#53019,#53020,#53021,
#53022,#53023,#53024,#53025),(#53026,#53027,#53028,#53029,#53030,#53031,
#53032,#53033,#53034,#53035,#53036,#53037,#53038,#53039,#53040,#53041),
(#53042,#53043,#53044,#53045,#53046,#53047,#53048,#53049,#53050,#53051,
#53052,#53053,#53054,#53055,#53056,#53057)),.UNSPECIFIED.,.F.,.F.,.F.)
B_SPLINE_SURFACE_WITH_KNOTS((4,4),(4,1,1,1,1,1,1,1,1,1,1,1,1,4),(0.0607615083810939,
0.93302086581287),(-0.009395290942738,0.,0.0753533259589,0.1579195464055,
0.2496880158193,0.352840403202,0.4595197316146,0.5578787401128,0.6478313181872,
0.7283133787206,0.8001424242299,0.867942029368,0.9343337419824,0.9520744430681),
 .UNSPECIFIED.)
GEOMETRIC_REPRESENTATION_ITEM()
RATIONAL_B_SPLINE_SURFACE(((1.07734787781885,1.07734787781885,1.07734787781885,
1.07734787781885,1.07734787781885,1.07734787781885,1.07734787781885,1.07734787781885,
1.07734787781885,1.07734787781885,1.07734787781885,1.07734787781885,1.07734787781885,
1.07734787781885,1.07734787781885,1.07734787781885),(0.974947304262177,
0.974947304262177,0.974947304262177,0.974947304262177,0.974947304262177,
0.974947304262177,0.974947304262177,0.974947304262177,0.974947304262177,
0.974947304262177,0.974947304262177,0.974947304262177,0.974947304262177,
0.974947304262177,0.974947304262177,0.974947304262177),(0.974222540311786,
0.974222540311786,0.974222540311786,0.974222540311786,0.974222540311786,
0.974222540311786,0.974222540311786,0.974222540311786,0.974222540311786,
0.974222540311786,0.974222540311786,0.974222540311786,0.974222540311786,
0.974222540311786,0.974222540311786,0.974222540311786),(1.07517358596768,
1.07517358596768,1.07517358596768,1.07517358596768,1.07517358596768,1.07517358596768,
1.07517358596768,1.07517358596768,1.07517358596768,1.07517358596768,1.07517358596768,
1.07517358596768,1.07517358596768,1.07517358596768,1.07517358596768,1.07517358596768)))
REPRESENTATION_ITEM('')
SURFACE()
);
#464=(
BOUNDED_SURFACE()
B_SPLINE_SURFACE(3,3,((#53524,#53525,#53526,#53527,#53528,#53529,#53530,
#53531,#53532),(#53533,#53534,#53535,#53536,#53537,#53538,#53539,#53540,
#53541),(#53542,#53543,#53544,#53545,#53546,#53547,#53548,#53549,#53550),
(#53551,#53552,#53553,#53554,#53555,#53556,#53557,#53558,#53559)),
 .UNSPECIFIED.,.F.,.F.,.F.)
B_SPLINE_SURFACE_WITH_KNOTS((4,4),(4,1,1,1,1,1,4),(0.0580455652775177,0.958569362546839),
(0.2691839560331,0.3316611066132,0.4169070356234,0.499999867704,0.5830925415824,
0.6683381194025,0.7308257034814),.UNSPECIFIED.)
GEOMETRIC_REPRESENTATION_ITEM()
RATIONAL_B_SPLINE_SURFACE(((1.19903368051256,1.19903368051256,1.19903368051256,
1.19903368051256,1.19903368051256,1.19903368051256,1.19903368051256,1.19903368051256,
1.19903368051256),(0.928667097175851,0.928667097175851,0.928667097175851,
0.928667097175851,0.928667097175851,0.928667097175851,0.928667097175851,
0.928667097175851,0.928667097175851),(0.933749206229783,0.933749206229783,
0.933749206229783,0.933749206229783,0.933749206229783,0.933749206229783,
0.933749206229783,0.933749206229783,0.933749206229783),(1.21428000767435,
1.21428000767435,1.21428000767435,1.21428000767435,1.21428000767435,1.21428000767435,
1.21428000767435,1.21428000767435,1.21428000767435)))
REPRESENTATION_ITEM('')
SURFACE()
);
#465=(
BOUNDED_SURFACE()
B_SPLINE_SURFACE(3,3,((#53644,#53645,#53646,#53647,#53648,#53649,#53650,
#53651,#53652),(#53653,#53654,#53655,#53656,#53657,#53658,#53659,#53660,
#53661),(#53662,#53663,#53664,#53665,#53666,#53667,#53668,#53669,#53670),
(#53671,#53672,#53673,#53674,#53675,#53676,#53677,#53678,#53679)),
 .UNSPECIFIED.,.F.,.F.,.F.)
B_SPLINE_SURFACE_WITH_KNOTS((4,4),(4,1,1,1,1,1,4),(0.0491576255108182,0.946591020356229),
(0.22996558030876,0.2892821395991,0.3893944830893,0.4899684829189,0.5875628832777,
0.6780458245647,0.758314180295999),.UNSPECIFIED.)
GEOMETRIC_REPRESENTATION_ITEM()
RATIONAL_B_SPLINE_SURFACE(((1.20712810928682,1.20712810928682,1.20712810928682,
1.20712810928682,1.20712810928682,1.20712810928682,1.20712810928682,1.20712810928682,
1.20712810928682),(0.932259414885021,0.932259414885021,0.932259414885021,
0.932259414885021,0.932259414885021,0.932259414885021,0.932259414885021,
0.932259414885021,0.932259414885021),(0.930963436261351,0.930963436261351,
0.930963436261351,0.930963436261351,0.930963436261351,0.930963436261351,
0.930963436261351,0.930963436261351,0.930963436261351),(1.20324017341582,
1.20324017341582,1.20324017341582,1.20324017341582,1.20324017341582,1.20324017341582,
1.20324017341582,1.20324017341582,1.20324017341582)))
REPRESENTATION_ITEM('')
SURFACE()
);
#466=(
BOUNDED_SURFACE()
B_SPLINE_SURFACE(3,3,((#53796,#53797,#53798,#53799,#53800,#53801,#53802,
#53803,#53804,#53805),(#53806,#53807,#53808,#53809,#53810,#53811,#53812,
#53813,#53814,#53815),(#53816,#53817,#53818,#53819,#53820,#53821,#53822,
#53823,#53824,#53825),(#53826,#53827,#53828,#53829,#53830,#53831,#53832,
#53833,#53834,#53835)),.UNSPECIFIED.,.F.,.F.,.F.)
B_SPLINE_SURFACE_WITH_KNOTS((4,4),(4,1,1,1,1,1,1,4),(0.0418800048973985,
0.963270228783426),(0.03308221537886,0.1426814397772,0.2856169899415,0.4287844215146,
0.5720769018753,0.7151865925248,0.8579144138988,0.9460833470307),
 .UNSPECIFIED.)
GEOMETRIC_REPRESENTATION_ITEM()
RATIONAL_B_SPLINE_SURFACE(((1.1300301908407,1.1300301908407,1.1300301908407,
1.1300301908407,1.1300301908407,1.1300301908407,1.1300301908407,1.1300301908407,
1.1300301908407,1.1300301908407),(0.955682060901635,0.955682060901635,0.955682060901635,
0.955682060901635,0.955682060901635,0.955682060901635,0.955682060901635,
0.955682060901635,0.955682060901635,0.955682060901635),(0.956662081006193,
0.956662081006193,0.956662081006193,0.956662081006193,0.956662081006193,
0.956662081006193,0.956662081006193,0.956662081006193,0.956662081006193,
0.956662081006193),(1.13297025115438,1.13297025115438,1.13297025115438,
1.13297025115438,1.13297025115438,1.13297025115438,1.13297025115438,1.13297025115438,
1.13297025115438,1.13297025115438)))
REPRESENTATION_ITEM('')
SURFACE()
);
#467=(
BOUNDED_SURFACE()
B_SPLINE_SURFACE(3,3,((#53931,#53932,#53933,#53934,#53935,#53936,#53937,
#53938,#53939,#53940),(#53941,#53942,#53943,#53944,#53945,#53946,#53947,
#53948,#53949,#53950),(#53951,#53952,#53953,#53954,#53955,#53956,#53957,
#53958,#53959,#53960),(#53961,#53962,#53963,#53964,#53965,#53966,#53967,
#53968,#53969,#53970)),.UNSPECIFIED.,.F.,.F.,.F.)
B_SPLINE_SURFACE_WITH_KNOTS((4,4),(4,1,1,1,1,1,1,4),(0.0438856011091739,
0.946597267382723),(0.236379435895912,0.2520150267493,0.335933433698,0.4293648728823,
0.5272993584536,0.6257010423672,0.7220735755741,0.775269513209664),
 .UNSPECIFIED.)
GEOMETRIC_REPRESENTATION_ITEM()
RATIONAL_B_SPLINE_SURFACE(((1.21199876592565,1.21199876592565,1.21199876592565,
1.21199876592565,1.21199876592565,1.21199876592565,1.21199876592565,1.21199876592565,
1.21199876592565,1.21199876592565),(0.932282741901863,0.932282741901864,
0.932282741901864,0.932282741901864,0.932282741901864,0.932282741901864,
0.932282741901864,0.932282741901864,0.932282741901864,0.932282741901864),
(0.929364511089559,0.929364511089559,0.929364511089559,0.929364511089559,
0.929364511089559,0.929364511089559,0.929364511089559,0.929364511089559,
0.929364511089559,0.929364511089559),(1.20324407348874,1.20324407348874,
1.20324407348874,1.20324407348874,1.20324407348874,1.20324407348874,1.20324407348874,
1.20324407348874,1.20324407348874,1.20324407348874)))
REPRESENTATION_ITEM('')
SURFACE()
);
#468=(
BOUNDED_SURFACE()
B_SPLINE_SURFACE(3,3,((#54150,#54151,#54152,#54153,#54154,#54155,#54156,
#54157,#54158,#54159),(#54160,#54161,#54162,#54163,#54164,#54165,#54166,
#54167,#54168,#54169),(#54170,#54171,#54172,#54173,#54174,#54175,#54176,
#54177,#54178,#54179),(#54180,#54181,#54182,#54183,#54184,#54185,#54186,
#54187,#54188,#54189)),.UNSPECIFIED.,.F.,.F.,.F.)
B_SPLINE_SURFACE_WITH_KNOTS((4,4),(4,1,1,1,1,1,1,4),(0.0418844974680166,
0.963268781581434),(0.05391635099617,0.1420855946084,0.2848134123028,0.427923098216,
0.5712155761158,0.714383007194,0.8573185600195,0.9669169090932),
 .UNSPECIFIED.)
GEOMETRIC_REPRESENTATION_ITEM()
RATIONAL_B_SPLINE_SURFACE(((1.13002764499145,1.13002764499145,1.13002764499145,
1.13002764499145,1.13002764499145,1.13002764499145,1.13002764499145,1.13002764499145,
1.13002764499145,1.13002764499145),(0.955682342794086,0.955682342794086,
0.955682342794086,0.955682342794086,0.955682342794086,0.955682342794086,
0.955682342794086,0.955682342794086,0.955682342794086,0.955682342794086),
(0.956662936103217,0.956662936103217,0.956662936103217,0.956662936103217,
0.956662936103217,0.956662936103217,0.956662936103217,0.956662936103217,
0.956662936103217,0.956662936103217),(1.13296942491884,1.13296942491884,
1.13296942491884,1.13296942491884,1.13296942491884,1.13296942491884,1.13296942491884,
1.13296942491884,1.13296942491884,1.13296942491884)))
REPRESENTATION_ITEM('')
SURFACE()
);
#469=(
BOUNDED_SURFACE()
B_SPLINE_SURFACE(3,3,((#54343,#54344,#54345,#54346,#54347,#54348),(#54349,
#54350,#54351,#54352,#54353,#54354),(#54355,#54356,#54357,#54358,#54359,
#54360),(#54361,#54362,#54363,#54364,#54365,#54366)),.UNSPECIFIED.,.F.,
 .F.,.F.)
B_SPLINE_SURFACE_WITH_KNOTS((4,4),(4,1,1,4),(0.060607058952475,0.939489995743308),
(0.199119631433838,0.3331969354622,0.6668030645378,0.800880373770273),
 .UNSPECIFIED.)
GEOMETRIC_REPRESENTATION_ITEM()
RATIONAL_B_SPLINE_SURFACE(((1.17469014882161,1.17469014882161,1.17469014882161,
1.17469014882161,1.17469014882161,1.17469014882161),(0.941744226266654,
0.941744226266654,0.941744226266654,0.941744226266654,0.941744226266654,
0.941744226266654),(0.941769953233949,0.941769953233949,0.941769953233949,
0.941769953233949,0.941769953233949,0.941769953233949),(1.1747673297235,
1.1747673297235,1.1747673297235,1.1747673297235,1.1747673297235,1.1747673297235)))
REPRESENTATION_ITEM('')
SURFACE()
);
#470=(
BOUNDED_SURFACE()
B_SPLINE_SURFACE(3,3,((#54633,#54634,#54635,#54636,#54637,#54638,#54639,
#54640,#54641,#54642,#54643,#54644,#54645,#54646,#54647,#54648,#54649,#54650,
#54651,#54652),(#54653,#54654,#54655,#54656,#54657,#54658,#54659,#54660,
#54661,#54662,#54663,#54664,#54665,#54666,#54667,#54668,#54669,#54670,#54671,
#54672),(#54673,#54674,#54675,#54676,#54677,#54678,#54679,#54680,#54681,
#54682,#54683,#54684,#54685,#54686,#54687,#54688,#54689,#54690,#54691,#54692),
(#54693,#54694,#54695,#54696,#54697,#54698,#54699,#54700,#54701,#54702,
#54703,#54704,#54705,#54706,#54707,#54708,#54709,#54710,#54711,#54712)),
 .UNSPECIFIED.,.F.,.F.,.F.)
B_SPLINE_SURFACE_WITH_KNOTS((4,4),(4,1,1,1,1,1,1,1,1,1,1,1,1,1,1,1,1,4),
(0.0633076649181857,0.9392002877331),(-0.0091538312793,0.,0.07546639963989,
0.1557177906993,0.2403998675743,0.3291523205441,0.4125160476047,0.4856762677964,
0.5506584357867,0.6094492100254,0.6638177940728,0.7128085155366,0.7565093937176,
0.7968455102028,0.8357682044765,0.8748882668515,0.9149303281208,0.9275319405255),
 .UNSPECIFIED.)
GEOMETRIC_REPRESENTATION_ITEM()
RATIONAL_B_SPLINE_SURFACE(((1.07645082929997,1.07645082929997,1.07645082929997,
1.07645082929997,1.07645082929997,1.07645082929997,1.07645082929997,1.07645082929997,
1.07645082929997,1.07645082929997,1.07645082929997,1.07645082929997,1.07645082929997,
1.07645082929997,1.07645082929997,1.07645082929997,1.07645082929997,1.07645082929997,
1.07645082929997,1.07645082929997),(0.974223682156895,0.974223682156895,
0.974223682156895,0.974223682156895,0.974223682156895,0.974223682156895,
0.974223682156895,0.974223682156895,0.974223682156895,0.974223682156895,
0.974223682156895,0.974223682156895,0.974223682156895,0.974223682156895,
0.974223682156895,0.974223682156895,0.974223682156895,0.974223682156895,
0.974223682156895,0.974223682156895),(0.974517230754059,0.974517230754059,
0.974517230754059,0.974517230754059,0.974517230754059,0.974517230754059,
0.974517230754059,0.974517230754059,0.974517230754059,0.974517230754059,
0.974517230754059,0.974517230754059,0.974517230754059,0.974517230754059,
0.974517230754059,0.974517230754059,0.974517230754059,0.974517230754059,
0.974517230754059,0.974517230754059),(1.07733147509147,1.07733147509147,
1.07733147509147,1.07733147509147,1.07733147509147,1.07733147509147,1.07733147509147,
1.07733147509147,1.07733147509147,1.07733147509147,1.07733147509147,1.07733147509147,
1.07733147509147,1.07733147509147,1.07733147509147,1.07733147509147,1.07733147509147,
1.07733147509147,1.07733147509147,1.07733147509147)))
REPRESENTATION_ITEM('')
SURFACE()
);
#471=(
BOUNDED_SURFACE()
B_SPLINE_SURFACE(3,3,((#54874,#54875,#54876,#54877,#54878,#54879,#54880,
#54881,#54882,#54883),(#54884,#54885,#54886,#54887,#54888,#54889,#54890,
#54891,#54892,#54893),(#54894,#54895,#54896,#54897,#54898,#54899,#54900,
#54901,#54902,#54903),(#54904,#54905,#54906,#54907,#54908,#54909,#54910,
#54911,#54912,#54913)),.UNSPECIFIED.,.F.,.F.,.F.)
B_SPLINE_SURFACE_WITH_KNOTS((4,4),(4,1,1,1,1,1,1,4),(0.0471532343849083,
0.946601707615917),(0.229158000328599,0.2767714735063,0.372769960558,0.470949598223,
0.568892608243,0.662583621586,0.7468957137446,0.761354885822289),
 .UNSPECIFIED.)
GEOMETRIC_REPRESENTATION_ITEM()
RATIONAL_B_SPLINE_SURFACE(((1.20897622394021,1.20897622394021,1.20897622394021,
1.20897622394021,1.20897622394021,1.20897622394021,1.20897622394021,1.20897622394021,
1.20897622394021,1.20897622394021),(0.932262539405233,0.932262539405233,
0.932262539405233,0.932262539405233,0.932262539405233,0.932262539405233,
0.932262539405233,0.932262539405233,0.932262539405233,0.932262539405233),
(0.930354506555822,0.930354506555822,0.930354506555822,0.930354506555822,
0.930354506555822,0.930354506555822,0.930354506555822,0.930354506555822,
0.930354506555822,0.930354506555822),(1.20325212539198,1.20325212539198,
1.20325212539198,1.20325212539198,1.20325212539198,1.20325212539198,1.20325212539198,
1.20325212539198,1.20325212539198,1.20325212539198)))
REPRESENTATION_ITEM('')
SURFACE()
);
#472=(
BOUNDED_SURFACE()
B_SPLINE_SURFACE(3,3,((#55105,#55106,#55107,#55108,#55109,#55110,#55111,
#55112,#55113,#55114,#55115),(#55116,#55117,#55118,#55119,#55120,#55121,
#55122,#55123,#55124,#55125,#55126),(#55127,#55128,#55129,#55130,#55131,
#55132,#55133,#55134,#55135,#55136,#55137),(#55138,#55139,#55140,#55141,
#55142,#55143,#55144,#55145,#55146,#55147,#55148)),.UNSPECIFIED.,.F.,.F.,
 .F.)
B_SPLINE_SURFACE_WITH_KNOTS((4,4),(4,1,1,1,1,1,1,1,4),(0.059506601274082,
0.936820242954807),(0.05105962729005,0.1243084941807,0.2492353165502,0.3744835129416,
0.4998949769261,0.6253220276845,0.7506164023093,0.8756120170229,0.9160299525995),
 .UNSPECIFIED.)
GEOMETRIC_REPRESENTATION_ITEM()
RATIONAL_B_SPLINE_SURFACE(((1.11958804019898,1.11958804019898,1.11958804019898,
1.11958804019898,1.11958804019898,1.11958804019898,1.11958804019898,1.11958804019898,
1.11958804019898,1.11958804019898,1.11958804019898),(0.960802128231612,
0.960802128231612,0.960802128231612,0.960802128231612,0.960802128231612,
0.960802128231612,0.960802128231612,0.960802128231612,0.960802128231612,
0.960802128231612,0.960802128231612),(0.960140091762279,0.960140091762279,
0.960140091762279,0.960140091762279,0.960140091762279,0.960140091762279,
0.960140091762279,0.960140091762279,0.960140091762279,0.960140091762279,
0.960140091762279),(1.11760193079098,1.11760193079098,1.11760193079098,
1.11760193079098,1.11760193079098,1.11760193079098,1.11760193079098,1.11760193079098,
1.11760193079098,1.11760193079098,1.11760193079098)))
REPRESENTATION_ITEM('')
SURFACE()
);
#473=(
BOUNDED_SURFACE()
B_SPLINE_SURFACE(3,3,((#55382,#55383,#55384,#55385,#55386,#55387,#55388,
#55389,#55390,#55391,#55392),(#55393,#55394,#55395,#55396,#55397,#55398,
#55399,#55400,#55401,#55402,#55403),(#55404,#55405,#55406,#55407,#55408,
#55409,#55410,#55411,#55412,#55413,#55414),(#55415,#55416,#55417,#55418,
#55419,#55420,#55421,#55422,#55423,#55424,#55425)),.UNSPECIFIED.,.F.,.F.,
 .F.)
B_SPLINE_SURFACE_WITH_KNOTS((4,4),(4,1,1,1,1,1,1,1,4),(0.0556357165437915,
0.955304109070403),(0.2692123318637,0.2896670261853,0.3517274755791,0.422380333238,
0.5000250192074,0.5776669090115,0.6483133938419,0.7103683419862,0.730777134988),
 .UNSPECIFIED.)
GEOMETRIC_REPRESENTATION_ITEM()
RATIONAL_B_SPLINE_SURFACE(((1.20121075267841,1.20121075267841,1.20121075267841,
1.20121075267841,1.20121075267841,1.20121075267841,1.20121075267841,1.20121075267841,
1.20121075267841,1.20121075267841,1.20121075267841),(0.929627337657785,
0.929627337657785,0.929627337657785,0.929627337657785,0.929627337657785,
0.929627337657785,0.929627337657785,0.929627337657785,0.929627337657785,
0.929627337657785,0.929627337657785),(0.93297040022002,0.93297040022002,
0.93297040022002,0.93297040022002,0.93297040022002,0.93297040022002,0.93297040022002,
0.93297040022002,0.93297040022002,0.93297040022002,0.93297040022002),(1.21123994036511,
1.21123994036511,1.21123994036511,1.21123994036511,1.21123994036511,1.21123994036511,
1.21123994036511,1.21123994036511,1.21123994036511,1.21123994036511,1.21123994036511)))
REPRESENTATION_ITEM('')
SURFACE()
);
#474=(
BOUNDED_SURFACE()
B_SPLINE_SURFACE(3,3,((#55517,#55518,#55519,#55520,#55521,#55522,#55523,
#55524,#55525),(#55526,#55527,#55528,#55529,#55530,#55531,#55532,#55533,
#55534),(#55535,#55536,#55537,#55538,#55539,#55540,#55541,#55542,#55543),
(#55544,#55545,#55546,#55547,#55548,#55549,#55550,#55551,#55552)),
 .UNSPECIFIED.,.F.,.F.,.F.)
B_SPLINE_SURFACE_WITH_KNOTS((4,4),(4,1,1,1,1,1,4),(0.053271791488534,0.946598328512929),
(0.244689773436238,0.3238159337994,0.4243565900039,0.5246117495307,0.6233178136293,
0.720247333279,0.764677618064232),.UNSPECIFIED.)
GEOMETRIC_REPRESENTATION_ITEM()
RATIONAL_B_SPLINE_SURFACE(((1.20336592416562,1.20336592416562,1.20336592416562,
1.20336592416562,1.20336592416562,1.20336592416562,1.20336592416562,1.20336592416562,
1.20336592416562),(0.9322507758164,0.932250775816401,0.9322507758164,0.932250775816401,
0.932250775816401,0.932250775816401,0.932250775816401,0.932250775816401,
0.9322507758164),(0.932211364341593,0.932211364341593,0.932211364341593,
0.932211364341593,0.932211364341593,0.932211364341593,0.932211364341593,
0.932211364341593,0.932211364341593),(1.2032476897412,1.2032476897412,1.2032476897412,
1.2032476897412,1.2032476897412,1.2032476897412,1.2032476897412,1.2032476897412,
1.2032476897412)))
REPRESENTATION_ITEM('')
SURFACE()
);
#475=(
BOUNDED_SURFACE()
B_SPLINE_SURFACE(3,3,((#55689,#55690,#55691,#55692,#55693,#55694,#55695,
#55696,#55697,#55698,#55699),(#55700,#55701,#55702,#55703,#55704,#55705,
#55706,#55707,#55708,#55709,#55710),(#55711,#55712,#55713,#55714,#55715,
#55716,#55717,#55718,#55719,#55720,#55721),(#55722,#55723,#55724,#55725,
#55726,#55727,#55728,#55729,#55730,#55731,#55732)),.UNSPECIFIED.,.F.,.F.,
 .F.)
B_SPLINE_SURFACE_WITH_KNOTS((4,4),(4,1,1,1,1,1,1,1,4),(0.0422678684933725,
0.937007437303486),(-0.009351371213946,0.,0.1428545029,0.2856984060337,
0.4287781897902,0.5720429752755,0.7151346717899,0.857843506892,0.9437353739471),
 .UNSPECIFIED.)
GEOMETRIC_REPRESENTATION_ITEM()
RATIONAL_B_SPLINE_SURFACE(((1.12913131189582,1.12913131189582,1.12913131189582,
1.12913131189582,1.12913131189582,1.12913131189582,1.12913131189582,1.12913131189582,
1.12913131189582,1.12913131189582,1.12913131189582),(0.960854006789805,
0.960854006789805,0.960854006789805,0.960854006789805,0.960854006789805,
0.960854006789805,0.960854006789805,0.960854006789805,0.960854006789805,
0.960854006789805,0.960854006789805),(0.957044469016947,0.957044469016947,
0.957044469016947,0.957044469016947,0.957044469016947,0.957044469016947,
0.957044469016947,0.957044469016947,0.957044469016947,0.957044469016947,
0.957044469016947),(1.11770269857725,1.11770269857725,1.11770269857725,
1.11770269857725,1.11770269857725,1.11770269857725,1.11770269857725,1.11770269857725,
1.11770269857725,1.11770269857725,1.11770269857725)))
REPRESENTATION_ITEM('')
SURFACE()
);
#476=(
BOUNDED_SURFACE()
B_SPLINE_SURFACE(3,3,((#55882,#55883,#55884,#55885,#55886,#55887),(#55888,
#55889,#55890,#55891,#55892,#55893),(#55894,#55895,#55896,#55897,#55898,
#55899),(#55900,#55901,#55902,#55903,#55904,#55905)),.UNSPECIFIED.,.F.,
 .F.,.F.)
B_SPLINE_SURFACE_WITH_KNOTS((4,4),(4,1,1,4),(0.0606720801614013,0.938680242176577),
(-1.E-5,0.,0.333614254626,0.663356363361679),.UNSPECIFIED.)
GEOMETRIC_REPRESENTATION_ITEM()
RATIONAL_B_SPLINE_SURFACE(((1.1746305435148,1.1746305435148,1.1746305435148,
1.1746305435148,1.1746305435148,1.1746305435148),(0.941961451143949,0.941961451143949,
0.941961451143949,0.941961451143949,0.941961451143949,0.941961451143949),
(0.941789945342739,0.941789945342739,0.941789945342739,0.941789945342739,
0.941789945342739,0.941789945342739),(1.17411602611117,1.17411602611117,
1.17411602611117,1.17411602611117,1.17411602611117,1.17411602611117)))
REPRESENTATION_ITEM('')
SURFACE()
);
#477=(
BOUNDED_SURFACE()
B_SPLINE_SURFACE(3,3,((#55915,#55916,#55917,#55918,#55919,#55920,#55921,
#55922,#55923,#55924,#55925,#55926,#55927,#55928,#55929,#55930),(#55931,
#55932,#55933,#55934,#55935,#55936,#55937,#55938,#55939,#55940,#55941,#55942,
#55943,#55944,#55945,#55946),(#55947,#55948,#55949,#55950,#55951,#55952,
#55953,#55954,#55955,#55956,#55957,#55958,#55959,#55960,#55961,#55962),
(#55963,#55964,#55965,#55966,#55967,#55968,#55969,#55970,#55971,#55972,
#55973,#55974,#55975,#55976,#55977,#55978)),.UNSPECIFIED.,.F.,.F.,.F.)
B_SPLINE_SURFACE_WITH_KNOTS((4,4),(4,1,1,1,1,1,1,1,1,1,1,1,1,4),(0.060761509047659,
0.933020866626784),(-0.009395290942739,0.,0.07535332595895,0.1579195464056,
0.2496880158195,0.3528404032023,0.4595197316149,0.5578787401132,0.6478313181877,
0.7283133787211,0.8001424242306,0.8679420293686,0.9343337419829,0.9520744430681),
 .UNSPECIFIED.)
GEOMETRIC_REPRESENTATION_ITEM()
RATIONAL_B_SPLINE_SURFACE(((1.07734787758409,1.07734787758409,1.07734787758409,
1.07734787758409,1.07734787758409,1.07734787758409,1.07734787758409,1.07734787758409,
1.07734787758409,1.07734787758409,1.07734787758409,1.07734787758409,1.07734787758409,
1.07734787758409,1.07734787758409,1.07734787758409),(0.974947304165518,
0.974947304165518,0.974947304165518,0.974947304165518,0.974947304165518,
0.974947304165518,0.974947304165518,0.974947304165518,0.974947304165518,
0.974947304165518,0.974947304165518,0.974947304165518,0.974947304165518,
0.974947304165518,0.974947304165518,0.974947304165518),(0.974222540387579,
0.974222540387579,0.974222540387579,0.974222540387579,0.974222540387579,
0.974222540387579,0.974222540387579,0.974222540387579,0.974222540387579,
0.974222540387579,0.974222540387579,0.974222540387579,0.974222540387579,
0.974222540387579,0.974222540387579,0.974222540387579),(1.07517358625027,
1.07517358625027,1.07517358625027,1.07517358625027,1.07517358625027,1.07517358625027,
1.07517358625027,1.07517358625027,1.07517358625027,1.07517358625027,1.07517358625027,
1.07517358625027,1.07517358625027,1.07517358625027,1.07517358625027,1.07517358625027)))
REPRESENTATION_ITEM('')
SURFACE()
);
#478=(
BOUNDED_SURFACE()
B_SPLINE_SURFACE(3,3,((#56445,#56446,#56447,#56448,#56449,#56450,#56451,
#56452,#56453,#56454,#56455),(#56456,#56457,#56458,#56459,#56460,#56461,
#56462,#56463,#56464,#56465,#56466),(#56467,#56468,#56469,#56470,#56471,
#56472,#56473,#56474,#56475,#56476,#56477),(#56478,#56479,#56480,#56481,
#56482,#56483,#56484,#56485,#56486,#56487,#56488)),.UNSPECIFIED.,.F.,.F.,
 .F.)
B_SPLINE_SURFACE_WITH_KNOTS((4,4),(4,1,1,1,1,1,1,1,4),(0.0571956856471758,
0.954452770725331),(0.2692306949416,0.2749419490826,0.3416670598954,0.4177877612555,
0.4999458204015,0.5821135283534,0.658256170395,0.7250020340387,0.7307792782023),
 .UNSPECIFIED.)
GEOMETRIC_REPRESENTATION_ITEM()
RATIONAL_B_SPLINE_SURFACE(((1.19979901822718,1.19979901822718,1.1997990182272,
1.19979901822718,1.19979901822718,1.19979901822718,1.19979901822718,1.19979901822718,
1.19979901822718,1.19979901822718,1.19979901822718),(0.929896371414247,
0.929896371414247,0.929896371414343,0.929896371414247,0.929896371414247,
0.929896371414247,0.929896371414247,0.929896371414247,0.929896371414247,
0.929896371414247,0.929896371414247),(0.933446414971094,0.933446414971094,
0.933446414971189,0.933446414971094,0.933446414971094,0.933446414971094,
0.933446414971094,0.933446414971094,0.933446414971094,0.933446414971094,
0.933446414971094),(1.21044914889772,1.21044914889772,1.21044914889774,
1.21044914889772,1.21044914889772,1.21044914889772,1.21044914889772,1.21044914889772,
1.21044914889772,1.21044914889772,1.21044914889772)))
REPRESENTATION_ITEM('')
SURFACE()
);
#479=(
BOUNDED_SURFACE()
B_SPLINE_SURFACE(3,3,((#56645,#56646,#56647,#56648,#56649,#56650,#56651,
#56652,#56653),(#56654,#56655,#56656,#56657,#56658,#56659,#56660,#56661,
#56662),(#56663,#56664,#56665,#56666,#56667,#56668,#56669,#56670,#56671),
(#56672,#56673,#56674,#56675,#56676,#56677,#56678,#56679,#56680)),
 .UNSPECIFIED.,.F.,.F.,.F.)
B_SPLINE_SURFACE_WITH_KNOTS((4,4),(4,1,1,1,1,1,4),(0.0528061476738938,0.946595630268755),
(0.233696593713312,0.2806158094266,0.377846836066,0.4768946763461,0.5774309799662,
0.6780149464306,0.75477374610499),.UNSPECIFIED.)
GEOMETRIC_REPRESENTATION_ITEM()
RATIONAL_B_SPLINE_SURFACE(((1.20378794912229,1.20378794912229,1.20378794912229,
1.20378794912229,1.20378794912229,1.20378794912229,1.20378794912229,1.20378794912229,
1.20378794912229),(0.932252425012417,0.932252425012417,0.932252425012417,
0.932252425012417,0.932252425012417,0.932252425012417,0.932252425012417,
0.932252425012417,0.932252425012417),(0.932070805185767,0.932070805185767,
0.932070805185767,0.932070805185767,0.932070805185767,0.932070805185767,
0.932070805185767,0.932070805185767,0.932070805185767),(1.20324308964234,
1.20324308964234,1.20324308964234,1.20324308964234,1.20324308964234,1.20324308964234,
1.20324308964234,1.20324308964234,1.20324308964234)))
REPRESENTATION_ITEM('')
SURFACE()
);
#480=(
BOUNDED_SURFACE()
B_SPLINE_SURFACE(3,3,((#56781,#56782,#56783,#56784,#56785,#56786,#56787,
#56788,#56789,#56790),(#56791,#56792,#56793,#56794,#56795,#56796,#56797,
#56798,#56799,#56800),(#56801,#56802,#56803,#56804,#56805,#56806,#56807,
#56808,#56809,#56810),(#56811,#56812,#56813,#56814,#56815,#56816,#56817,
#56818,#56819,#56820)),.UNSPECIFIED.,.F.,.F.,.F.)
B_SPLINE_SURFACE_WITH_KNOTS((4,4),(4,1,1,1,1,1,1,4),(0.0418818139400337,
0.96327015985212),(0.03308221537868,0.1426814397217,0.2856169891585,0.4287844208669,
0.5720769019003,0.7151865938446,0.8579144162245,0.9460833470456),
 .UNSPECIFIED.)
GEOMETRIC_REPRESENTATION_ITEM()
RATIONAL_B_SPLINE_SURFACE(((1.13002916390669,1.13002916390669,1.13002916390669,
1.13002916390669,1.13002916390669,1.13002916390669,1.13002916390669,1.13002916390669,
1.13002916390669,1.13002916390669),(0.955682077793698,0.955682077793698,
0.955682077793698,0.955682077793698,0.955682077793698,0.955682077793698,
0.955682077793698,0.955682077793698,0.955682077793698,0.955682077793698),
(0.956662427019863,0.956662427019863,0.956662427019863,0.956662427019863,
0.956662427019863,0.956662427019863,0.956662427019863,0.956662427019863,
0.956662427019863,0.956662427019863),(1.13297021158519,1.13297021158519,
1.13297021158519,1.13297021158519,1.13297021158519,1.13297021158519,1.13297021158519,
1.13297021158519,1.13297021158519,1.13297021158519)))
REPRESENTATION_ITEM('')
SURFACE()
);
#481=(
BOUNDED_SURFACE()
B_SPLINE_SURFACE(3,3,((#56916,#56917,#56918,#56919,#56920,#56921,#56922,
#56923,#56924),(#56925,#56926,#56927,#56928,#56929,#56930,#56931,#56932,
#56933),(#56934,#56935,#56936,#56937,#56938,#56939,#56940,#56941,#56942),
(#56943,#56944,#56945,#56946,#56947,#56948,#56949,#56950,#56951)),
 .UNSPECIFIED.,.F.,.F.,.F.)
B_SPLINE_SURFACE_WITH_KNOTS((4,4),(4,1,1,1,1,1,4),(0.0492017398553194,0.946591167977457),
(0.241730237030952,0.3218312021396,0.4122894732501,0.5098786318471,0.6104690043264,
0.7106140261538,0.769990664121402),.UNSPECIFIED.)
GEOMETRIC_REPRESENTATION_ITEM()
RATIONAL_B_SPLINE_SURFACE(((1.20708756720507,1.20708756720507,1.20708756720507,
1.20708756720507,1.20708756720507,1.20708756720507,1.20708756720507,1.20708756720507,
1.20708756720507),(0.932259246075696,0.932259246075696,0.932259246075696,
0.932259246075696,0.932259246075696,0.932259246075696,0.932259246075696,
0.932259246075696,0.932259246075696),(0.930976823116939,0.930976823116939,
0.930976823116939,0.930976823116939,0.930976823116939,0.930976823116939,
0.930976823116939,0.930976823116939,0.930976823116939),(1.2032402983288,
1.2032402983288,1.2032402983288,1.2032402983288,1.2032402983288,1.2032402983288,
1.2032402983288,1.2032402983288,1.2032402983288)))
REPRESENTATION_ITEM('')
SURFACE()
);
#482=(
BOUNDED_SURFACE()
B_SPLINE_SURFACE(3,3,((#57045,#57046,#57047,#57048,#57049,#57050,#57051,
#57052,#57053,#57054),(#57055,#57056,#57057,#57058,#57059,#57060,#57061,
#57062,#57063,#57064),(#57065,#57066,#57067,#57068,#57069,#57070,#57071,
#57072,#57073,#57074),(#57075,#57076,#57077,#57078,#57079,#57080,#57081,
#57082,#57083,#57084)),.UNSPECIFIED.,.F.,.F.,.F.)
B_SPLINE_SURFACE_WITH_KNOTS((4,4),(4,1,1,1,1,1,1,4),(0.0418822688619605,
0.96326878165287),(0.05391635099207,0.1420855967788,0.2848134135343,0.4279230982392,
0.5712155755112,0.7143830064632,0.8573185599676,0.9669169090933),
 .UNSPECIFIED.)
GEOMETRIC_REPRESENTATION_ITEM()
RATIONAL_B_SPLINE_SURFACE(((1.1300289100912,1.1300289100912,1.1300289100912,
1.1300289100912,1.1300289100912,1.1300289100912,1.1300289100912,1.1300289100912,
1.1300289100912,1.1300289100912),(0.955682338038116,0.955682338038116,0.955682338038116,
0.955682338038116,0.955682338038116,0.955682338038116,0.955682338038116,
0.955682338038116,0.955682338038116,0.955682338038116),(0.956662509660705,
0.956662509660705,0.956662509660705,0.956662509660705,0.956662509660705,
0.956662509660705,0.956662509660705,0.956662509660705,0.956662509660705,
0.956662509660705),(1.13296942495897,1.13296942495897,1.13296942495897,
1.13296942495897,1.13296942495897,1.13296942495897,1.13296942495897,1.13296942495897,
1.13296942495897,1.13296942495897)))
REPRESENTATION_ITEM('')
SURFACE()
);
#483=(
BOUNDED_SURFACE()
B_SPLINE_SURFACE(3,3,((#57238,#57239,#57240,#57241,#57242,#57243),(#57244,
#57245,#57246,#57247,#57248,#57249),(#57250,#57251,#57252,#57253,#57254,
#57255),(#57256,#57257,#57258,#57259,#57260,#57261)),.UNSPECIFIED.,.F.,
 .F.,.F.)
B_SPLINE_SURFACE_WITH_KNOTS((4,4),(4,1,1,4),(0.0606070589478182,0.939490001387273),
(0.199119623286195,0.3331969354622,0.6668030645378,0.800880381172182),
 .UNSPECIFIED.)
GEOMETRIC_REPRESENTATION_ITEM()
RATIONAL_B_SPLINE_SURFACE(((1.17469014882531,1.17469014882531,1.17469014882531,
1.17469014882531,1.17469014882531,1.17469014882531),(0.941744224770734,
0.941744224770734,0.941744224770734,0.941744224770734,0.941744224770734,
0.941744224770734),(0.941769953233044,0.941769953233044,0.941769953233044,
0.941769953233044,0.941769953233044,0.941769953233044),(1.17476733421225,
1.17476733421225,1.17476733421225,1.17476733421225,1.17476733421225,1.17476733421225)))
REPRESENTATION_ITEM('')
SURFACE()
);
#484=(
BOUNDED_SURFACE()
B_SPLINE_SURFACE(3,3,((#57525,#57526,#57527,#57528,#57529,#57530,#57531,
#57532,#57533,#57534,#57535,#57536,#57537,#57538,#57539,#57540,#57541,#57542,
#57543,#57544),(#57545,#57546,#57547,#57548,#57549,#57550,#57551,#57552,
#57553,#57554,#57555,#57556,#57557,#57558,#57559,#57560,#57561,#57562,#57563,
#57564),(#57565,#57566,#57567,#57568,#57569,#57570,#57571,#57572,#57573,
#57574,#57575,#57576,#57577,#57578,#57579,#57580,#57581,#57582,#57583,#57584),
(#57585,#57586,#57587,#57588,#57589,#57590,#57591,#57592,#57593,#57594,
#57595,#57596,#57597,#57598,#57599,#57600,#57601,#57602,#57603,#57604)),
 .UNSPECIFIED.,.F.,.F.,.F.)
B_SPLINE_SURFACE_WITH_KNOTS((4,4),(4,1,1,1,1,1,1,1,1,1,1,1,1,1,1,1,1,4),
(0.063307662778757,0.939200287735074),(-0.009153831279309,0.,0.07546639963968,
0.155717790699,0.2403998675739,0.3291523205437,0.4125160476044,0.4856762677962,
0.5506584357865,0.6094492100253,0.6638177940728,0.7128085155366,0.7565093937177,
0.7968455102028,0.8357682044765,0.8748882668516,0.9149303281208,0.9275319405256),
 .UNSPECIFIED.)
GEOMETRIC_REPRESENTATION_ITEM()
RATIONAL_B_SPLINE_SURFACE(((1.07645083004906,1.07645083004906,1.07645083004906,
1.07645083004906,1.07645083004906,1.07645083004906,1.07645083004906,1.07645083004906,
1.07645083004906,1.07645083004906,1.07645083004906,1.07645083004906,1.07645083004906,
1.07645083004906,1.07645083004906,1.07645083004906,1.07645083004906,1.07645083004906,
1.07645083004906,1.07645083004906),(0.97422368215523,0.97422368215523,0.97422368215523,
0.97422368215523,0.97422368215523,0.97422368215523,0.97422368215523,0.97422368215523,
0.97422368215523,0.97422368215523,0.97422368215523,0.97422368215523,0.97422368215523,
0.97422368215523,0.97422368215523,0.97422368215523,0.97422368215523,0.97422368215523,
0.97422368215523,0.97422368215523),(0.974517230502929,0.974517230502929,
0.974517230502929,0.974517230502929,0.974517230502929,0.974517230502929,
0.974517230502929,0.974517230502929,0.974517230502929,0.974517230502929,
0.974517230502929,0.974517230502929,0.974517230502929,0.974517230502929,
0.974517230502929,0.974517230502929,0.974517230502929,0.974517230502929,
0.974517230502929,0.974517230502929),(1.07733147509216,1.07733147509216,
1.07733147509216,1.07733147509216,1.07733147509216,1.07733147509216,1.07733147509216,
1.07733147509216,1.07733147509216,1.07733147509216,1.07733147509216,1.07733147509216,
1.07733147509216,1.07733147509216,1.07733147509216,1.07733147509216,1.07733147509216,
1.07733147509216,1.07733147509216,1.07733147509216)))
REPRESENTATION_ITEM('')
SURFACE()
);
#485=(
BOUNDED_SURFACE()
B_SPLINE_SURFACE(3,3,((#57766,#57767,#57768,#57769,#57770,#57771,#57772,
#57773,#57774,#57775),(#57776,#57777,#57778,#57779,#57780,#57781,#57782,
#57783,#57784,#57785),(#57786,#57787,#57788,#57789,#57790,#57791,#57792,
#57793,#57794,#57795),(#57796,#57797,#57798,#57799,#57800,#57801,#57802,
#57803,#57804,#57805)),.UNSPECIFIED.,.F.,.F.,.F.)
B_SPLINE_SURFACE_WITH_KNOTS((4,4),(4,1,1,1,1,1,1,4),(0.0487270299825949,
0.94659521046586),(0.230696758264988,0.2874600458818,0.3870132126609,0.4873166184574,
0.5850151645794,0.675938646053,0.7570631380884,0.759743236107495),
 .UNSPECIFIED.)
GEOMETRIC_REPRESENTATION_ITEM()
RATIONAL_B_SPLINE_SURFACE(((1.20752814113149,1.20752814113149,1.20752814113149,
1.20752814113149,1.20752814113149,1.20752814113149,1.20752814113149,1.20752814113149,
1.20752814113149,1.20752814113149),(0.932258069051191,0.932258069051191,
0.932258069051191,0.932258069051191,0.932258069051191,0.932258069051191,
0.932258069051191,0.932258069051191,0.932258069051191,0.932258069051191),
(0.930831385763603,0.930831385763603,0.930831385763603,0.930831385763603,
0.930831385763603,0.930831385763603,0.930831385763603,0.930831385763603,
0.930831385763603,0.930831385763603),(1.20324809126873,1.20324809126873,
1.20324809126873,1.20324809126873,1.20324809126873,1.20324809126873,1.20324809126873,
1.20324809126873,1.20324809126873,1.20324809126873)))
REPRESENTATION_ITEM('')
SURFACE()
);
#486=(
BOUNDED_SURFACE()
B_SPLINE_SURFACE(3,3,((#57925,#57926,#57927,#57928,#57929,#57930,#57931,
#57932,#57933,#57934,#57935),(#57936,#57937,#57938,#57939,#57940,#57941,
#57942,#57943,#57944,#57945,#57946),(#57947,#57948,#57949,#57950,#57951,
#57952,#57953,#57954,#57955,#57956,#57957),(#57958,#57959,#57960,#57961,
#57962,#57963,#57964,#57965,#57966,#57967,#57968)),.UNSPECIFIED.,.F.,.F.,
 .F.)
B_SPLINE_SURFACE_WITH_KNOTS((4,4),(4,1,1,1,1,1,1,1,4),(0.0595203864762429,
0.937476996026637),(0.05105962729005,0.1243084941807,0.2492353165502,0.3744835129416,
0.4998949769261,0.6253220276845,0.7506164023093,0.8756120170229,0.9160299525995),
 .UNSPECIFIED.)
GEOMETRIC_REPRESENTATION_ITEM()
RATIONAL_B_SPLINE_SURFACE(((1.11958055541173,1.11958055541173,1.11958055541173,
1.11958055541173,1.11958055541173,1.11958055541173,1.11958055541173,1.11958055541173,
1.11958055541173,1.11958055541173,1.11958055541173),(0.960683244731665,
0.960683244731665,0.960683244731665,0.960683244731665,0.960683244731665,
0.960683244731665,0.960683244731665,0.960683244731665,0.960683244731665,
0.960683244731665,0.960683244731665),(0.960141667061955,0.960141667061955,
0.960141667061955,0.960141667061955,0.960141667061955,0.960141667061955,
0.960141667061955,0.960141667061955,0.960141667061955,0.960141667061955,
0.960141667061955),(1.1179558224026,1.1179558224026,1.1179558224026,1.1179558224026,
1.1179558224026,1.1179558224026,1.1179558224026,1.1179558224026,1.1179558224026,
1.1179558224026,1.1179558224026)))
REPRESENTATION_ITEM('')
SURFACE()
);
#487=(
BOUNDED_SURFACE()
B_SPLINE_SURFACE(3,3,((#58202,#58203,#58204,#58205,#58206,#58207,#58208,
#58209,#58210),(#58211,#58212,#58213,#58214,#58215,#58216,#58217,#58218,
#58219),(#58220,#58221,#58222,#58223,#58224,#58225,#58226,#58227,#58228),
(#58229,#58230,#58231,#58232,#58233,#58234,#58235,#58236,#58237)),
 .UNSPECIFIED.,.F.,.F.,.F.)
B_SPLINE_SURFACE_WITH_KNOTS((4,4),(4,1,1,1,1,1,4),(0.0580435500156731,0.958553804869728),
(0.2691745286223,0.3315918821098,0.4168737318583,0.5000003344174,0.583127115061,
0.6684093799117,0.7308143681514),.UNSPECIFIED.)
GEOMETRIC_REPRESENTATION_ITEM()
RATIONAL_B_SPLINE_SURFACE(((1.19903754000942,1.19903754000942,1.19903754000942,
1.19903754000942,1.19903754000942,1.19903754000942,1.19903754000942,1.19903754000942,
1.19903754000942),(0.928671012740672,0.928671012740672,0.928671012740672,
0.928671012740672,0.928671012740672,0.928671012740672,0.928671012740672,
0.928671012740672,0.928671012740672),(0.933747722450839,0.933747722450839,
0.933747722450839,0.933747722450839,0.933747722450839,0.933747722450839,
0.933747722450839,0.933747722450839,0.933747722450839),(1.21426766913992,
1.21426766913992,1.21426766913992,1.21426766913992,1.21426766913992,1.21426766913992,
1.21426766913992,1.21426766913992,1.21426766913992)))
REPRESENTATION_ITEM('')
SURFACE()
);
#488=(
BOUNDED_SURFACE()
B_SPLINE_SURFACE(3,3,((#58314,#58315,#58316,#58317,#58318,#58319,#58320,
#58321,#58322,#58323,#58324),(#58325,#58326,#58327,#58328,#58329,#58330,
#58331,#58332,#58333,#58334,#58335),(#58336,#58337,#58338,#58339,#58340,
#58341,#58342,#58343,#58344,#58345,#58346),(#58347,#58348,#58349,#58350,
#58351,#58352,#58353,#58354,#58355,#58356,#58357)),.UNSPECIFIED.,.F.,.F.,
 .F.)
B_SPLINE_SURFACE_WITH_KNOTS((4,4),(4,1,1,1,1,1,1,1,4),(0.0422653268062964,
0.937533390179831),(-0.009351371223958,0.,0.1428542653358,0.2856978653279,
0.4287777392072,0.5720428464823,0.7151350525691,0.8578442953538,0.9437353734563),
 .UNSPECIFIED.)
GEOMETRIC_REPRESENTATION_ITEM()
RATIONAL_B_SPLINE_SURFACE(((1.12913274597187,1.12913274597187,1.12913274597187,
1.12913274597187,1.12913274597187,1.12913274597187,1.12913274597187,1.12913274597187,
1.12913274597187,1.12913274597187,1.12913274597187),(0.960755109792916,
0.960755109792916,0.960755109792916,0.960755109792916,0.960755109792916,
0.960755109792916,0.960755109792916,0.960755109792916,0.960755109792916,
0.960755109792916,0.960755109792916),(0.957039590212626,0.957039590212626,
0.957039590212626,0.957039590212626,0.957039590212626,0.957039590212626,
0.957039590212626,0.957039590212626,0.957039590212626,0.957039590212626,
0.957039590212626),(1.117986187231,1.117986187231,1.117986187231,1.117986187231,
1.117986187231,1.117986187231,1.117986187231,1.117986187231,1.117986187231,
1.117986187231,1.117986187231)))
REPRESENTATION_ITEM('')
SURFACE()
);
#489=(
BOUNDED_SURFACE()
B_SPLINE_SURFACE(3,3,((#58567,#58568,#58569,#58570,#58571,#58572,#58573,
#58574,#58575),(#58576,#58577,#58578,#58579,#58580,#58581,#58582,#58583,
#58584),(#58585,#58586,#58587,#58588,#58589,#58590,#58591,#58592,#58593),
(#58594,#58595,#58596,#58597,#58598,#58599,#58600,#58601,#58602)),
 .UNSPECIFIED.,.F.,.F.,.F.)
B_SPLINE_SURFACE_WITH_KNOTS((4,4),(4,1,1,1,1,1,4),(0.0522319358346092,0.946599708933178),
(0.243637547330016,0.3281816498601,0.4286250598175,0.5281721425414,0.6260232294075,
0.7222208859256,0.765710581954822),.UNSPECIFIED.)
GEOMETRIC_REPRESENTATION_ITEM()
RATIONAL_B_SPLINE_SURFACE(((1.20431342445013,1.20431342445013,1.20431342445013,
1.20431342445013,1.20431342445013,1.20431342445013,1.20431342445013,1.20431342445013,
1.20431342445013),(0.932250933377241,0.932250933377241,0.932250933377241,
0.932250933377241,0.932250933377241,0.932250933377241,0.932250933377241,
0.932250933377241,0.932250933377241),(0.931895988864253,0.931895988864253,
0.931895988864253,0.931895988864253,0.931895988864253,0.931895988864253,
0.931895988864253,0.931895988864253,0.931895988864253),(1.20324859091116,
1.20324859091116,1.20324859091116,1.20324859091116,1.20324859091116,1.20324859091116,
1.20324859091116,1.20324859091116,1.20324859091116)))
REPRESENTATION_ITEM('')
SURFACE()
);
#490=(
BOUNDED_SURFACE()
B_SPLINE_SURFACE(3,3,((#58701,#58702,#58703,#58704,#58705,#58706,#58707,
#58708,#58709,#58710,#58711),(#58712,#58713,#58714,#58715,#58716,#58717,
#58718,#58719,#58720,#58721,#58722),(#58723,#58724,#58725,#58726,#58727,
#58728,#58729,#58730,#58731,#58732,#58733),(#58734,#58735,#58736,#58737,
#58738,#58739,#58740,#58741,#58742,#58743,#58744)),.UNSPECIFIED.,.F.,.F.,
 .F.)
B_SPLINE_SURFACE_WITH_KNOTS((4,4),(4,1,1,1,1,1,1,1,4),(0.0572670136322689,
0.950748781721039),(0.269229383309,0.2752759889051,0.3420135561061,0.4180771376681,
0.4999456411107,0.5818236269898,0.657909057418,0.7246675349474,0.7307806429001),
 .UNSPECIFIED.)
GEOMETRIC_REPRESENTATION_ITEM()
RATIONAL_B_SPLINE_SURFACE(((1.19973463403615,1.19973463403615,1.19973463403615,
1.19973463403615,1.19973463403615,1.19973463403615,1.19973463403615,1.19973463403615,
1.19973463403615,1.19973463403615,1.19973463403615),(0.931010957144128,
0.931010957144128,0.931010957144128,0.931010957144128,0.931010957144128,
0.931010957144128,0.931010957144128,0.931010957144128,0.931010957144128,
0.931010957144128,0.931010957144128),(0.933443613018979,0.933443613018979,
0.933443613018979,0.933443613018979,0.933443613018979,0.933443613018979,
0.933443613018979,0.933443613018979,0.933443613018979,0.933443613018979,
0.933443613018979),(1.2070326016607,1.2070326016607,1.2070326016607,1.2070326016607,
1.2070326016607,1.2070326016607,1.2070326016607,1.2070326016607,1.2070326016607,
1.2070326016607,1.2070326016607)))
REPRESENTATION_ITEM('')
SURFACE()
);
#491=(
BOUNDED_SURFACE()
B_SPLINE_SURFACE(3,3,((#59178,#59179,#59180,#59181,#59182,#59183,#59184,
#59185,#59186,#59187,#59188,#59189,#59190,#59191,#59192,#59193),(#59194,
#59195,#59196,#59197,#59198,#59199,#59200,#59201,#59202,#59203,#59204,#59205,
#59206,#59207,#59208,#59209),(#59210,#59211,#59212,#59213,#59214,#59215,
#59216,#59217,#59218,#59219,#59220,#59221,#59222,#59223,#59224,#59225),
(#59226,#59227,#59228,#59229,#59230,#59231,#59232,#59233,#59234,#59235,
#59236,#59237,#59238,#59239,#59240,#59241)),.UNSPECIFIED.,.F.,.F.,.F.)
B_SPLINE_SURFACE_WITH_KNOTS((4,4),(4,1,1,1,1,1,1,1,1,1,1,1,1,4),(0.0586203715926453,
0.933020863373606),(-0.009395290952153,0.,0.07535316275351,0.1579191313331,
0.2496874711698,0.3528406113057,0.4595229844577,0.5578824678157,0.6478335957937,
0.7283142435542,0.8001427386493,0.8679421724001,0.9343338107667,0.952074442993),
 .UNSPECIFIED.)
GEOMETRIC_REPRESENTATION_ITEM()
RATIONAL_B_SPLINE_SURFACE(((1.07810380266528,1.07810380266528,1.07810380266528,
1.07810380266528,1.07810380266528,1.07810380266528,1.07810380266528,1.07810380266528,
1.07810380266528,1.07810380266528,1.07810380266528,1.07810380266528,1.07810380266528,
1.07810380266528,1.07810380266528,1.07810380266528),(0.974951475937913,
0.974951475937913,0.974951475937913,0.974951475937913,0.974951475937913,
0.974951475937913,0.974951475937913,0.974951475937913,0.974951475937913,
0.974951475937913,0.974951475937913,0.974951475937913,0.974951475937913,
0.974951475937913,0.974951475937913,0.974951475937913),(0.973974736181131,
0.973974736181131,0.973974736181131,0.973974736181131,0.973974736181131,
0.973974736181131,0.973974736181131,0.973974736181131,0.973974736181131,
0.973974736181131,0.973974736181131,0.973974736181131,0.973974736181131,
0.973974736181131,0.973974736181131,0.973974736181131),(1.07517358339494,
1.07517358339494,1.07517358339494,1.07517358339494,1.07517358339494,1.07517358339494,
1.07517358339494,1.07517358339494,1.07517358339494,1.07517358339494,1.07517358339494,
1.07517358339494,1.07517358339494,1.07517358339494,1.07517358339494,1.07517358339494)))
REPRESENTATION_ITEM('')
SURFACE()
);
#492=(
BOUNDED_SURFACE()
B_SPLINE_SURFACE(3,3,((#59414,#59415,#59416,#59417,#59418,#59419),(#59420,
#59421,#59422,#59423,#59424,#59425),(#59426,#59427,#59428,#59429,#59430,
#59431),(#59432,#59433,#59434,#59435,#59436,#59437)),.UNSPECIFIED.,.F.,
 .F.,.F.)
B_SPLINE_SURFACE_WITH_KNOTS((4,4),(4,1,1,4),(0.0606720802686711,0.938680242175199),
(-1.E-5,0.,0.3335568389414,0.663356367030841),.UNSPECIFIED.)
GEOMETRIC_REPRESENTATION_ITEM()
RATIONAL_B_SPLINE_SURFACE(((1.17463054343028,1.17463054343028,1.17463054343028,
1.17463054343028,1.17463054343028,1.17463054343028),(0.941961451143953,
0.941961451143953,0.941961451143953,0.941961451143953,0.941961451143953,
0.941961451143953),(0.941789945370804,0.941789945370804,0.941789945370804,
0.941789945370804,0.941789945370804,0.941789945370804),(1.17411602611083,
1.17411602611083,1.17411602611083,1.17411602611083,1.17411602611083,1.17411602611083)))
REPRESENTATION_ITEM('')
SURFACE()
);
#493=(
BOUNDED_SURFACE()
B_SPLINE_SURFACE(3,3,((#59679,#59680,#59681,#59682,#59683,#59684,#59685,
#59686,#59687,#59688,#59689,#59690,#59691,#59692,#59693,#59694,#59695,#59696,
#59697,#59698),(#59699,#59700,#59701,#59702,#59703,#59704,#59705,#59706,
#59707,#59708,#59709,#59710,#59711,#59712,#59713,#59714,#59715,#59716,#59717,
#59718),(#59719,#59720,#59721,#59722,#59723,#59724,#59725,#59726,#59727,
#59728,#59729,#59730,#59731,#59732,#59733,#59734,#59735,#59736,#59737,#59738),
(#59739,#59740,#59741,#59742,#59743,#59744,#59745,#59746,#59747,#59748,
#59749,#59750,#59751,#59752,#59753,#59754,#59755,#59756,#59757,#59758)),
 .UNSPECIFIED.,.F.,.F.,.F.)
B_SPLINE_SURFACE_WITH_KNOTS((4,4),(4,1,1,1,1,1,1,1,1,1,1,1,1,1,1,1,1,4),
(0.0633076876987065,0.940112450452113),(-0.009153831272559,0.,0.07546697590282,
0.1557186836765,0.240400675928,0.3291525043907,0.4125154315421,0.4856750471872,
0.5506567542878,0.6094471595415,0.6638154833413,0.7128062934011,0.7565074154861,
0.7968438500049,0.8357668687042,0.874887243177,0.9149296242807,0.9275319406291),
 .UNSPECIFIED.)
GEOMETRIC_REPRESENTATION_ITEM()
RATIONAL_B_SPLINE_SURFACE(((1.07645082081108,1.07645082081108,1.07645082081108,
1.07645082081108,1.07645082081108,1.07645082081108,1.07645082081108,1.07645082081108,
1.07645082081108,1.07645082081108,1.07645082081108,1.07645082081108,1.07645082081108,
1.07645082081108,1.07645082081108,1.07645082081108,1.07645082081108,1.07645082081108,
1.07645082081108,1.07645082081108),(0.974117222049909,0.974117222049909,
0.974117222049909,0.974117222049909,0.974117222049909,0.974117222049909,
0.974117222049909,0.974117222049909,0.974117222049909,0.974117222049909,
0.974117222049909,0.974117222049909,0.974117222049909,0.974117222049909,
0.974117222049909,0.974117222049909,0.974117222049909,0.974117222049909,
0.974117222049909,0.974117222049909),(0.97451795619999,0.97451795619999,
0.97451795619999,0.97451795619999,0.97451795619999,0.97451795619999,0.97451795619999,
0.97451795619999,0.97451795619999,0.97451795619999,0.97451795619999,0.97451795619999,
0.97451795619999,0.97451795619999,0.97451795619999,0.97451795619999,0.97451795619999,
0.97451795619999,0.97451795619999,0.97451795619999),(1.07765302326132,1.07765302326132,
1.07765302326132,1.07765302326132,1.07765302326132,1.07765302326132,1.07765302326132,
1.07765302326132,1.07765302326132,1.07765302326132,1.07765302326132,1.07765302326132,
1.07765302326132,1.07765302326132,1.07765302326132,1.07765302326132,1.07765302326132,
1.07765302326132,1.07765302326132,1.07765302326132)))
REPRESENTATION_ITEM('')
SURFACE()
);
#494=(
BOUNDED_SURFACE()
B_SPLINE_SURFACE(3,3,((#59922,#59923,#59924,#59925,#59926,#59927,#59928,
#59929,#59930),(#59931,#59932,#59933,#59934,#59935,#59936,#59937,#59938,
#59939),(#59940,#59941,#59942,#59943,#59944,#59945,#59946,#59947,#59948),
(#59949,#59950,#59951,#59952,#59953,#59954,#59955,#59956,#59957)),
 .UNSPECIFIED.,.F.,.F.,.F.)
B_SPLINE_SURFACE_WITH_KNOTS((4,4),(4,1,1,1,1,1,4),(0.0556339209179322,0.946594676964208),
(0.23622684912609,0.2892204677235,0.3894748956345,0.4915097291946,0.5954545891223,
0.7006023497823,0.755351077420202),.UNSPECIFIED.)
GEOMETRIC_REPRESENTATION_ITEM()
RATIONAL_B_SPLINE_SURFACE(((1.20122430718483,1.20122430718483,1.20122430718483,
1.20122430718483,1.20122430718483,1.20122430718483,1.20122430718483,1.20122430718483,
1.20122430718483),(0.932252440213298,0.932252440213298,0.932252440213298,
0.932252440213298,0.932252440213298,0.932252440213298,0.932252440213298,
0.932252440213298,0.932252440213298),(0.932926918038345,0.932926918038345,
0.932926918038345,0.932926918038345,0.932926918038345,0.932926918038345,
0.932926918038345,0.932926918038345,0.932926918038345),(1.20324774065997,
1.20324774065997,1.20324774065997,1.20324774065997,1.20324774065997,1.20324774065997,
1.20324774065997,1.20324774065997,1.20324774065997)))
REPRESENTATION_ITEM('')
SURFACE()
);
#495=(
BOUNDED_SURFACE()
B_SPLINE_SURFACE(3,3,((#60077,#60078,#60079,#60080,#60081,#60082,#60083,
#60084,#60085,#60086,#60087),(#60088,#60089,#60090,#60091,#60092,#60093,
#60094,#60095,#60096,#60097,#60098),(#60099,#60100,#60101,#60102,#60103,
#60104,#60105,#60106,#60107,#60108,#60109),(#60110,#60111,#60112,#60113,
#60114,#60115,#60116,#60117,#60118,#60119,#60120)),.UNSPECIFIED.,.F.,.F.,
 .F.)
B_SPLINE_SURFACE_WITH_KNOTS((4,4),(4,1,1,1,1,1,1,1,4),(0.0595078021839535,
0.938342362610477),(0.05105962744621,0.1243082719354,0.2492351900332,0.374483525782,
0.4998948479171,0.6253218237211,0.750616579156,0.8756124488067,0.9160299520784),
 .UNSPECIFIED.)
GEOMETRIC_REPRESENTATION_ITEM()
RATIONAL_B_SPLINE_SURFACE(((1.1195873881288,1.1195873881288,1.1195873881288,
1.1195873881288,1.1195873881288,1.1195873881288,1.1195873881288,1.1195873881288,
1.1195873881288,1.1195873881288,1.1195873881288),(0.96052663714813,0.96052663714813,
0.96052663714813,0.96052663714813,0.96052663714813,0.96052663714813,0.96052663714813,
0.96052663714813,0.96052663714813,0.96052663714813,0.96052663714813),(0.960138486797252,
0.960138486797252,0.960138486797252,0.960138486797252,0.960138486797252,
0.960138486797252,0.960138486797252,0.960138486797252,0.960138486797252,
0.960138486797252,0.960138486797252),(1.11842293707616,1.11842293707616,
1.11842293707616,1.11842293707616,1.11842293707616,1.11842293707616,1.11842293707616,
1.11842293707616,1.11842293707616,1.11842293707616,1.11842293707616)))
REPRESENTATION_ITEM('')
SURFACE()
);
#496=(
BOUNDED_SURFACE()
B_SPLINE_SURFACE(3,3,((#60413,#60414,#60415,#60416,#60417,#60418,#60419,
#60420,#60421),(#60422,#60423,#60424,#60425,#60426,#60427,#60428,#60429,
#60430),(#60431,#60432,#60433,#60434,#60435,#60436,#60437,#60438,#60439),
(#60440,#60441,#60442,#60443,#60444,#60445,#60446,#60447,#60448)),
 .UNSPECIFIED.,.F.,.F.,.F.)
B_SPLINE_SURFACE_WITH_KNOTS((4,4),(4,1,1,1,1,1,4),(0.0549132206529749,0.961333582072497),
(0.269227069858,0.3329416456222,0.4153128648057,0.5000235250822,0.5847341870831,
0.6671012504363,0.7307621725325),.UNSPECIFIED.)
GEOMETRIC_REPRESENTATION_ITEM()
RATIONAL_B_SPLINE_SURFACE(((1.20186626112831,1.20186626112831,1.20186626112831,
1.20186626112831,1.20186626112831,1.20186626112831,1.20186626112831,1.20186626112831,
1.20186626112831),(0.92779882400403,0.92779882400403,0.92779882400403,0.92779882400403,
0.92779882400403,0.92779882400403,0.92779882400403,0.92779882400403,0.92779882400403),
(0.932800904262363,0.932800904262363,0.932800904262363,0.932800904262363,
0.932800904262363,0.932800904262363,0.932800904262363,0.932800904262363,
0.932800904262363),(1.21687250190331,1.21687250190331,1.21687250190331,
1.21687250190331,1.21687250190331,1.21687250190331,1.21687250190331,1.21687250190331,
1.21687250190331)))
REPRESENTATION_ITEM('')
SURFACE()
);
#497=(
BOUNDED_SURFACE()
B_SPLINE_SURFACE(3,3,((#60533,#60534,#60535,#60536,#60537,#60538,#60539,
#60540,#60541),(#60542,#60543,#60544,#60545,#60546,#60547,#60548,#60549,
#60550),(#60551,#60552,#60553,#60554,#60555,#60556,#60557,#60558,#60559),
(#60560,#60561,#60562,#60563,#60564,#60565,#60566,#60567,#60568)),
 .UNSPECIFIED.,.F.,.F.,.F.)
B_SPLINE_SURFACE_WITH_KNOTS((4,4),(4,1,1,1,1,1,4),(0.0551738827458389,0.94659152318391),
(0.245643394324907,0.2993405166024,0.4044749934007,0.5084175034907,0.6104536407677,
0.7107127111402,0.764615799035645),.UNSPECIFIED.)
GEOMETRIC_REPRESENTATION_ITEM()
RATIONAL_B_SPLINE_SURFACE(((1.20163682857439,1.20163682857439,1.20163682857439,
1.20163682857439,1.20163682857439,1.20163682857439,1.20163682857439,1.20163682857439,
1.20163682857439),(0.932254225678232,0.932254225678232,0.932254225678232,
0.932254225678232,0.932254225678232,0.932254225678232,0.932254225678232,
0.932254225678232,0.932254225678232),(0.932788782470288,0.932788782470288,
0.932788782470288,0.932788782470288,0.932788782470288,0.932788782470288,
0.932788782470288,0.932788782470288,0.932788782470288),(1.20324049895056,
1.20324049895056,1.20324049895056,1.20324049895056,1.20324049895056,1.20324049895056,
1.20324049895056,1.20324049895056,1.20324049895056)))
REPRESENTATION_ITEM('')
SURFACE()
);
#498=(
BOUNDED_SURFACE()
B_SPLINE_SURFACE(3,3,((#60663,#60664,#60665,#60666,#60667,#60668,#60669,
#60670,#60671,#60672),(#60673,#60674,#60675,#60676,#60677,#60678,#60679,
#60680,#60681,#60682),(#60683,#60684,#60685,#60686,#60687,#60688,#60689,
#60690,#60691,#60692),(#60693,#60694,#60695,#60696,#60697,#60698,#60699,
#60700,#60701,#60702)),.UNSPECIFIED.,.F.,.F.,.F.)
B_SPLINE_SURFACE_WITH_KNOTS((4,4),(4,1,1,1,1,1,1,4),(0.041884544995783,
0.963268707501492),(0.05391635144467,0.142084834672,0.2848129606579,0.4279230595161,
0.5712157651896,0.7143832496897,0.8573185671688,0.966916909086),
 .UNSPECIFIED.)
GEOMETRIC_REPRESENTATION_ITEM()
RATIONAL_B_SPLINE_SURFACE(((1.13002761804694,1.13002761804694,1.13002761804694,
1.13002761804694,1.13002761804694,1.13002761804694,1.13002761804694,1.13002761804694,
1.13002761804694,1.13002761804694),(0.955682356900717,0.955682356900717,
0.955682356900717,0.955682356900717,0.955682356900717,0.955682356900717,
0.955682356900717,0.955682356900717,0.955682356900717,0.955682356900717),
(0.956662945028202,0.956662945028202,0.956662945028202,0.956662945028202,
0.956662945028202,0.956662945028202,0.956662945028202,0.956662945028202,
0.956662945028202,0.956662945028202),(1.1329693824294,1.1329693824294,1.1329693824294,
1.1329693824294,1.1329693824294,1.1329693824294,1.1329693824294,1.1329693824294,
1.1329693824294,1.1329693824294)))
REPRESENTATION_ITEM('')
SURFACE()
);
#499=(
BOUNDED_SURFACE()
B_SPLINE_SURFACE(3,3,((#60795,#60796,#60797,#60798,#60799,#60800),(#60801,
#60802,#60803,#60804,#60805,#60806),(#60807,#60808,#60809,#60810,#60811,
#60812),(#60813,#60814,#60815,#60816,#60817,#60818)),.UNSPECIFIED.,.F.,
 .F.,.F.)
B_SPLINE_SURFACE_WITH_KNOTS((4,4),(4,1,1,4),(0.0606070674814838,0.939489987503615),
(0.199119642928049,0.3332353956662,0.6667646043338,0.800880362821028),
 .UNSPECIFIED.)
GEOMETRIC_REPRESENTATION_ITEM()
RATIONAL_B_SPLINE_SURFACE(((1.17469014203132,1.17469014203132,1.17469014203132,
1.17469014203132,1.17469014203132,1.17469014203132),(0.941744228453835,
0.941744228453835,0.941744228453835,0.941744228453835,0.941744228453835,
0.941744228453835),(0.941769955497328,0.941769955497328,0.941769955497328,
0.941769955497328,0.941769955497328,0.941769955497328),(1.1747673231618,
1.1747673231618,1.1747673231618,1.1747673231618,1.1747673231618,1.1747673231618)))
REPRESENTATION_ITEM('')
SURFACE()
);
#500=(
BOUNDED_SURFACE()
B_SPLINE_SURFACE(3,3,((#60824,#60825,#60826,#60827,#60828,#60829,#60830,
#60831,#60832,#60833),(#60834,#60835,#60836,#60837,#60838,#60839,#60840,
#60841,#60842,#60843),(#60844,#60845,#60846,#60847,#60848,#60849,#60850,
#60851,#60852,#60853),(#60854,#60855,#60856,#60857,#60858,#60859,#60860,
#60861,#60862,#60863)),.UNSPECIFIED.,.F.,.F.,.F.)
B_SPLINE_SURFACE_WITH_KNOTS((4,4),(4,1,1,1,1,1,1,4),(0.0418820911112758,
0.963270219149611),(0.03308221537276,0.1426814328191,0.2856167501412,0.4287842346698,
0.5720769404872,0.7151870396265,0.8579151658318,0.9460833466072),
 .UNSPECIFIED.)
GEOMETRIC_REPRESENTATION_ITEM()
RATIONAL_B_SPLINE_SURFACE(((1.13002900659617,1.13002900659617,1.13002900659617,
1.13002900659617,1.13002900659617,1.13002900659617,1.13002900659617,1.13002900659617,
1.13002900659617,1.13002900659617),(0.95568206715303,0.95568206715303,0.95568206715303,
0.95568206715303,0.95568206715303,0.95568206715303,0.95568206715303,0.95568206715303,
0.95568206715303,0.95568206715303),(0.956662480172929,0.956662480172929,
0.956662480172929,0.956662480172929,0.956662480172929,0.956662480172929,
0.956662480172929,0.956662480172929,0.956662480172929,0.956662480172929),
(1.13297024565587,1.13297024565587,1.13297024565587,1.13297024565587,1.13297024565587,
1.13297024565587,1.13297024565587,1.13297024565587,1.13297024565587,1.13297024565587)))
REPRESENTATION_ITEM('')
SURFACE()
);
#501=(
BOUNDED_SURFACE()
B_SPLINE_SURFACE(3,3,((#61020,#61021,#61022,#61023,#61024,#61025,#61026,
#61027,#61028),(#61029,#61030,#61031,#61032,#61033,#61034,#61035,#61036,
#61037),(#61038,#61039,#61040,#61041,#61042,#61043,#61044,#61045,#61046),
(#61047,#61048,#61049,#61050,#61051,#61052,#61053,#61054,#61055)),
 .UNSPECIFIED.,.F.,.F.,.F.)
B_SPLINE_SURFACE_WITH_KNOTS((4,4),(4,1,1,1,1,1,4),(0.0519164749251763,0.946596975406882),
(0.23281373816856,0.2786409342623,0.3751379338287,0.4733293945345,0.5731667317773,
0.6736811683426,0.755675667880648),.UNSPECIFIED.)
GEOMETRIC_REPRESENTATION_ITEM()
RATIONAL_B_SPLINE_SURFACE(((1.20459928322244,1.20459928322244,1.20459928322244,
1.20459928322244,1.20459928322244,1.20459928322244,1.20459928322244,1.20459928322244,
1.20459928322244),(0.932252754256132,0.932252754256133,0.932252754256132,
0.932252754256132,0.932252754256132,0.932252754256132,0.932252754256132,
0.932252754256133,0.932252754256132),(0.931800989552072,0.931800989552072,
0.931800989552072,0.931800989552072,0.931800989552072,0.931800989552072,
0.931800989552072,0.931800989552072,0.931800989552072),(1.20324398911026,
1.20324398911026,1.20324398911026,1.20324398911026,1.20324398911026,1.20324398911026,
1.20324398911026,1.20324398911026,1.20324398911026)))
REPRESENTATION_ITEM('')
SURFACE()
);
#502=(
BOUNDED_SURFACE()
B_SPLINE_SURFACE(3,3,((#61113,#61114,#61115,#61116,#61117,#61118,#61119,
#61120,#61121,#61122),(#61123,#61124,#61125,#61126,#61127,#61128,#61129,
#61130,#61131,#61132),(#61133,#61134,#61135,#61136,#61137,#61138,#61139,
#61140,#61141,#61142),(#61143,#61144,#61145,#61146,#61147,#61148,#61149,
#61150,#61151,#61152)),.UNSPECIFIED.,.F.,.F.,.F.)
B_SPLINE_SURFACE_WITH_KNOTS((4,4),(4,1,1,1,1,1,1,4),(0.0506777938854956,
0.94932519705549),(0.077728727808056,0.1141533201323,0.2302983301971,0.3458029403667,
0.4595257213141,0.5713502050872,0.6814413055602,0.713640661394635),
 .UNSPECIFIED.)
GEOMETRIC_REPRESENTATION_ITEM()
RATIONAL_B_SPLINE_SURFACE(((1.20573036432394,1.20573036432394,1.20573036432394,
1.20573036432394,1.20573036432394,1.20573036432394,1.20573036432394,1.20573036432394,
1.20573036432394,1.20573036432394),(0.931422298920844,0.931422298920844,
0.931422298920844,0.931422298920844,0.931422298920844,0.931422298920844,
0.931422298920844,0.931422298920844,0.931422298920844,0.931422298920844),
(0.931423211895124,0.931423211895124,0.931423211895124,0.931423211895124,
0.931423211895124,0.931423211895124,0.931423211895124,0.931423211895124,
0.931423211895124,0.931423211895124),(1.20573310324678,1.20573310324678,
1.20573310324678,1.20573310324678,1.20573310324678,1.20573310324678,1.20573310324678,
1.20573310324678,1.20573310324678,1.20573310324678)))
REPRESENTATION_ITEM('')
SURFACE()
);
#503=(
BOUNDED_SURFACE()
B_SPLINE_SURFACE(3,3,((#61240,#61241,#61242,#61243,#61244,#61245,#61246,
#61247,#61248,#61249,#61250),(#61251,#61252,#61253,#61254,#61255,#61256,
#61257,#61258,#61259,#61260,#61261),(#61262,#61263,#61264,#61265,#61266,
#61267,#61268,#61269,#61270,#61271,#61272),(#61273,#61274,#61275,#61276,
#61277,#61278,#61279,#61280,#61281,#61282,#61283)),.UNSPECIFIED.,.F.,.F.,
 .F.)
B_SPLINE_SURFACE_WITH_KNOTS((4,4),(4,1,1,1,1,1,1,1,4),(0.0434902479384873,
0.93850620438699),(-0.009351371213917,0.,0.1428545029,0.2856984060337,0.4287781897902,
0.5720429752755,0.7151346717899,0.857843506892,0.9437353739471),
 .UNSPECIFIED.)
GEOMETRIC_REPRESENTATION_ITEM()
RATIONAL_B_SPLINE_SURFACE(((1.12844253916938,1.12844253916938,1.12844253916938,
1.12844253916938,1.12844253916938,1.12844253916938,1.12844253916938,1.12844253916938,
1.12844253916938,1.12844253916938,1.12844253916938),(0.960562778259995,
0.960562778259995,0.960562778259995,0.960562778259995,0.960562778259995,
0.960562778259995,0.960562778259995,0.960562778259995,0.960562778259995,
0.960562778259995,0.960562778259995),(0.957252409461222,0.957252409461222,
0.957252409461222,0.957252409461222,0.957252409461222,0.957252409461222,
0.957252409461222,0.957252409461222,0.957252409461222,0.957252409461222,
0.957252409461222),(1.11851143277306,1.11851143277306,1.11851143277306,
1.11851143277306,1.11851143277306,1.11851143277306,1.11851143277306,1.11851143277306,
1.11851143277306,1.11851143277306,1.11851143277306)))
REPRESENTATION_ITEM('')
SURFACE()
);
#504=(
BOUNDED_SURFACE()
B_SPLINE_SURFACE(3,3,((#61433,#61434,#61435,#61436,#61437,#61438),(#61439,
#61440,#61441,#61442,#61443,#61444),(#61445,#61446,#61447,#61448,#61449,
#61450),(#61451,#61452,#61453,#61454,#61455,#61456)),.UNSPECIFIED.,.F.,
 .F.,.F.)
B_SPLINE_SURFACE_WITH_KNOTS((4,4),(4,1,1,4),(0.0606720801571683,0.938680239727398),
(-1.E-5,0.,0.3336142546261,0.663356363362683),.UNSPECIFIED.)
GEOMETRIC_REPRESENTATION_ITEM()
RATIONAL_B_SPLINE_SURFACE(((1.17463054351817,1.17463054351817,1.17463054351817,
1.17463054351817,1.17463054351817,1.17463054351817),(0.941961451792975,
0.941961451792975,0.941961451792975,0.941961451792975,0.941961451792975,
0.941961451792975),(0.941789945342576,0.941789945342576,0.941789945342576,
0.941789945342576,0.941789945342576,0.941789945342576),(1.17411602416697,
1.17411602416697,1.17411602416697,1.17411602416697,1.17411602416697,1.17411602416697)))
REPRESENTATION_ITEM('')
SURFACE()
);
#505=(
BOUNDED_SURFACE()
B_SPLINE_SURFACE(3,3,((#61466,#61467,#61468,#61469,#61470,#61471,#61472,
#61473,#61474,#61475,#61476,#61477,#61478,#61479,#61480,#61481),(#61482,
#61483,#61484,#61485,#61486,#61487,#61488,#61489,#61490,#61491,#61492,#61493,
#61494,#61495,#61496,#61497),(#61498,#61499,#61500,#61501,#61502,#61503,
#61504,#61505,#61506,#61507,#61508,#61509,#61510,#61511,#61512,#61513),
(#61514,#61515,#61516,#61517,#61518,#61519,#61520,#61521,#61522,#61523,
#61524,#61525,#61526,#61527,#61528,#61529)),.UNSPECIFIED.,.F.,.F.,.F.)
B_SPLINE_SURFACE_WITH_KNOTS((4,4),(4,1,1,1,1,1,1,1,1,1,1,1,1,4),(0.0608897632428477,
0.933027487588604),(-0.009395290939728,0.,0.07535337983447,0.1579196834309,
0.2496881956056,0.3528403343846,0.4595186573857,0.5578775090873,0.6478305660607,
0.7283130931759,0.8001423204479,0.8679419821683,0.9343337192845,0.9520744430929),
 .UNSPECIFIED.)
GEOMETRIC_REPRESENTATION_ITEM()
RATIONAL_B_SPLINE_SURFACE(((1.07730271481584,1.07730271481584,1.07730271481584,
1.07730271481584,1.07730271481584,1.07730271481584,1.07730271481584,1.07730271481584,
1.07730271481584,1.07730271481584,1.07730271481584,1.07730271481584,1.07730271481584,
1.07730271481584,1.07730271481584,1.07730271481584),(0.974946315986727,
0.974946315986727,0.974946315986727,0.974946315986727,0.974946315986727,
0.974946315986727,0.974946315986727,0.974946315986727,0.974946315986727,
0.974946315986727,0.974946315986727,0.974946315986727,0.974946315986727,
0.974946315986727,0.974946315986727,0.974946315986727),(0.974237372938085,
0.974237372938085,0.974237372938085,0.974237372938085,0.974237372938085,
0.974237372938085,0.974237372938085,0.974237372938085,0.974237372938085,
0.974237372938085,0.974237372938085,0.974237372938085,0.974237372938085,
0.974237372938085,0.974237372938085,0.974237372938085),(1.07517588566991,
1.07517588566991,1.07517588566991,1.07517588566991,1.07517588566991,1.07517588566991,
1.07517588566991,1.07517588566991,1.07517588566991,1.07517588566991,1.07517588566991,
1.07517588566991,1.07517588566991,1.07517588566991,1.07517588566991,1.07517588566991)))
REPRESENTATION_ITEM('')
SURFACE()
);
#506=(
BOUNDED_SURFACE()
B_SPLINE_SURFACE(3,3,((#61996,#61997,#61998,#61999,#62000,#62001,#62002,
#62003,#62004,#62005),(#62006,#62007,#62008,#62009,#62010,#62011,#62012,
#62013,#62014,#62015),(#62016,#62017,#62018,#62019,#62020,#62021,#62022,
#62023,#62024,#62025),(#62026,#62027,#62028,#62029,#62030,#62031,#62032,
#62033,#62034,#62035)),.UNSPECIFIED.,.F.,.F.,.F.)
B_SPLINE_SURFACE_WITH_KNOTS((4,4),(4,1,1,1,1,1,1,4),(0.0329440013745224,
0.967052315169442),(0.2245728991605,0.2654375946881,0.3544413771844,0.4511118902311,
0.549022999066,0.6456758358933,0.7346467284996,0.775427045264),
 .UNSPECIFIED.)
GEOMETRIC_REPRESENTATION_ITEM()
RATIONAL_B_SPLINE_SURFACE(((1.22228338242005,1.22228338242005,1.22228338242005,
1.22228338242005,1.22228338242005,1.22228338242005,1.22228338242005,1.22228338242005,
1.22228338242005,1.22228338242005),(0.925906707891112,0.925906707891112,
0.925906707891112,0.925906707891112,0.925906707891112,0.925906707891112,
0.925906707891112,0.925906707891112,0.925906707891112,0.925906707891112),
(0.925905539197793,0.925905539197793,0.925905539197793,0.925905539197793,
0.925905539197793,0.925905539197793,0.925905539197793,0.925905539197793,
0.925905539197793,0.925905539197793),(1.22227987634009,1.22227987634009,
1.22227987634009,1.22227987634009,1.22227987634009,1.22227987634009,1.22227987634009,
1.22227987634009,1.22227987634009,1.22227987634009)))
REPRESENTATION_ITEM('')
SURFACE()
);
#507=(
BOUNDED_SURFACE()
B_SPLINE_SURFACE(3,3,((#62123,#62124,#62125,#62126,#62127,#62128,#62129,
#62130,#62131,#62132),(#62133,#62134,#62135,#62136,#62137,#62138,#62139,
#62140,#62141,#62142),(#62143,#62144,#62145,#62146,#62147,#62148,#62149,
#62150,#62151,#62152),(#62153,#62154,#62155,#62156,#62157,#62158,#62159,
#62160,#62161,#62162)),.UNSPECIFIED.,.F.,.F.,.F.)
B_SPLINE_SURFACE_WITH_KNOTS((4,4),(4,1,1,1,1,1,1,4),(0.0311354311261585,
0.968867350391379),(0.2740335216418,0.3186323860176,0.4287267447046,0.5405493543357,
0.6542631421455,0.769753263817,0.8858807480565,0.922150638721103),
 .UNSPECIFIED.)
GEOMETRIC_REPRESENTATION_ITEM()
RATIONAL_B_SPLINE_SURFACE(((1.22401274089182,1.22401274089182,1.22401274089182,
1.22401274089182,1.22401274089182,1.22401274089182,1.22401274089182,1.22401274089182,
1.22401274089182,1.22401274089182),(0.92532820040589,0.92532820040589,0.92532820040589,
0.92532820040589,0.92532820040589,0.92532820040589,0.92532820040589,0.92532820040589,
0.92532820040589,0.92532820040589),(0.925329086372054,0.925329086372054,
0.925329086372054,0.925329086372054,0.925329086372054,0.925329086372054,
0.925329086372054,0.925329086372054,0.925329086372054,0.925329086372054),
(1.22401539879031,1.22401539879031,1.22401539879031,1.22401539879031,1.22401539879031,
1.22401539879031,1.22401539879031,1.22401539879031,1.22401539879031,1.22401539879031)))
REPRESENTATION_ITEM('')
SURFACE()
);
#508=(
BOUNDED_SURFACE()
B_SPLINE_SURFACE(3,3,((#62276,#62277,#62278,#62279,#62280,#62281,#62282,
#62283,#62284,#62285),(#62286,#62287,#62288,#62289,#62290,#62291,#62292,
#62293,#62294,#62295),(#62296,#62297,#62298,#62299,#62300,#62301,#62302,
#62303,#62304,#62305),(#62306,#62307,#62308,#62309,#62310,#62311,#62312,
#62313,#62314,#62315)),.UNSPECIFIED.,.F.,.F.,.F.)
B_SPLINE_SURFACE_WITH_KNOTS((4,4),(4,1,1,1,1,1,1,4),(0.0418834176682723,
0.963270158916865),(0.03308221537874,0.1426814400664,0.2856169940151,0.4287844248845,
0.5720769017456,0.7151865856598,0.857914401801,0.9460833470526),
 .UNSPECIFIED.)
GEOMETRIC_REPRESENTATION_ITEM()
RATIONAL_B_SPLINE_SURFACE(((1.13002825352558,1.13002825352558,1.13002825352558,
1.13002825352558,1.13002825352558,1.13002825352558,1.13002825352558,1.13002825352558,
1.13002825352558,1.13002825352558),(0.955682081384098,0.955682081384098,
0.955682081384098,0.955682081384098,0.955682081384098,0.955682081384098,
0.955682081384098,0.955682081384098,0.955682081384098,0.955682081384098),
(0.95666273389168,0.95666273389168,0.95666273389168,0.95666273389168,0.95666273389168,
0.95666273389168,0.95666273389168,0.95666273389168,0.95666273389168,0.95666273389168),
(1.13297021104833,1.13297021104833,1.13297021104833,1.13297021104833,1.13297021104833,
1.13297021104833,1.13297021104833,1.13297021104833,1.13297021104833,1.13297021104833)))
REPRESENTATION_ITEM('')
SURFACE()
);
#509=(
BOUNDED_SURFACE()
B_SPLINE_SURFACE(3,3,((#62411,#62412,#62413,#62414,#62415,#62416,#62417,
#62418,#62419,#62420),(#62421,#62422,#62423,#62424,#62425,#62426,#62427,
#62428,#62429,#62430),(#62431,#62432,#62433,#62434,#62435,#62436,#62437,
#62438,#62439,#62440),(#62441,#62442,#62443,#62444,#62445,#62446,#62447,
#62448,#62449,#62450)),.UNSPECIFIED.,.F.,.F.,.F.)
B_SPLINE_SURFACE_WITH_KNOTS((4,4),(4,1,1,1,1,1,1,4),(0.0506807378443564,
0.94932028223993),(0.0780685614205442,0.1141112037554,0.2302382189757,0.3457306297879,
0.4594466176023,0.5712706666257,0.681366169875,0.714773732635213),
 .UNSPECIFIED.)
GEOMETRIC_REPRESENTATION_ITEM()
RATIONAL_B_SPLINE_SURFACE(((1.20572543061212,1.20572543061212,1.20572543061212,
1.20572543061212,1.20572543061212,1.20572543061212,1.20572543061212,1.20572543061212,
1.20572543061212,1.20572543061212),(0.931424545091861,0.931424545091861,
0.931424545091861,0.931424545091861,0.931424545091861,0.931424545091861,
0.931424545091861,0.931424545091861,0.931424545091861,0.931424545091861),
(0.931424856462914,0.931424856462914,0.931424856462914,0.931424856462914,
0.931424856462914,0.931424856462914,0.931424856462914,0.931424856462914,
0.931424856462914,0.931424856462914),(1.20572636472528,1.20572636472528,
1.20572636472528,1.20572636472528,1.20572636472528,1.20572636472528,1.20572636472528,
1.20572636472528,1.20572636472528,1.20572636472528)))
REPRESENTATION_ITEM('')
SURFACE()
);
#510=(
BOUNDED_SURFACE()
B_SPLINE_SURFACE(3,3,((#62598,#62599,#62600,#62601,#62602,#62603,#62604,
#62605,#62606,#62607),(#62608,#62609,#62610,#62611,#62612,#62613,#62614,
#62615,#62616,#62617),(#62618,#62619,#62620,#62621,#62622,#62623,#62624,
#62625,#62626,#62627),(#62628,#62629,#62630,#62631,#62632,#62633,#62634,
#62635,#62636,#62637)),.UNSPECIFIED.,.F.,.F.,.F.)
B_SPLINE_SURFACE_WITH_KNOTS((4,4),(4,1,1,1,1,1,1,4),(0.0418856368296952,
0.963268780585969),(0.05391635097625,0.1420855982353,0.2848134143608,0.4279230982548,
0.5712155751054,0.7143830059727,0.8573185599327,0.9669169090934),
 .UNSPECIFIED.)
GEOMETRIC_REPRESENTATION_ITEM()
RATIONAL_B_SPLINE_SURFACE(((1.13002699821861,1.13002699821861,1.13002699821861,
1.13002699821861,1.13002699821861,1.13002699821861,1.13002699821861,1.13002699821861,
1.13002699821861,1.13002699821861),(0.955682345407873,0.955682345407873,
0.955682345407873,0.955682345407873,0.955682345407873,0.955682345407873,
0.955682345407873,0.955682345407873,0.955682345407873,0.955682345407873),
(0.956663154117468,0.956663154117468,0.956663154117468,0.956663154117468,
0.956663154117468,0.956663154117468,0.956663154117468,0.956663154117468,
0.956663154117468,0.956663154117468),(1.13296942434739,1.13296942434739,
1.13296942434739,1.13296942434739,1.13296942434739,1.13296942434739,1.13296942434739,
1.13296942434739,1.13296942434739,1.13296942434739)))
REPRESENTATION_ITEM('')
SURFACE()
);
#511=(
BOUNDED_SURFACE()
B_SPLINE_SURFACE(3,3,((#62791,#62792,#62793,#62794,#62795,#62796),(#62797,
#62798,#62799,#62800,#62801,#62802),(#62803,#62804,#62805,#62806,#62807,
#62808),(#62809,#62810,#62811,#62812,#62813,#62814)),.UNSPECIFIED.,.F.,
 .F.,.F.)
B_SPLINE_SURFACE_WITH_KNOTS((4,4),(4,1,1,4),(0.0606070589512044,0.9394900012978),
(0.199119623412498,0.3331969354622,0.6668030645378,0.800880381046923),
 .UNSPECIFIED.)
GEOMETRIC_REPRESENTATION_ITEM()
RATIONAL_B_SPLINE_SURFACE(((1.17469014882262,1.17469014882262,1.17469014882262,
1.17469014882262,1.17469014882262,1.17469014882262),(0.941744224794448,
0.941744224794448,0.941744224794448,0.941744224794448,0.941744224794448,
0.941744224794448),(0.941769953233938,0.941769953233938,0.941769953233937,
0.941769953233937,0.941769953233937,0.941769953233937),(1.17476733414109,
1.17476733414109,1.17476733414109,1.17476733414109,1.17476733414109,1.17476733414109)))
REPRESENTATION_ITEM('')
SURFACE()
);
#512=(
BOUNDED_SURFACE()
B_SPLINE_SURFACE(3,3,((#63081,#63082,#63083,#63084,#63085,#63086,#63087,
#63088,#63089,#63090,#63091,#63092,#63093,#63094,#63095,#63096,#63097,#63098,
#63099,#63100),(#63101,#63102,#63103,#63104,#63105,#63106,#63107,#63108,
#63109,#63110,#63111,#63112,#63113,#63114,#63115,#63116,#63117,#63118,#63119,
#63120),(#63121,#63122,#63123,#63124,#63125,#63126,#63127,#63128,#63129,
#63130,#63131,#63132,#63133,#63134,#63135,#63136,#63137,#63138,#63139,#63140),
(#63141,#63142,#63143,#63144,#63145,#63146,#63147,#63148,#63149,#63150,
#63151,#63152,#63153,#63154,#63155,#63156,#63157,#63158,#63159,#63160)),
 .UNSPECIFIED.,.F.,.F.,.F.)
B_SPLINE_SURFACE_WITH_KNOTS((4,4),(4,1,1,1,1,1,1,1,1,1,1,1,1,1,1,1,1,4),
(0.0633076409949893,0.939204474105228),(-0.009153831281455,0.,0.07546620931579,
0.1557174957677,0.2403996005821,0.3291522597982,0.4125162510435,0.4856766709034,
0.5506589911205,0.6094498872342,0.6638185572398,0.7128092494438,0.7565100470699,
0.7968460585168,0.8357686456417,0.87488860494,0.9149305605777,0.9275319404913),
 .UNSPECIFIED.)
GEOMETRIC_REPRESENTATION_ITEM()
RATIONAL_B_SPLINE_SURFACE(((1.07645083767944,1.07645083767944,1.07645083767944,
1.07645083767944,1.07645083767944,1.07645083767944,1.07645083767944,1.07645083767944,
1.07645083767944,1.07645083767944,1.07645083767944,1.07645083767944,1.07645083767944,
1.07645083767944,1.07645083767944,1.07645083767944,1.07645083767944,1.07645083767944,
1.07645083767944,1.07645083767944),(0.974223193540317,0.974223193540317,
0.974223193540317,0.974223193540317,0.974223193540317,0.974223193540317,
0.974223193540317,0.974223193540317,0.974223193540317,0.974223193540317,
0.974223193540317,0.974223193540317,0.974223193540317,0.974223193540317,
0.974223193540317,0.974223193540317,0.974223193540317,0.974223193540317,
0.974223193540317,0.974223193540317),(0.974517230753478,0.974517230753478,
0.974517230753478,0.974517230753478,0.974517230753478,0.974517230753478,
0.974517230753478,0.974517230753478,0.974517230753478,0.974517230753478,
0.974517230753478,0.974517230753478,0.974517230753478,0.974517230753478,
0.974517230753478,0.974517230753478,0.974517230753478,0.974517230753478,
0.974517230753478,0.974517230753478),(1.07733294931892,1.07733294931892,
1.07733294931892,1.07733294931892,1.07733294931892,1.07733294931892,1.07733294931892,
1.07733294931892,1.07733294931892,1.07733294931892,1.07733294931892,1.07733294931892,
1.07733294931892,1.07733294931892,1.07733294931892,1.07733294931892,1.07733294931892,
1.07733294931892,1.07733294931892,1.07733294931892)))
REPRESENTATION_ITEM('')
SURFACE()
);
#513=(
BOUNDED_SURFACE()
B_SPLINE_SURFACE(3,3,((#63322,#63323,#63324,#63325,#63326,#63327,#63328,
#63329,#63330,#63331),(#63332,#63333,#63334,#63335,#63336,#63337,#63338,
#63339,#63340,#63341),(#63342,#63343,#63344,#63345,#63346,#63347,#63348,
#63349,#63350,#63351),(#63352,#63353,#63354,#63355,#63356,#63357,#63358,
#63359,#63360,#63361)),.UNSPECIFIED.,.F.,.F.,.F.)
B_SPLINE_SURFACE_WITH_KNOTS((4,4),(4,1,1,1,1,1,1,4),(0.0543118686704758,
0.946617716449823),(0.289640600847592,0.3185583158377,0.428651361796,0.5404783317088,
0.654204063309,0.7697110119304,0.8858550830104,0.922057258249154),
 .UNSPECIFIED.)
GEOMETRIC_REPRESENTATION_ITEM()
RATIONAL_B_SPLINE_SURFACE(((1.20241792264148,1.20241792264148,1.20241792264148,
1.20241792264148,1.20241792264148,1.20241792264148,1.20241792264148,1.20241792264148,
1.20241792264148,1.20241792264148),(0.932245899692698,0.932245899692698,
0.932245899692698,0.932245899692698,0.932245899692698,0.932245899692698,
0.932245899692698,0.932245899692698,0.932245899692698,0.932245899692698),
(0.932527652643697,0.932527652643697,0.932527652643697,0.932527652643697,
0.932527652643697,0.932527652643697,0.932527652643697,0.932527652643697,
0.932527652643697,0.932527652643697),(1.20326318149447,1.20326318149447,
1.20326318149447,1.20326318149447,1.20326318149447,1.20326318149447,1.20326318149447,
1.20326318149447,1.20326318149447,1.20326318149447)))
REPRESENTATION_ITEM('')
SURFACE()
);
#514=(
BOUNDED_SURFACE()
B_SPLINE_SURFACE(3,3,((#63475,#63476,#63477,#63478,#63479,#63480,#63481,
#63482,#63483,#63484,#63485),(#63486,#63487,#63488,#63489,#63490,#63491,
#63492,#63493,#63494,#63495,#63496),(#63497,#63498,#63499,#63500,#63501,
#63502,#63503,#63504,#63505,#63506,#63507),(#63508,#63509,#63510,#63511,
#63512,#63513,#63514,#63515,#63516,#63517,#63518)),.UNSPECIFIED.,.F.,.F.,
 .F.)
B_SPLINE_SURFACE_WITH_KNOTS((4,4),(4,1,1,1,1,1,1,1,4),(0.0595203863462284,
0.938436205671232),(0.05105962729005,0.1243084941807,0.2492353165502,0.3744835129416,
0.4998949769261,0.6253220276845,0.7506164023093,0.8756120170229,0.9160299525996),
 .UNSPECIFIED.)
GEOMETRIC_REPRESENTATION_ITEM()
RATIONAL_B_SPLINE_SURFACE(((1.11958055537369,1.11958055537369,1.11958055537369,
1.11958055537369,1.11958055537369,1.11958055537369,1.11958055537369,1.11958055537369,
1.11958055537369,1.11958055537369,1.11958055537369),(0.96050964184567,0.96050964184567,
0.96050964184567,0.96050964184567,0.96050964184567,0.96050964184567,0.96050964184567,
0.96050964184567,0.96050964184567,0.96050964184567,0.96050964184567),(0.960140672698838,
0.960140672698838,0.960140672698838,0.960140672698838,0.960140672698838,
0.960140672698838,0.960140672698838,0.960140672698838,0.960140672698838,
0.960140672698838,0.960140672698838),(1.1184736479332,1.1184736479332,1.1184736479332,
1.1184736479332,1.1184736479332,1.1184736479332,1.1184736479332,1.1184736479332,
1.1184736479332,1.1184736479332,1.1184736479332)))
REPRESENTATION_ITEM('')
SURFACE()
);
#515=(
BOUNDED_SURFACE()
B_SPLINE_SURFACE(3,3,((#63752,#63753,#63754,#63755,#63756,#63757,#63758,
#63759,#63760,#63761),(#63762,#63763,#63764,#63765,#63766,#63767,#63768,
#63769,#63770,#63771),(#63772,#63773,#63774,#63775,#63776,#63777,#63778,
#63779,#63780,#63781),(#63782,#63783,#63784,#63785,#63786,#63787,#63788,
#63789,#63790,#63791)),.UNSPECIFIED.,.F.,.F.,.F.)
B_SPLINE_SURFACE_WITH_KNOTS((4,4),(4,1,1,1,1,1,1,4),(0.0567016135390075,
0.965170855368738),(0.2246119235744,0.2652891204936,0.3542346581807,0.4509283928036,
0.5489344914255,0.6456463447232,0.7346252853759,0.7753865663254),
 .UNSPECIFIED.)
GEOMETRIC_REPRESENTATION_ITEM()
RATIONAL_B_SPLINE_SURFACE(((1.20024622089112,1.20024622089112,1.20024622089112,
1.20024622089112,1.20024622089112,1.20024622089112,1.20024622089112,1.20024622089112,
1.20024622089112,1.20024622089112),(0.926664455909577,0.926664455909577,
0.926664455909577,0.926664455909577,0.926664455909577,0.926664455909577,
0.926664455909577,0.926664455909577,0.926664455909577,0.926664455909577),
(0.933413757092531,0.933413757092531,0.933413757092531,0.933413757092531,
0.933413757092531,0.933413757092531,0.933413757092531,0.933413757092531,
0.933413757092531,0.933413757092531),(1.22049412443998,1.22049412443998,
1.22049412443998,1.22049412443998,1.22049412443998,1.22049412443998,1.22049412443998,
1.22049412443998,1.22049412443998,1.22049412443998)))
REPRESENTATION_ITEM('')
SURFACE()
);
#516=(
BOUNDED_SURFACE()
B_SPLINE_SURFACE(2,2,((#63877,#63878,#63879),(#63880,#63881,#63882),(#63883,
#63884,#63885)),.UNSPECIFIED.,.F.,.F.,.F.)
B_SPLINE_SURFACE_WITH_KNOTS((3,3),(3,3),(-0.316361998869524,0.316361961333282),
(0.571031091629656,0.999765088357377),.UNSPECIFIED.)
GEOMETRIC_REPRESENTATION_ITEM()
RATIONAL_B_SPLINE_SURFACE(((1.,0.977111247736172,1.),(0.950373533316957,
0.928620668954766,0.950373533316957),(1.,0.977111247736172,1.)))
REPRESENTATION_ITEM('')
SURFACE()
);
#517=(
BOUNDED_SURFACE()
B_SPLINE_SURFACE(2,2,((#63888,#63889,#63890),(#63891,#63892,#63893),(#63894,
#63895,#63896)),.UNSPECIFIED.,.F.,.F.,.F.)
B_SPLINE_SURFACE_WITH_KNOTS((3,3),(3,3),(-0.316362027618547,0.316362033179937),
(1.35642916480867,1.78516363636164),.UNSPECIFIED.)
GEOMETRIC_REPRESENTATION_ITEM()
RATIONAL_B_SPLINE_SURFACE(((1.,0.977111197231604,1.),(0.950373517668733,
0.928620605666507,0.950373517668733),(1.,0.977111197231604,1.)))
REPRESENTATION_ITEM('')
SURFACE()
);
#518=(
BOUNDED_SURFACE()
B_SPLINE_SURFACE(2,2,((#63899,#63900,#63901),(#63902,#63903,#63904),(#63905,
#63906,#63907)),.UNSPECIFIED.,.F.,.F.,.F.)
B_SPLINE_SURFACE_WITH_KNOTS((3,3),(3,3),(-0.31636199673171,0.316361977977988),
(2.14182744740588,2.57056168331331),.UNSPECIFIED.)
GEOMETRIC_REPRESENTATION_ITEM()
RATIONAL_B_SPLINE_SURFACE(((1.,0.97711122229594,1.),(0.950373531060328,
0.928620642572066,0.950373531060328),(1.,0.97711122229594,1.)))
REPRESENTATION_ITEM('')
SURFACE()
);
#519=(
BOUNDED_SURFACE()
B_SPLINE_SURFACE(2,2,((#63910,#63911,#63912),(#63913,#63914,#63915),(#63916,
#63917,#63918)),.UNSPECIFIED.,.F.,.F.,.F.)
B_SPLINE_SURFACE_WITH_KNOTS((3,3),(3,3),(-0.316362001159797,0.316362001025874),
(-0.214366972691254,0.214366972691255),.UNSPECIFIED.)
GEOMETRIC_REPRESENTATION_ITEM()
RATIONAL_B_SPLINE_SURFACE(((1.,0.977111253197478,1.),(0.950373526786289,
0.928620667763857,0.950373526786289),(1.,0.977111253197478,1.)))
REPRESENTATION_ITEM('')
SURFACE()
);
#520=(
BOUNDED_SURFACE()
B_SPLINE_SURFACE(2,2,((#63921,#63922,#63923),(#63924,#63925,#63926),(#63927,
#63928,#63929)),.UNSPECIFIED.,.F.,.F.,.F.)
B_SPLINE_SURFACE_WITH_KNOTS((3,3),(3,3),(-0.316362027572333,0.316361999994803),
(-2.57055983293518,-2.14182718056046),.UNSPECIFIED.)
GEOMETRIC_REPRESENTATION_ITEM()
RATIONAL_B_SPLINE_SURFACE(((1.,0.977111390727357,1.),(0.950373522838055,
0.928620794610749,0.950373522838055),(1.,0.977111390727357,1.)))
REPRESENTATION_ITEM('')
SURFACE()
);
#521=(
BOUNDED_SURFACE()
B_SPLINE_SURFACE(2,2,((#63932,#63933,#63934),(#63935,#63936,#63937),(#63938,
#63939,#63940)),.UNSPECIFIED.,.F.,.F.,.F.)
B_SPLINE_SURFACE_WITH_KNOTS((3,3),(3,3),(-0.316361976307064,0.316361980987301),
(-1.78516344737183,-1.35642909114174),.UNSPECIFIED.)
GEOMETRIC_REPRESENTATION_ITEM()
RATIONAL_B_SPLINE_SURFACE(((1.,0.977111209497874,1.),(0.950373533769378,
0.928620633056165,0.950373533769378),(1.,0.977111209497874,1.)))
REPRESENTATION_ITEM('')
SURFACE()
);
#522=(
BOUNDED_SURFACE()
B_SPLINE_SURFACE(2,2,((#63943,#63944,#63945),(#63946,#63947,#63948),(#63949,
#63950,#63951)),.UNSPECIFIED.,.F.,.F.,.F.)
B_SPLINE_SURFACE_WITH_KNOTS((3,3),(3,3),(-0.316361997381232,0.316362033180092),
(-0.999765325442169,-0.571033470390333),.UNSPECIFIED.)
GEOMETRIC_REPRESENTATION_ITEM()
RATIONAL_B_SPLINE_SURFACE(((1.,0.977111475533851,1.),(0.950373522372293,
0.928620874753495,0.950373522372293),(1.,0.977111475533851,1.)))
REPRESENTATION_ITEM('')
SURFACE()
);
#523=(
BOUNDED_SURFACE()
B_SPLINE_SURFACE(2,2,((#63954,#63955,#63956),(#63957,#63958,#63959),(#63960,
#63961,#63962)),.UNSPECIFIED.,.F.,.F.,.F.)
B_SPLINE_SURFACE_WITH_KNOTS((3,3),(3,3),(-0.316361967725758,0.316361973128478),
(-0.2143652338984,0.214367145981156),.UNSPECIFIED.)
GEOMETRIC_REPRESENTATION_ITEM()
RATIONAL_B_SPLINE_SURFACE(((1.,0.977111419711065,1.),(0.950373536326736,
0.928620835336042,0.950373536326736),(1.,0.977111419711065,1.)))
REPRESENTATION_ITEM('')
SURFACE()
);
#524=CONICAL_SURFACE('',#26602,2.5,1.02974425867665);
#525=CONICAL_SURFACE('',#26603,2.5,1.02974425867665);
#526=CONICAL_SURFACE('',#26629,2.5,1.02974425867665);
#527=CONICAL_SURFACE('',#26630,2.5,1.02974425867665);
#528=CONICAL_SURFACE('',#27199,2.5,0.371257902576146);
#529=CONICAL_SURFACE('',#27203,4.00000000000001,1.04719755119661);
#530=CONICAL_SURFACE('',#27205,3.46410161513776,1.0471975511966);
#531=CONICAL_SURFACE('',#27247,3.46410161513776,1.0471975511966);
#532=CONICAL_SURFACE('',#27248,3.46410161513776,1.0471975511966);
#533=CONICAL_SURFACE('',#27249,3.46410161513776,1.0471975511966);
#534=CONICAL_SURFACE('',#27250,3.46410161513776,1.0471975511966);
#535=CONICAL_SURFACE('',#27251,3.46410161513776,1.0471975511966);
#536=CONICAL_SURFACE('',#27252,4.00000000000001,1.04719755119661);
#537=CONICAL_SURFACE('',#27253,4.00000000000001,1.04719755119661);
#538=CONICAL_SURFACE('',#27254,4.00000000000001,1.04719755119661);
#539=CONICAL_SURFACE('',#27255,4.00000000000001,1.04719755119661);
#540=CONICAL_SURFACE('',#27256,4.00000000000001,1.04719755119661);
#541=CONICAL_SURFACE('',#27283,7.00000000000019,0.785398163397415);
#542=CONICAL_SURFACE('',#27291,9.00000000000005,0.785398163397447);
#543=CONICAL_SURFACE('',#27297,9.9999999999999,0.785398163397382);
#544=CONICAL_SURFACE('',#27312,7.5,0.785398163397448);
#545=CONICAL_SURFACE('',#27319,5.00000000000007,0.785398163397425);
#546=CONICAL_SURFACE('',#27603,1.,1.02974425867665);
#547=CONICAL_SURFACE('',#27612,2.,0.785398163397443);
#548=CONICAL_SURFACE('',#27613,1.25,0.785398163397442);
#549=CONICAL_SURFACE('',#27618,6.9585,0.78539816339745);
#550=CONICAL_SURFACE('',#27622,7.5,0.785398163397448);
#551=CONICAL_SURFACE('',#27976,2.693275,0.785398163397448);
#552=CONICAL_SURFACE('',#27998,2.693275,0.785398163397448);
#553=CONICAL_SURFACE('',#28005,26.75,0.785398163397448);
#554=CONICAL_SURFACE('',#28068,26.75,0.785398163397448);
#555=CONICAL_SURFACE('',#28241,2.693275,0.785398163397448);
#556=CONICAL_SURFACE('',#28263,2.693275,0.785398163397448);
#557=CONICAL_SURFACE('',#28270,26.75,0.785398163397448);
#558=CONICAL_SURFACE('',#28333,26.75,0.785398163397448);
#559=CONICAL_SURFACE('',#28483,2.5,1.02974425867665);
#560=CONICAL_SURFACE('',#28487,2.5,1.02974425867665);
#561=CONICAL_SURFACE('',#28491,2.5,1.02974425867665);
#562=CONICAL_SURFACE('',#28495,2.5,1.02974425867665);
#563=CONICAL_SURFACE('',#28499,2.5,1.02974425867665);
#564=CONICAL_SURFACE('',#28503,2.5,1.02974425867665);
#565=CONICAL_SURFACE('',#28507,2.5,1.02974425867665);
#566=CONICAL_SURFACE('',#28511,2.5,1.02974425867665);
#567=CONICAL_SURFACE('',#28515,2.5,1.02974425867665);
#568=CONICAL_SURFACE('',#28519,2.5,1.02974425867665);
#569=CONICAL_SURFACE('',#28523,2.5,1.02974425867665);
#570=CONICAL_SURFACE('',#28527,2.5,1.02974425867665);
#571=CONICAL_SURFACE('',#28531,2.5,1.02974425867665);
#572=CONICAL_SURFACE('',#28535,2.5,1.02974425867665);
#573=CONICAL_SURFACE('',#28539,2.5,1.02974425867665);
#574=CONICAL_SURFACE('',#28543,2.5,1.02974425867665);
#575=CONICAL_SURFACE('',#28547,2.5,1.02974425867665);
#576=CONICAL_SURFACE('',#28568,5.,0.785398163397445);
#577=CONICAL_SURFACE('',#28570,2.4585,0.785398163397448);
#578=CONICAL_SURFACE('',#28587,3.75,0.785398163397444);
#579=CONICAL_SURFACE('',#28591,1664.2794823505,1.02974425867665);
#580=CONICAL_SURFACE('',#28684,5.,0.785398163397451);
#581=CONICAL_SURFACE('',#28686,2.4585,0.785398163397442);
#582=ELLIPSE('',#26235,4.94974735819038,3.49999990182558);
#583=ELLIPSE('',#26237,4.94974766602105,3.5000001764392);
#584=ELLIPSE('',#26241,4.94974746762207,3.49999999945822);
#585=ELLIPSE('',#26243,4.94974743837769,3.49999997319395);
#586=ELLIPSE('',#26249,4.94974746471116,3.49999999781732);
#587=ELLIPSE('',#26251,4.94974761521235,3.50000013143823);
#588=ELLIPSE('',#26255,4.94974751536128,3.5000000426592);
#589=ELLIPSE('',#26257,4.94974734791332,3.49999989298097);
#590=ELLIPSE('',#26263,4.94974738455087,3.49999992654364);
#591=ELLIPSE('',#26265,4.94974756609828,3.50000008750549);
#592=ELLIPSE('',#26269,4.94974748465299,3.50000001559145);
#593=ELLIPSE('',#26271,4.9497474078675,3.49999994629514);
#594=ELLIPSE('',#26277,4.9497473461591,3.49999989191482);
#595=ELLIPSE('',#26279,4.94974750610666,3.50000003412937);
#596=ELLIPSE('',#26283,4.94974748783974,3.50000001743086);
#597=ELLIPSE('',#26285,4.94974744634947,3.49999998103439);
#598=ELLIPSE('',#26291,4.94974749695506,3.50000002579411);
#599=ELLIPSE('',#26293,4.94974750752024,3.50000003493957);
#600=ELLIPSE('',#26297,4.94974751315491,3.50000003982775);
#601=ELLIPSE('',#26299,4.949747463355,3.4999999955299);
#602=ELLIPSE('',#26305,4.94974749836308,3.50000002653739);
#603=ELLIPSE('',#26307,4.94974757675016,3.50000009672614);
#604=ELLIPSE('',#26311,4.94974748001691,3.50000000973653);
#605=ELLIPSE('',#26313,4.94974739716868,3.49999993702713);
#606=ELLIPSE('',#26319,4.94974749924226,3.5000000270794);
#607=ELLIPSE('',#26321,4.94974743684973,3.49999997233704);
#608=ELLIPSE('',#26325,4.9497475382208,3.50000006223073);
#609=ELLIPSE('',#26327,4.94974747235583,3.5000000037591);
#610=ELLIPSE('',#26333,4.94974748843076,3.5000000176963);
#611=ELLIPSE('',#26335,4.94974741762146,3.49999995499458);
#612=ELLIPSE('',#26339,4.94974749231943,3.50000002155544);
#613=ELLIPSE('',#26341,4.94974745849775,3.49999999105758);
#614=ELLIPSE('',#26347,4.94974743835813,3.49999997320228);
#615=ELLIPSE('',#26349,4.94974746762365,3.49999999944211);
#616=ELLIPSE('',#26353,4.94974749229401,3.50000002151707);
#617=ELLIPSE('',#26355,4.9497474430954,3.4999999775075);
#618=ELLIPSE('',#26361,4.94974746457826,3.49999999694589);
#619=ELLIPSE('',#26363,4.94974746001076,3.49999999272877);
#620=ELLIPSE('',#26367,4.94974748578252,3.50000001541321);
#621=ELLIPSE('',#26369,4.94974746533883,3.49999999735002);
#622=ELLIPSE('',#26375,4.94974749254742,3.50000002161139);
#623=ELLIPSE('',#26377,4.94974746567926,3.49999999752504);
#624=ELLIPSE('',#26381,4.94974748072687,3.50000001091353);
#625=ELLIPSE('',#26383,4.94974746232603,3.49999999483898);
#626=ELLIPSE('',#26389,4.94974748208041,3.50000001242701);
#627=ELLIPSE('',#26391,4.94974745070612,3.49999998421949);
#628=ELLIPSE('',#26395,4.94974745801903,3.49999999076925);
#629=ELLIPSE('',#26397,4.94974746302533,3.49999999523587);
#630=ELLIPSE('',#26403,4.94974746046047,3.49999999301059);
#631=ELLIPSE('',#26405,4.94974745907472,3.49999999180994);
#632=ELLIPSE('',#26409,4.94974747036828,3.50000000182558);
#633=ELLIPSE('',#26411,4.9497474701889,3.50000000171811);
#634=ELLIPSE('',#26417,4.94974746606674,3.49999999798426);
#635=ELLIPSE('',#26419,4.94974746678755,3.49999999861078);
#636=ELLIPSE('',#26423,4.94974746786117,3.49999999962962);
#637=ELLIPSE('',#26425,4.9497474685907,3.50000000019107);
#638=ELLIPSE('',#26431,4.94974746853076,3.50000000020001);
#639=ELLIPSE('',#26433,4.94974746847046,3.50000000014575);
#640=ELLIPSE('',#26437,4.9497474687332,3.50000000037123);
#641=ELLIPSE('',#26439,4.94974746865778,3.50000000030521);
#642=ELLIPSE('',#26643,6.97960018289555,5.49999999999817);
#643=ELLIPSE('',#26645,6.97960018289945,5.50000000000025);
#644=ELLIPSE('',#26646,6.97960018289465,5.49999999999756);
#645=ELLIPSE('',#26648,6.97960018289959,5.50000000000032);
#646=ELLIPSE('',#26649,6.97960018289765,5.49999999999922);
#647=ELLIPSE('',#26651,6.9796001828989,5.49999999999987);
#648=ELLIPSE('',#26972,21.2503681783598,5.50000000000001);
#649=ELLIPSE('',#26973,21.2503681783597,5.5);
#650=ELLIPSE('',#26978,21.2503681783597,5.5);
#651=ELLIPSE('',#26983,21.2503681783597,5.5);
#652=ELLIPSE('',#26985,21.2503681783597,5.49999999999999);
#653=ELLIPSE('',#26986,21.2503681783597,5.5);
#654=ELLIPSE('',#27079,21.2503681783598,5.50000000000001);
#655=ELLIPSE('',#27081,21.2503681783597,5.49999999999999);
#656=ELLIPSE('',#27086,6.97960018290351,5.50000000000224);
#657=ELLIPSE('',#27091,6.97960018290198,5.50000000000146);
#658=ELLIPSE('',#28121,54.9999999419771,27.4999999445285);
#659=ELLIPSE('',#28122,55.000000033545,27.5000000336033);
#660=ELLIPSE('',#28123,54.9999999899496,27.4999999902495);
#661=ELLIPSE('',#28124,55.0000000182334,27.5000000177256);
#662=ELLIPSE('',#28125,32.156845610475,27.5);
#663=ELLIPSE('',#28131,33.1709935839343,27.5);
#664=ELLIPSE('',#28132,55.0000000634487,27.5000000626689);
#665=ELLIPSE('',#28133,54.9999999927228,27.4999999930211);
#666=ELLIPSE('',#28134,54.9999999529142,27.4999999544911);
#667=ELLIPSE('',#28135,54.999999883306,27.4999998869508);
#668=ELLIPSE('',#28150,31.5721756903194,27.);
#669=ELLIPSE('',#28153,31.5721756902846,27.);
#670=ELLIPSE('',#28166,32.567884609681,27.);
#671=ELLIPSE('',#28169,54.0000000152791,27.00000001486);
#672=ELLIPSE('',#28170,53.9999998552686,26.9999998599516);
#673=ELLIPSE('',#28171,53.9999996954935,26.9999997042733);
#674=ELLIPSE('',#28172,54.0000000102257,27.0000000099676);
#675=ELLIPSE('',#28181,54.0000000020546,27.0000000020822);
#676=ELLIPSE('',#28183,53.9999999941722,26.9999999944392);
#677=ELLIPSE('',#28186,54.0000000784931,27.0000000775048);
#678=ELLIPSE('',#28188,54.0000000505798,27.0000000505259);
#679=ELLIPSE('',#28381,55.0000000336669,27.5000000339144);
#680=ELLIPSE('',#28382,55.0000002451225,27.5000002404132);
#681=ELLIPSE('',#28383,54.9999999054554,27.4999999087398);
#682=ELLIPSE('',#28384,54.9999999692227,27.4999999704721);
#683=ELLIPSE('',#28385,32.156845610475,27.5);
#684=ELLIPSE('',#28391,33.1709935839343,27.5);
#685=ELLIPSE('',#28392,55.0000000340055,27.5000000342412);
#686=ELLIPSE('',#28393,54.9999999479979,27.4999999499152);
#687=ELLIPSE('',#28394,54.99999995367,27.4999999554067);
#688=ELLIPSE('',#28395,55.0000002756688,27.5000002701183);
#689=ELLIPSE('',#28410,31.5721756903194,27.);
#690=ELLIPSE('',#28413,31.5721756902845,27.);
#691=ELLIPSE('',#28426,32.5678846096809,27.);
#692=ELLIPSE('',#28429,54.0000000112232,27.0000000109264);
#693=ELLIPSE('',#28430,54.00000012479,27.0000001227984);
#694=ELLIPSE('',#28431,53.999999886139,26.9999998900941);
#695=ELLIPSE('',#28432,53.9999999927924,26.9999999931258);
#696=ELLIPSE('',#28441,53.9999999968904,26.9999999970926);
#697=ELLIPSE('',#28443,53.9999999996556,26.9999999997697);
#698=ELLIPSE('',#28446,53.9999999562436,26.9999999583659);
#699=ELLIPSE('',#28448,53.9999995905245,26.999999602125);
#700=ITEM_DEFINED_TRANSFORMATION($,$,#26142,#26201);
#701=ITEM_DEFINED_TRANSFORMATION($,$,#26176,#26202);
#702=ITEM_DEFINED_TRANSFORMATION($,$,#26229,#27264);
#703=ITEM_DEFINED_TRANSFORMATION($,$,#26592,#27265);
#704=ITEM_DEFINED_TRANSFORMATION($,$,#27192,#27266);
#705=ITEM_DEFINED_TRANSFORMATION($,$,#26592,#27267);
#706=ITEM_DEFINED_TRANSFORMATION($,$,#27192,#27268);
#707=ITEM_DEFINED_TRANSFORMATION($,$,#26229,#27269);
#708=ITEM_DEFINED_TRANSFORMATION($,$,#26592,#27270);
#709=ITEM_DEFINED_TRANSFORMATION($,$,#27192,#27271);
#710=ITEM_DEFINED_TRANSFORMATION($,$,#26592,#27272);
#711=ITEM_DEFINED_TRANSFORMATION($,$,#27192,#27273);
#712=ITEM_DEFINED_TRANSFORMATION($,$,#27275,#27392);
#713=ITEM_DEFINED_TRANSFORMATION($,$,#27328,#27393);
#714=ITEM_DEFINED_TRANSFORMATION($,$,#27395,#27468);
#715=ITEM_DEFINED_TRANSFORMATION($,$,#27435,#27469);
#716=ITEM_DEFINED_TRANSFORMATION($,$,#27471,#27677);
#717=ITEM_DEFINED_TRANSFORMATION($,$,#27668,#27678);
#718=ITEM_DEFINED_TRANSFORMATION($,$,#27602,#27679);
#719=ITEM_DEFINED_TRANSFORMATION($,$,#27668,#27680);
#720=ITEM_DEFINED_TRANSFORMATION($,$,#27714,#28469);
#721=ITEM_DEFINED_TRANSFORMATION($,$,#27944,#28470);
#722=ITEM_DEFINED_TRANSFORMATION($,$,#27957,#28471);
#723=ITEM_DEFINED_TRANSFORMATION($,$,#27979,#28472);
#724=ITEM_DEFINED_TRANSFORMATION($,$,#28001,#28473);
#725=ITEM_DEFINED_TRANSFORMATION($,$,#28209,#28474);
#726=ITEM_DEFINED_TRANSFORMATION($,$,#28222,#28475);
#727=ITEM_DEFINED_TRANSFORMATION($,$,#28244,#28476);
#728=ITEM_DEFINED_TRANSFORMATION($,$,#28266,#28477);
#729=ITEM_DEFINED_TRANSFORMATION($,$,#27713,#28478);
#730=ITEM_DEFINED_TRANSFORMATION($,$,#26042,#28702);
#731=ITEM_DEFINED_TRANSFORMATION($,$,#28479,#28703);
#732=ITEM_DEFINED_TRANSFORMATION($,$,#26069,#28704);
#733=ITEM_DEFINED_TRANSFORMATION($,$,#26070,#28705);
#734=ITEM_DEFINED_TRANSFORMATION($,$,#26095,#28706);
#735=ITEM_DEFINED_TRANSFORMATION($,$,#26141,#28707);
#736=ITEM_DEFINED_TRANSFORMATION($,$,#26203,#28708);
#737=ITEM_DEFINED_TRANSFORMATION($,$,#26228,#28709);
#738=ITEM_DEFINED_TRANSFORMATION($,$,#28586,#28710);
#739=ITEM_DEFINED_TRANSFORMATION($,$,#28680,#28711);
#740=ITEM_DEFINED_TRANSFORMATION($,$,#27274,#28712);
#741=ITEM_DEFINED_TRANSFORMATION($,$,#27394,#28713);
#742=ITEM_DEFINED_TRANSFORMATION($,$,#27470,#28714);
#743=ITEM_DEFINED_TRANSFORMATION($,$,#27681,#28715);
#744=ITEM_DEFINED_TRANSFORMATION($,$,#27712,#28716);
#745=ITEM_DEFINED_TRANSFORMATION($,$,#28641,#28717);
#746=ITEM_DEFINED_TRANSFORMATION($,$,#28564,#28718);
#747=ITEM_DEFINED_TRANSFORMATION($,$,#28479,#28719);
#748=ITEM_DEFINED_TRANSFORMATION($,$,#28586,#28720);
#749=ITEM_DEFINED_TRANSFORMATION($,$,#28586,#28721);
#750=ITEM_DEFINED_TRANSFORMATION($,$,#28680,#28722);
#751=ITEM_DEFINED_TRANSFORMATION($,$,#28680,#28723);
#752=ITEM_DEFINED_TRANSFORMATION($,$,#28680,#28724);
#753=ITEM_DEFINED_TRANSFORMATION($,$,#28680,#28725);
#754=ITEM_DEFINED_TRANSFORMATION($,$,#28680,#28726);
#755=ITEM_DEFINED_TRANSFORMATION($,$,#28680,#28727);
#756=ITEM_DEFINED_TRANSFORMATION($,$,#28680,#28728);
#757=ITEM_DEFINED_TRANSFORMATION($,$,#28680,#28729);
#758=ITEM_DEFINED_TRANSFORMATION($,$,#28680,#28730);
#759=ITEM_DEFINED_TRANSFORMATION($,$,#28680,#28731);
#760=ITEM_DEFINED_TRANSFORMATION($,$,#28680,#28732);
#761=ITEM_DEFINED_TRANSFORMATION($,$,#28680,#28733);
#762=ITEM_DEFINED_TRANSFORMATION($,$,#28680,#28734);
#763=ITEM_DEFINED_TRANSFORMATION($,$,#28680,#28735);
#764=ITEM_DEFINED_TRANSFORMATION($,$,#28680,#28736);
#765=ITEM_DEFINED_TRANSFORMATION($,$,#28680,#28737);
#766=ITEM_DEFINED_TRANSFORMATION($,$,#28680,#28738);
#767=ITEM_DEFINED_TRANSFORMATION($,$,#28680,#28739);
#768=ITEM_DEFINED_TRANSFORMATION($,$,#28680,#28740);
#769=ITEM_DEFINED_TRANSFORMATION($,$,#28680,#28741);
#770=ITEM_DEFINED_TRANSFORMATION($,$,#28680,#28742);
#771=ITEM_DEFINED_TRANSFORMATION($,$,#28680,#28743);
#772=ITEM_DEFINED_TRANSFORMATION($,$,#28564,#28744);
#773=ITEM_DEFINED_TRANSFORMATION($,$,#28586,#28745);
#774=ITEM_DEFINED_TRANSFORMATION($,$,#28586,#28746);
#775=ITEM_DEFINED_TRANSFORMATION($,$,#28586,#28747);
#776=ITEM_DEFINED_TRANSFORMATION($,$,#28680,#28748);
#777=ITEM_DEFINED_TRANSFORMATION($,$,#28641,#28749);
#778=ITEM_DEFINED_TRANSFORMATION($,$,#28680,#28750);
#779=ITEM_DEFINED_TRANSFORMATION($,$,#28680,#28751);
#780=ITEM_DEFINED_TRANSFORMATION($,$,#28680,#28752);
#781=ITEM_DEFINED_TRANSFORMATION($,$,#28680,#28753);
#782=ITEM_DEFINED_TRANSFORMATION($,$,#28680,#28754);
#783=ITEM_DEFINED_TRANSFORMATION($,$,#28680,#28755);
#784=(
REPRESENTATION_RELATIONSHIP($,$,#66896,#66895)
REPRESENTATION_RELATIONSHIP_WITH_TRANSFORMATION(#700)
SHAPE_REPRESENTATION_RELATIONSHIP()
);
#785=(
REPRESENTATION_RELATIONSHIP($,$,#66897,#66895)
REPRESENTATION_RELATIONSHIP_WITH_TRANSFORMATION(#701)
SHAPE_REPRESENTATION_RELATIONSHIP()
);
#786=(
REPRESENTATION_RELATIONSHIP($,$,#66900,#66892)
REPRESENTATION_RELATIONSHIP_WITH_TRANSFORMATION(#702)
SHAPE_REPRESENTATION_RELATIONSHIP()
);
#787=(
REPRESENTATION_RELATIONSHIP($,$,#66901,#66892)
REPRESENTATION_RELATIONSHIP_WITH_TRANSFORMATION(#703)
SHAPE_REPRESENTATION_RELATIONSHIP()
);
#788=(
REPRESENTATION_RELATIONSHIP($,$,#66902,#66892)
REPRESENTATION_RELATIONSHIP_WITH_TRANSFORMATION(#704)
SHAPE_REPRESENTATION_RELATIONSHIP()
);
#789=(
REPRESENTATION_RELATIONSHIP($,$,#66901,#66892)
REPRESENTATION_RELATIONSHIP_WITH_TRANSFORMATION(#705)
SHAPE_REPRESENTATION_RELATIONSHIP()
);
#790=(
REPRESENTATION_RELATIONSHIP($,$,#66902,#66892)
REPRESENTATION_RELATIONSHIP_WITH_TRANSFORMATION(#706)
SHAPE_REPRESENTATION_RELATIONSHIP()
);
#791=(
REPRESENTATION_RELATIONSHIP($,$,#66900,#66899)
REPRESENTATION_RELATIONSHIP_WITH_TRANSFORMATION(#707)
SHAPE_REPRESENTATION_RELATIONSHIP()
);
#792=(
REPRESENTATION_RELATIONSHIP($,$,#66901,#66899)
REPRESENTATION_RELATIONSHIP_WITH_TRANSFORMATION(#708)
SHAPE_REPRESENTATION_RELATIONSHIP()
);
#793=(
REPRESENTATION_RELATIONSHIP($,$,#66902,#66899)
REPRESENTATION_RELATIONSHIP_WITH_TRANSFORMATION(#709)
SHAPE_REPRESENTATION_RELATIONSHIP()
);
#794=(
REPRESENTATION_RELATIONSHIP($,$,#66901,#66899)
REPRESENTATION_RELATIONSHIP_WITH_TRANSFORMATION(#710)
SHAPE_REPRESENTATION_RELATIONSHIP()
);
#795=(
REPRESENTATION_RELATIONSHIP($,$,#66902,#66899)
REPRESENTATION_RELATIONSHIP_WITH_TRANSFORMATION(#711)
SHAPE_REPRESENTATION_RELATIONSHIP()
);
#796=(
REPRESENTATION_RELATIONSHIP($,$,#66904,#66903)
REPRESENTATION_RELATIONSHIP_WITH_TRANSFORMATION(#712)
SHAPE_REPRESENTATION_RELATIONSHIP()
);
#797=(
REPRESENTATION_RELATIONSHIP($,$,#66905,#66903)
REPRESENTATION_RELATIONSHIP_WITH_TRANSFORMATION(#713)
SHAPE_REPRESENTATION_RELATIONSHIP()
);
#798=(
REPRESENTATION_RELATIONSHIP($,$,#66907,#66906)
REPRESENTATION_RELATIONSHIP_WITH_TRANSFORMATION(#714)
SHAPE_REPRESENTATION_RELATIONSHIP()
);
#799=(
REPRESENTATION_RELATIONSHIP($,$,#66908,#66906)
REPRESENTATION_RELATIONSHIP_WITH_TRANSFORMATION(#715)
SHAPE_REPRESENTATION_RELATIONSHIP()
);
#800=(
REPRESENTATION_RELATIONSHIP($,$,#66910,#66909)
REPRESENTATION_RELATIONSHIP_WITH_TRANSFORMATION(#716)
SHAPE_REPRESENTATION_RELATIONSHIP()
);
#801=(
REPRESENTATION_RELATIONSHIP($,$,#66912,#66909)
REPRESENTATION_RELATIONSHIP_WITH_TRANSFORMATION(#717)
SHAPE_REPRESENTATION_RELATIONSHIP()
);
#802=(
REPRESENTATION_RELATIONSHIP($,$,#66911,#66909)
REPRESENTATION_RELATIONSHIP_WITH_TRANSFORMATION(#718)
SHAPE_REPRESENTATION_RELATIONSHIP()
);
#803=(
REPRESENTATION_RELATIONSHIP($,$,#66912,#66909)
REPRESENTATION_RELATIONSHIP_WITH_TRANSFORMATION(#719)
SHAPE_REPRESENTATION_RELATIONSHIP()
);
#804=(
REPRESENTATION_RELATIONSHIP($,$,#66916,#66915)
REPRESENTATION_RELATIONSHIP_WITH_TRANSFORMATION(#720)
SHAPE_REPRESENTATION_RELATIONSHIP()
);
#805=(
REPRESENTATION_RELATIONSHIP($,$,#66917,#66915)
REPRESENTATION_RELATIONSHIP_WITH_TRANSFORMATION(#721)
SHAPE_REPRESENTATION_RELATIONSHIP()
);
#806=(
REPRESENTATION_RELATIONSHIP($,$,#66918,#66915)
REPRESENTATION_RELATIONSHIP_WITH_TRANSFORMATION(#722)
SHAPE_REPRESENTATION_RELATIONSHIP()
);
#807=(
REPRESENTATION_RELATIONSHIP($,$,#66919,#66915)
REPRESENTATION_RELATIONSHIP_WITH_TRANSFORMATION(#723)
SHAPE_REPRESENTATION_RELATIONSHIP()
);
#808=(
REPRESENTATION_RELATIONSHIP($,$,#66920,#66915)
REPRESENTATION_RELATIONSHIP_WITH_TRANSFORMATION(#724)
SHAPE_REPRESENTATION_RELATIONSHIP()
);
#809=(
REPRESENTATION_RELATIONSHIP($,$,#66921,#66915)
REPRESENTATION_RELATIONSHIP_WITH_TRANSFORMATION(#725)
SHAPE_REPRESENTATION_RELATIONSHIP()
);
#810=(
REPRESENTATION_RELATIONSHIP($,$,#66922,#66915)
REPRESENTATION_RELATIONSHIP_WITH_TRANSFORMATION(#726)
SHAPE_REPRESENTATION_RELATIONSHIP()
);
#811=(
REPRESENTATION_RELATIONSHIP($,$,#66923,#66915)
REPRESENTATION_RELATIONSHIP_WITH_TRANSFORMATION(#727)
SHAPE_REPRESENTATION_RELATIONSHIP()
);
#812=(
REPRESENTATION_RELATIONSHIP($,$,#66924,#66915)
REPRESENTATION_RELATIONSHIP_WITH_TRANSFORMATION(#728)
SHAPE_REPRESENTATION_RELATIONSHIP()
);
#813=(
REPRESENTATION_RELATIONSHIP($,$,#66915,#66914)
REPRESENTATION_RELATIONSHIP_WITH_TRANSFORMATION(#729)
SHAPE_REPRESENTATION_RELATIONSHIP()
);
#814=(
REPRESENTATION_RELATIONSHIP($,$,#66891,#66890)
REPRESENTATION_RELATIONSHIP_WITH_TRANSFORMATION(#730)
SHAPE_REPRESENTATION_RELATIONSHIP()
);
#815=(
REPRESENTATION_RELATIONSHIP($,$,#66925,#66890)
REPRESENTATION_RELATIONSHIP_WITH_TRANSFORMATION(#731)
SHAPE_REPRESENTATION_RELATIONSHIP()
);
#816=(
REPRESENTATION_RELATIONSHIP($,$,#66892,#66890)
REPRESENTATION_RELATIONSHIP_WITH_TRANSFORMATION(#732)
SHAPE_REPRESENTATION_RELATIONSHIP()
);
#817=(
REPRESENTATION_RELATIONSHIP($,$,#66893,#66890)
REPRESENTATION_RELATIONSHIP_WITH_TRANSFORMATION(#733)
SHAPE_REPRESENTATION_RELATIONSHIP()
);
#818=(
REPRESENTATION_RELATIONSHIP($,$,#66894,#66890)
REPRESENTATION_RELATIONSHIP_WITH_TRANSFORMATION(#734)
SHAPE_REPRESENTATION_RELATIONSHIP()
);
#819=(
REPRESENTATION_RELATIONSHIP($,$,#66895,#66890)
REPRESENTATION_RELATIONSHIP_WITH_TRANSFORMATION(#735)
SHAPE_REPRESENTATION_RELATIONSHIP()
);
#820=(
REPRESENTATION_RELATIONSHIP($,$,#66898,#66890)
REPRESENTATION_RELATIONSHIP_WITH_TRANSFORMATION(#736)
SHAPE_REPRESENTATION_RELATIONSHIP()
);
#821=(
REPRESENTATION_RELATIONSHIP($,$,#66899,#66890)
REPRESENTATION_RELATIONSHIP_WITH_TRANSFORMATION(#737)
SHAPE_REPRESENTATION_RELATIONSHIP()
);
#822=(
REPRESENTATION_RELATIONSHIP($,$,#66927,#66890)
REPRESENTATION_RELATIONSHIP_WITH_TRANSFORMATION(#738)
SHAPE_REPRESENTATION_RELATIONSHIP()
);
#823=(
REPRESENTATION_RELATIONSHIP($,$,#66929,#66890)
REPRESENTATION_RELATIONSHIP_WITH_TRANSFORMATION(#739)
SHAPE_REPRESENTATION_RELATIONSHIP()
);
#824=(
REPRESENTATION_RELATIONSHIP($,$,#66903,#66890)
REPRESENTATION_RELATIONSHIP_WITH_TRANSFORMATION(#740)
SHAPE_REPRESENTATION_RELATIONSHIP()
);
#825=(
REPRESENTATION_RELATIONSHIP($,$,#66906,#66890)
REPRESENTATION_RELATIONSHIP_WITH_TRANSFORMATION(#741)
SHAPE_REPRESENTATION_RELATIONSHIP()
);
#826=(
REPRESENTATION_RELATIONSHIP($,$,#66909,#66890)
REPRESENTATION_RELATIONSHIP_WITH_TRANSFORMATION(#742)
SHAPE_REPRESENTATION_RELATIONSHIP()
);
#827=(
REPRESENTATION_RELATIONSHIP($,$,#66913,#66890)
REPRESENTATION_RELATIONSHIP_WITH_TRANSFORMATION(#743)
SHAPE_REPRESENTATION_RELATIONSHIP()
);
#828=(
REPRESENTATION_RELATIONSHIP($,$,#66914,#66890)
REPRESENTATION_RELATIONSHIP_WITH_TRANSFORMATION(#744)
SHAPE_REPRESENTATION_RELATIONSHIP()
);
#829=(
REPRESENTATION_RELATIONSHIP($,$,#66928,#66890)
REPRESENTATION_RELATIONSHIP_WITH_TRANSFORMATION(#745)
SHAPE_REPRESENTATION_RELATIONSHIP()
);
#830=(
REPRESENTATION_RELATIONSHIP($,$,#66926,#66890)
REPRESENTATION_RELATIONSHIP_WITH_TRANSFORMATION(#746)
SHAPE_REPRESENTATION_RELATIONSHIP()
);
#831=(
REPRESENTATION_RELATIONSHIP($,$,#66925,#66890)
REPRESENTATION_RELATIONSHIP_WITH_TRANSFORMATION(#747)
SHAPE_REPRESENTATION_RELATIONSHIP()
);
#832=(
REPRESENTATION_RELATIONSHIP($,$,#66927,#66890)
REPRESENTATION_RELATIONSHIP_WITH_TRANSFORMATION(#748)
SHAPE_REPRESENTATION_RELATIONSHIP()
);
#833=(
REPRESENTATION_RELATIONSHIP($,$,#66927,#66890)
REPRESENTATION_RELATIONSHIP_WITH_TRANSFORMATION(#749)
SHAPE_REPRESENTATION_RELATIONSHIP()
);
#834=(
REPRESENTATION_RELATIONSHIP($,$,#66929,#66890)
REPRESENTATION_RELATIONSHIP_WITH_TRANSFORMATION(#750)
SHAPE_REPRESENTATION_RELATIONSHIP()
);
#835=(
REPRESENTATION_RELATIONSHIP($,$,#66929,#66890)
REPRESENTATION_RELATIONSHIP_WITH_TRANSFORMATION(#751)
SHAPE_REPRESENTATION_RELATIONSHIP()
);
#836=(
REPRESENTATION_RELATIONSHIP($,$,#66929,#66890)
REPRESENTATION_RELATIONSHIP_WITH_TRANSFORMATION(#752)
SHAPE_REPRESENTATION_RELATIONSHIP()
);
#837=(
REPRESENTATION_RELATIONSHIP($,$,#66929,#66890)
REPRESENTATION_RELATIONSHIP_WITH_TRANSFORMATION(#753)
SHAPE_REPRESENTATION_RELATIONSHIP()
);
#838=(
REPRESENTATION_RELATIONSHIP($,$,#66929,#66890)
REPRESENTATION_RELATIONSHIP_WITH_TRANSFORMATION(#754)
SHAPE_REPRESENTATION_RELATIONSHIP()
);
#839=(
REPRESENTATION_RELATIONSHIP($,$,#66929,#66890)
REPRESENTATION_RELATIONSHIP_WITH_TRANSFORMATION(#755)
SHAPE_REPRESENTATION_RELATIONSHIP()
);
#840=(
REPRESENTATION_RELATIONSHIP($,$,#66929,#66890)
REPRESENTATION_RELATIONSHIP_WITH_TRANSFORMATION(#756)
SHAPE_REPRESENTATION_RELATIONSHIP()
);
#841=(
REPRESENTATION_RELATIONSHIP($,$,#66929,#66890)
REPRESENTATION_RELATIONSHIP_WITH_TRANSFORMATION(#757)
SHAPE_REPRESENTATION_RELATIONSHIP()
);
#842=(
REPRESENTATION_RELATIONSHIP($,$,#66929,#66890)
REPRESENTATION_RELATIONSHIP_WITH_TRANSFORMATION(#758)
SHAPE_REPRESENTATION_RELATIONSHIP()
);
#843=(
REPRESENTATION_RELATIONSHIP($,$,#66929,#66890)
REPRESENTATION_RELATIONSHIP_WITH_TRANSFORMATION(#759)
SHAPE_REPRESENTATION_RELATIONSHIP()
);
#844=(
REPRESENTATION_RELATIONSHIP($,$,#66929,#66890)
REPRESENTATION_RELATIONSHIP_WITH_TRANSFORMATION(#760)
SHAPE_REPRESENTATION_RELATIONSHIP()
);
#845=(
REPRESENTATION_RELATIONSHIP($,$,#66929,#66890)
REPRESENTATION_RELATIONSHIP_WITH_TRANSFORMATION(#761)
SHAPE_REPRESENTATION_RELATIONSHIP()
);
#846=(
REPRESENTATION_RELATIONSHIP($,$,#66929,#66890)
REPRESENTATION_RELATIONSHIP_WITH_TRANSFORMATION(#762)
SHAPE_REPRESENTATION_RELATIONSHIP()
);
#847=(
REPRESENTATION_RELATIONSHIP($,$,#66929,#66890)
REPRESENTATION_RELATIONSHIP_WITH_TRANSFORMATION(#763)
SHAPE_REPRESENTATION_RELATIONSHIP()
);
#848=(
REPRESENTATION_RELATIONSHIP($,$,#66929,#66890)
REPRESENTATION_RELATIONSHIP_WITH_TRANSFORMATION(#764)
SHAPE_REPRESENTATION_RELATIONSHIP()
);
#849=(
REPRESENTATION_RELATIONSHIP($,$,#66929,#66890)
REPRESENTATION_RELATIONSHIP_WITH_TRANSFORMATION(#765)
SHAPE_REPRESENTATION_RELATIONSHIP()
);
#850=(
REPRESENTATION_RELATIONSHIP($,$,#66929,#66890)
REPRESENTATION_RELATIONSHIP_WITH_TRANSFORMATION(#766)
SHAPE_REPRESENTATION_RELATIONSHIP()
);
#851=(
REPRESENTATION_RELATIONSHIP($,$,#66929,#66890)
REPRESENTATION_RELATIONSHIP_WITH_TRANSFORMATION(#767)
SHAPE_REPRESENTATION_RELATIONSHIP()
);
#852=(
REPRESENTATION_RELATIONSHIP($,$,#66929,#66890)
REPRESENTATION_RELATIONSHIP_WITH_TRANSFORMATION(#768)
SHAPE_REPRESENTATION_RELATIONSHIP()
);
#853=(
REPRESENTATION_RELATIONSHIP($,$,#66929,#66890)
REPRESENTATION_RELATIONSHIP_WITH_TRANSFORMATION(#769)
SHAPE_REPRESENTATION_RELATIONSHIP()
);
#854=(
REPRESENTATION_RELATIONSHIP($,$,#66929,#66890)
REPRESENTATION_RELATIONSHIP_WITH_TRANSFORMATION(#770)
SHAPE_REPRESENTATION_RELATIONSHIP()
);
#855=(
REPRESENTATION_RELATIONSHIP($,$,#66929,#66890)
REPRESENTATION_RELATIONSHIP_WITH_TRANSFORMATION(#771)
SHAPE_REPRESENTATION_RELATIONSHIP()
);
#856=(
REPRESENTATION_RELATIONSHIP($,$,#66926,#66890)
REPRESENTATION_RELATIONSHIP_WITH_TRANSFORMATION(#772)
SHAPE_REPRESENTATION_RELATIONSHIP()
);
#857=(
REPRESENTATION_RELATIONSHIP($,$,#66927,#66890)
REPRESENTATION_RELATIONSHIP_WITH_TRANSFORMATION(#773)
SHAPE_REPRESENTATION_RELATIONSHIP()
);
#858=(
REPRESENTATION_RELATIONSHIP($,$,#66927,#66890)
REPRESENTATION_RELATIONSHIP_WITH_TRANSFORMATION(#774)
SHAPE_REPRESENTATION_RELATIONSHIP()
);
#859=(
REPRESENTATION_RELATIONSHIP($,$,#66927,#66890)
REPRESENTATION_RELATIONSHIP_WITH_TRANSFORMATION(#775)
SHAPE_REPRESENTATION_RELATIONSHIP()
);
#860=(
REPRESENTATION_RELATIONSHIP($,$,#66929,#66890)
REPRESENTATION_RELATIONSHIP_WITH_TRANSFORMATION(#776)
SHAPE_REPRESENTATION_RELATIONSHIP()
);
#861=(
REPRESENTATION_RELATIONSHIP($,$,#66928,#66890)
REPRESENTATION_RELATIONSHIP_WITH_TRANSFORMATION(#777)
SHAPE_REPRESENTATION_RELATIONSHIP()
);
#862=(
REPRESENTATION_RELATIONSHIP($,$,#66929,#66890)
REPRESENTATION_RELATIONSHIP_WITH_TRANSFORMATION(#778)
SHAPE_REPRESENTATION_RELATIONSHIP()
);
#863=(
REPRESENTATION_RELATIONSHIP($,$,#66929,#66890)
REPRESENTATION_RELATIONSHIP_WITH_TRANSFORMATION(#779)
SHAPE_REPRESENTATION_RELATIONSHIP()
);
#864=(
REPRESENTATION_RELATIONSHIP($,$,#66929,#66890)
REPRESENTATION_RELATIONSHIP_WITH_TRANSFORMATION(#780)
SHAPE_REPRESENTATION_RELATIONSHIP()
);
#865=(
REPRESENTATION_RELATIONSHIP($,$,#66929,#66890)
REPRESENTATION_RELATIONSHIP_WITH_TRANSFORMATION(#781)
SHAPE_REPRESENTATION_RELATIONSHIP()
);
#866=(
REPRESENTATION_RELATIONSHIP($,$,#66929,#66890)
REPRESENTATION_RELATIONSHIP_WITH_TRANSFORMATION(#782)
SHAPE_REPRESENTATION_RELATIONSHIP()
);
#867=(
REPRESENTATION_RELATIONSHIP($,$,#66929,#66890)
REPRESENTATION_RELATIONSHIP_WITH_TRANSFORMATION(#783)
SHAPE_REPRESENTATION_RELATIONSHIP()
);
#868=CONTEXT_DEPENDENT_SHAPE_REPRESENTATION(#784,#66774);
#869=CONTEXT_DEPENDENT_SHAPE_REPRESENTATION(#785,#66775);
#870=CONTEXT_DEPENDENT_SHAPE_REPRESENTATION(#786,#66781);
#871=CONTEXT_DEPENDENT_SHAPE_REPRESENTATION(#787,#66782);
#872=CONTEXT_DEPENDENT_SHAPE_REPRESENTATION(#788,#66783);
#873=CONTEXT_DEPENDENT_SHAPE_REPRESENTATION(#789,#66784);
#874=CONTEXT_DEPENDENT_SHAPE_REPRESENTATION(#790,#66785);
#875=CONTEXT_DEPENDENT_SHAPE_REPRESENTATION(#791,#66786);
#876=CONTEXT_DEPENDENT_SHAPE_REPRESENTATION(#792,#66787);
#877=CONTEXT_DEPENDENT_SHAPE_REPRESENTATION(#793,#66788);
#878=CONTEXT_DEPENDENT_SHAPE_REPRESENTATION(#794,#66789);
#879=CONTEXT_DEPENDENT_SHAPE_REPRESENTATION(#795,#66790);
#880=CONTEXT_DEPENDENT_SHAPE_REPRESENTATION(#796,#66794);
#881=CONTEXT_DEPENDENT_SHAPE_REPRESENTATION(#797,#66795);
#882=CONTEXT_DEPENDENT_SHAPE_REPRESENTATION(#798,#66799);
#883=CONTEXT_DEPENDENT_SHAPE_REPRESENTATION(#799,#66800);
#884=CONTEXT_DEPENDENT_SHAPE_REPRESENTATION(#800,#66805);
#885=CONTEXT_DEPENDENT_SHAPE_REPRESENTATION(#801,#66806);
#886=CONTEXT_DEPENDENT_SHAPE_REPRESENTATION(#802,#66807);
#887=CONTEXT_DEPENDENT_SHAPE_REPRESENTATION(#803,#66808);
#888=CONTEXT_DEPENDENT_SHAPE_REPRESENTATION(#804,#66821);
#889=CONTEXT_DEPENDENT_SHAPE_REPRESENTATION(#805,#66822);
#890=CONTEXT_DEPENDENT_SHAPE_REPRESENTATION(#806,#66823);
#891=CONTEXT_DEPENDENT_SHAPE_REPRESENTATION(#807,#66824);
#892=CONTEXT_DEPENDENT_SHAPE_REPRESENTATION(#808,#66825);
#893=CONTEXT_DEPENDENT_SHAPE_REPRESENTATION(#809,#66826);
#894=CONTEXT_DEPENDENT_SHAPE_REPRESENTATION(#810,#66827);
#895=CONTEXT_DEPENDENT_SHAPE_REPRESENTATION(#811,#66828);
#896=CONTEXT_DEPENDENT_SHAPE_REPRESENTATION(#812,#66829);
#897=CONTEXT_DEPENDENT_SHAPE_REPRESENTATION(#813,#66830);
#898=CONTEXT_DEPENDENT_SHAPE_REPRESENTATION(#814,#66836);
#899=CONTEXT_DEPENDENT_SHAPE_REPRESENTATION(#815,#66837);
#900=CONTEXT_DEPENDENT_SHAPE_REPRESENTATION(#816,#66838);
#901=CONTEXT_DEPENDENT_SHAPE_REPRESENTATION(#817,#66839);
#902=CONTEXT_DEPENDENT_SHAPE_REPRESENTATION(#818,#66840);
#903=CONTEXT_DEPENDENT_SHAPE_REPRESENTATION(#819,#66841);
#904=CONTEXT_DEPENDENT_SHAPE_REPRESENTATION(#820,#66842);
#905=CONTEXT_DEPENDENT_SHAPE_REPRESENTATION(#821,#66843);
#906=CONTEXT_DEPENDENT_SHAPE_REPRESENTATION(#822,#66844);
#907=CONTEXT_DEPENDENT_SHAPE_REPRESENTATION(#823,#66845);
#908=CONTEXT_DEPENDENT_SHAPE_REPRESENTATION(#824,#66846);
#909=CONTEXT_DEPENDENT_SHAPE_REPRESENTATION(#825,#66847);
#910=CONTEXT_DEPENDENT_SHAPE_REPRESENTATION(#826,#66848);
#911=CONTEXT_DEPENDENT_SHAPE_REPRESENTATION(#827,#66849);
#912=CONTEXT_DEPENDENT_SHAPE_REPRESENTATION(#828,#66850);
#913=CONTEXT_DEPENDENT_SHAPE_REPRESENTATION(#829,#66851);
#914=CONTEXT_DEPENDENT_SHAPE_REPRESENTATION(#830,#66852);
#915=CONTEXT_DEPENDENT_SHAPE_REPRESENTATION(#831,#66853);
#916=CONTEXT_DEPENDENT_SHAPE_REPRESENTATION(#832,#66854);
#917=CONTEXT_DEPENDENT_SHAPE_REPRESENTATION(#833,#66855);
#918=CONTEXT_DEPENDENT_SHAPE_REPRESENTATION(#834,#66856);
#919=CONTEXT_DEPENDENT_SHAPE_REPRESENTATION(#835,#66857);
#920=CONTEXT_DEPENDENT_SHAPE_REPRESENTATION(#836,#66858);
#921=CONTEXT_DEPENDENT_SHAPE_REPRESENTATION(#837,#66859);
#922=CONTEXT_DEPENDENT_SHAPE_REPRESENTATION(#838,#66860);
#923=CONTEXT_DEPENDENT_SHAPE_REPRESENTATION(#839,#66861);
#924=CONTEXT_DEPENDENT_SHAPE_REPRESENTATION(#840,#66862);
#925=CONTEXT_DEPENDENT_SHAPE_REPRESENTATION(#841,#66863);
#926=CONTEXT_DEPENDENT_SHAPE_REPRESENTATION(#842,#66864);
#927=CONTEXT_DEPENDENT_SHAPE_REPRESENTATION(#843,#66865);
#928=CONTEXT_DEPENDENT_SHAPE_REPRESENTATION(#844,#66866);
#929=CONTEXT_DEPENDENT_SHAPE_REPRESENTATION(#845,#66867);
#930=CONTEXT_DEPENDENT_SHAPE_REPRESENTATION(#846,#66868);
#931=CONTEXT_DEPENDENT_SHAPE_REPRESENTATION(#847,#66869);
#932=CONTEXT_DEPENDENT_SHAPE_REPRESENTATION(#848,#66870);
#933=CONTEXT_DEPENDENT_SHAPE_REPRESENTATION(#849,#66871);
#934=CONTEXT_DEPENDENT_SHAPE_REPRESENTATION(#850,#66872);
#935=CONTEXT_DEPENDENT_SHAPE_REPRESENTATION(#851,#66873);
#936=CONTEXT_DEPENDENT_SHAPE_REPRESENTATION(#852,#66874);
#937=CONTEXT_DEPENDENT_SHAPE_REPRESENTATION(#853,#66875);
#938=CONTEXT_DEPENDENT_SHAPE_REPRESENTATION(#854,#66876);
#939=CONTEXT_DEPENDENT_SHAPE_REPRESENTATION(#855,#66877);
#940=CONTEXT_DEPENDENT_SHAPE_REPRESENTATION(#856,#66878);
#941=CONTEXT_DEPENDENT_SHAPE_REPRESENTATION(#857,#66879);
#942=CONTEXT_DEPENDENT_SHAPE_REPRESENTATION(#858,#66880);
#943=CONTEXT_DEPENDENT_SHAPE_REPRESENTATION(#859,#66881);
#944=CONTEXT_DEPENDENT_SHAPE_REPRESENTATION(#860,#66882);
#945=CONTEXT_DEPENDENT_SHAPE_REPRESENTATION(#861,#66883);
#946=CONTEXT_DEPENDENT_SHAPE_REPRESENTATION(#862,#66884);
#947=CONTEXT_DEPENDENT_SHAPE_REPRESENTATION(#863,#66885);
#948=CONTEXT_DEPENDENT_SHAPE_REPRESENTATION(#864,#66886);
#949=CONTEXT_DEPENDENT_SHAPE_REPRESENTATION(#865,#66887);
#950=CONTEXT_DEPENDENT_SHAPE_REPRESENTATION(#866,#66888);
#951=CONTEXT_DEPENDENT_SHAPE_REPRESENTATION(#867,#66889);
#952=NEXT_ASSEMBLY_USAGE_OCCURRENCE('Ball Screw Support Bracket:1',
'Ball Screw Support Bracket:1','Ball Screw Support Bracket:1',#66936,#66937,
'Ball Screw Support Bracket:1');
#953=NEXT_ASSEMBLY_USAGE_OCCURRENCE('Ball Screw Support Plate:1',
'Ball Screw Support Plate:1','Ball Screw Support Plate:1',#66936,#66938,
'Ball Screw Support Plate:1');
#954=NEXT_ASSEMBLY_USAGE_OCCURRENCE('Linear Guide Rail:1',
'Linear Guide Rail:1','Linear Guide Rail:1',#66933,#66941,
'Linear Guide Rail:1');
#955=NEXT_ASSEMBLY_USAGE_OCCURRENCE('Linear Guide Slider:1',
'Linear Guide Slider:1','Linear Guide Slider:1',#66933,#66942,
'Linear Guide Slider:1');
#956=NEXT_ASSEMBLY_USAGE_OCCURRENCE('Slider End Cap:1',
'Slider End Cap:1','Slider End Cap:1',#66933,#66943,'Slider End Cap:1');
#957=NEXT_ASSEMBLY_USAGE_OCCURRENCE('Linear Guide Slider:2',
'Linear Guide Slider:2','Linear Guide Slider:2',#66933,#66942,
'Linear Guide Slider:2');
#958=NEXT_ASSEMBLY_USAGE_OCCURRENCE('Slider End Cap:2',
'Slider End Cap:2','Slider End Cap:2',#66933,#66943,'Slider End Cap:2');
#959=NEXT_ASSEMBLY_USAGE_OCCURRENCE('Linear Guide Rail:2',
'Linear Guide Rail:2','Linear Guide Rail:2',#66940,#66941,
'Linear Guide Rail:2');
#960=NEXT_ASSEMBLY_USAGE_OCCURRENCE('Linear Guide Slider:3',
'Linear Guide Slider:3','Linear Guide Slider:3',#66940,#66942,
'Linear Guide Slider:3');
#961=NEXT_ASSEMBLY_USAGE_OCCURRENCE('Slider End Cap:3',
'Slider End Cap:3','Slider End Cap:3',#66940,#66943,'Slider End Cap:3');
#962=NEXT_ASSEMBLY_USAGE_OCCURRENCE('Linear Guide Slider:4',
'Linear Guide Slider:4','Linear Guide Slider:4',#66940,#66942,
'Linear Guide Slider:4');
#963=NEXT_ASSEMBLY_USAGE_OCCURRENCE('Slider End Cap:4',
'Slider End Cap:4','Slider End Cap:4',#66940,#66943,'Slider End Cap:4');
#964=NEXT_ASSEMBLY_USAGE_OCCURRENCE('Ball Screw Shaft:1',
'Ball Screw Shaft:1','Ball Screw Shaft:1',#66944,#66945,
'Ball Screw Shaft:1');
#965=NEXT_ASSEMBLY_USAGE_OCCURRENCE('Ball Screw Nut:1',
'Ball Screw Nut:1','Ball Screw Nut:1',#66944,#66946,'Ball Screw Nut:1');
#966=NEXT_ASSEMBLY_USAGE_OCCURRENCE('Fixed Bearing Housing:1',
'Fixed Bearing Housing:1','Fixed Bearing Housing:1',#66947,#66948,
'Fixed Bearing Housing:1');
#967=NEXT_ASSEMBLY_USAGE_OCCURRENCE('Washer:1','Washer:1','Washer:1',#66947,
#66949,'Washer:1');
#968=NEXT_ASSEMBLY_USAGE_OCCURRENCE('Floating Bearing Housing:1',
'Floating Bearing Housing:1','Floating Bearing Housing:1',#66950,#66951,
'Floating Bearing Housing:1');
#969=NEXT_ASSEMBLY_USAGE_OCCURRENCE('Collar:1','Collar:1','Collar:1',#66950,
#66953,'Collar:1');
#970=NEXT_ASSEMBLY_USAGE_OCCURRENCE('Lock Nut:1','Lock Nut:1',
'Lock Nut:1',#66950,#66952,'Lock Nut:1');
#971=NEXT_ASSEMBLY_USAGE_OCCURRENCE('Collar:2','Collar:2','Collar:2',#66950,
#66953,'Collar:2');
#972=NEXT_ASSEMBLY_USAGE_OCCURRENCE('Coupling Spider:1',
'Coupling Spider:1','Coupling Spider:1',#66956,#66957,
'Coupling Spider:1');
#973=NEXT_ASSEMBLY_USAGE_OCCURRENCE('Coupling Set Screw:1',
'Coupling Set Screw:1','Coupling Set Screw:1',#66956,#66958,
'Coupling Set Screw:1');
#974=NEXT_ASSEMBLY_USAGE_OCCURRENCE('Coupling Clamp Screw 1:1',
'Coupling Clamp Screw 1:1','Coupling Clamp Screw 1:1',#66956,#66959,
'Coupling Clamp Screw 1:1');
#975=NEXT_ASSEMBLY_USAGE_OCCURRENCE('Coupling Clamp Screw 2:1',
'Coupling Clamp Screw 2:1','Coupling Clamp Screw 2:1',#66956,#66960,
'Coupling Clamp Screw 2:1');
#976=NEXT_ASSEMBLY_USAGE_OCCURRENCE('Coupling Hub 2:1',
'Coupling Hub 2:1','Coupling Hub 2:1',#66956,#66961,'Coupling Hub 2:1');
#977=NEXT_ASSEMBLY_USAGE_OCCURRENCE('Coupling Washer:1',
'Coupling Washer:1','Coupling Washer:1',#66956,#66962,
'Coupling Washer:1');
#978=NEXT_ASSEMBLY_USAGE_OCCURRENCE('Coupling Clamp Ring 1:1',
'Coupling Clamp Ring 1:1','Coupling Clamp Ring 1:1',#66956,#66963,
'Coupling Clamp Ring 1:1');
#979=NEXT_ASSEMBLY_USAGE_OCCURRENCE('Coupling Clamp Ring 2:1',
'Coupling Clamp Ring 2:1','Coupling Clamp Ring 2:1',#66956,#66964,
'Coupling Clamp Ring 2:1');
#980=NEXT_ASSEMBLY_USAGE_OCCURRENCE('Coupling Hub 1:1',
'Coupling Hub 1:1','Coupling Hub 1:1',#66956,#66965,'Coupling Hub 1:1');
#981=NEXT_ASSEMBLY_USAGE_OCCURRENCE('Coupling Components:1',
'Coupling Components:1','Coupling Components:1',#66955,#66956,
'Coupling Components:1');
#982=NEXT_ASSEMBLY_USAGE_OCCURRENCE('Main Plate:1','Main Plate:1',
'Main Plate:1',#66931,#66932,'Main Plate:1');
#983=NEXT_ASSEMBLY_USAGE_OCCURRENCE('Linear Guide Spacer:1',
'Linear Guide Spacer:1','Linear Guide Spacer:1',#66931,#66966,
'Linear Guide Spacer:1');
#984=NEXT_ASSEMBLY_USAGE_OCCURRENCE('Linear Guide Assembly 1:1',
'Linear Guide Assembly 1:1','Linear Guide Assembly 1:1',#66931,#66933,
'Linear Guide Assembly 1:1');
#985=NEXT_ASSEMBLY_USAGE_OCCURRENCE('Ball Screw Spacer 2:1',
'Ball Screw Spacer 2:1','Ball Screw Spacer 2:1',#66931,#66934,
'Ball Screw Spacer 2:1');
#986=NEXT_ASSEMBLY_USAGE_OCCURRENCE('Motor Mount Plate:1',
'Motor Mount Plate:1','Motor Mount Plate:1',#66931,#66935,
'Motor Mount Plate:1');
#987=NEXT_ASSEMBLY_USAGE_OCCURRENCE('Ball Screw Support Assembly:1',
'Ball Screw Support Assembly:1','Ball Screw Support Assembly:1',#66931,
#66936,'Ball Screw Support Assembly:1');
#988=NEXT_ASSEMBLY_USAGE_OCCURRENCE('Ball Screw Support Spacer:1',
'Ball Screw Support Spacer:1','Ball Screw Support Spacer:1',#66931,#66939,
'Ball Screw Support Spacer:1');
#989=NEXT_ASSEMBLY_USAGE_OCCURRENCE('Linear Guide Assembly 2:1',
'Linear Guide Assembly 2:1','Linear Guide Assembly 2:1',#66931,#66940,
'Linear Guide Assembly 2:1');
#990=NEXT_ASSEMBLY_USAGE_OCCURRENCE('Low Head Cap Screw M6x25:1',
'Low Head Cap Screw M6x25:1','Low Head Cap Screw M6x25:1',#66931,#66968,
'Low Head Cap Screw M6x25:1');
#991=NEXT_ASSEMBLY_USAGE_OCCURRENCE('Socket Head Cap Screw M6x25:1',
'Socket Head Cap Screw M6x25:1','Socket Head Cap Screw M6x25:1',#66931,
#66970,'Socket Head Cap Screw M6x25:1');
#992=NEXT_ASSEMBLY_USAGE_OCCURRENCE('Ball Screw Assembly:1',
'Ball Screw Assembly:1','Ball Screw Assembly:1',#66931,#66944,
'Ball Screw Assembly:1');
#993=NEXT_ASSEMBLY_USAGE_OCCURRENCE('Fixed Bearing Support Assembly:1',
'Fixed Bearing Support Assembly:1','Fixed Bearing Support Assembly:1',#66931,
#66947,'Fixed Bearing Support Assembly:1');
#994=NEXT_ASSEMBLY_USAGE_OCCURRENCE(
'Floating Bearing Support Assembly:1',
'Floating Bearing Support Assembly:1',
'Floating Bearing Support Assembly:1',#66931,#66950,
'Floating Bearing Support Assembly:1');
#995=NEXT_ASSEMBLY_USAGE_OCCURRENCE('Ball Screw Spacer 1:1',
'Ball Screw Spacer 1:1','Ball Screw Spacer 1:1',#66931,#66954,
'Ball Screw Spacer 1:1');
#996=NEXT_ASSEMBLY_USAGE_OCCURRENCE('Coupling Assembly:1',
'Coupling Assembly:1','Coupling Assembly:1',#66931,#66955,
'Coupling Assembly:1');
#997=NEXT_ASSEMBLY_USAGE_OCCURRENCE('Linear Slider Spacer:1',
'Linear Slider Spacer:1','Linear Slider Spacer:1',#66931,#66969,
'Linear Slider Spacer:1');
#998=NEXT_ASSEMBLY_USAGE_OCCURRENCE('Socket Head Cap Screw M6x20:1',
'Socket Head Cap Screw M6x20:1','Socket Head Cap Screw M6x20:1',#66931,
#66967,'Socket Head Cap Screw M6x20:1');
#999=NEXT_ASSEMBLY_USAGE_OCCURRENCE('Linear Guide Spacer:2',
'Linear Guide Spacer:2','Linear Guide Spacer:2',#66931,#66966,
'Linear Guide Spacer:2');
#1000=NEXT_ASSEMBLY_USAGE_OCCURRENCE('Low Head Cap Screw M6x25:2',
'Low Head Cap Screw M6x25:2','Low Head Cap Screw M6x25:2',#66931,#66968,
'Low Head Cap Screw M6x25:2');
#1001=NEXT_ASSEMBLY_USAGE_OCCURRENCE('Low Head Cap Screw M6x25:3',
'Low Head Cap Screw M6x25:3','Low Head Cap Screw M6x25:3',#66931,#66968,
'Low Head Cap Screw M6x25:3');
#1002=NEXT_ASSEMBLY_USAGE_OCCURRENCE('Socket Head Cap Screw M6x25:2',
'Socket Head Cap Screw M6x25:2','Socket Head Cap Screw M6x25:2',#66931,
#66970,'Socket Head Cap Screw M6x25:2');
#1003=NEXT_ASSEMBLY_USAGE_OCCURRENCE('Socket Head Cap Screw M6x25:3',
'Socket Head Cap Screw M6x25:3','Socket Head Cap Screw M6x25:3',#66931,
#66970,'Socket Head Cap Screw M6x25:3');
#1004=NEXT_ASSEMBLY_USAGE_OCCURRENCE('Socket Head Cap Screw M6x25:4',
'Socket Head Cap Screw M6x25:4','Socket Head Cap Screw M6x25:4',#66931,
#66970,'Socket Head Cap Screw M6x25:4');
#1005=NEXT_ASSEMBLY_USAGE_OCCURRENCE('Socket Head Cap Screw M6x25:5',
'Socket Head Cap Screw M6x25:5','Socket Head Cap Screw M6x25:5',#66931,
#66970,'Socket Head Cap Screw M6x25:5');
#1006=NEXT_ASSEMBLY_USAGE_OCCURRENCE('Socket Head Cap Screw M6x25:6',
'Socket Head Cap Screw M6x25:6','Socket Head Cap Screw M6x25:6',#66931,
#66970,'Socket Head Cap Screw M6x25:6');
#1007=NEXT_ASSEMBLY_USAGE_OCCURRENCE('Socket Head Cap Screw M6x25:7',
'Socket Head Cap Screw M6x25:7','Socket Head Cap Screw M6x25:7',#66931,
#66970,'Socket Head Cap Screw M6x25:7');
#1008=NEXT_ASSEMBLY_USAGE_OCCURRENCE('Socket Head Cap Screw M6x25:8',
'Socket Head Cap Screw M6x25:8','Socket Head Cap Screw M6x25:8',#66931,
#66970,'Socket Head Cap Screw M6x25:8');
#1009=NEXT_ASSEMBLY_USAGE_OCCURRENCE('Socket Head Cap Screw M6x25:9',
'Socket Head Cap Screw M6x25:9','Socket Head Cap Screw M6x25:9',#66931,
#66970,'Socket Head Cap Screw M6x25:9');
#1010=NEXT_ASSEMBLY_USAGE_OCCURRENCE('Socket Head Cap Screw M6x25:10',
'Socket Head Cap Screw M6x25:10','Socket Head Cap Screw M6x25:10',#66931,
#66970,'Socket Head Cap Screw M6x25:10');
#1011=NEXT_ASSEMBLY_USAGE_OCCURRENCE('Socket Head Cap Screw M6x25:11',
'Socket Head Cap Screw M6x25:11','Socket Head Cap Screw M6x25:11',#66931,
#66970,'Socket Head Cap Screw M6x25:11');
#1012=NEXT_ASSEMBLY_USAGE_OCCURRENCE('Socket Head Cap Screw M6x25:12',
'Socket Head Cap Screw M6x25:12','Socket Head Cap Screw M6x25:12',#66931,
#66970,'Socket Head Cap Screw M6x25:12');
#1013=NEXT_ASSEMBLY_USAGE_OCCURRENCE('Socket Head Cap Screw M6x25:13',
'Socket Head Cap Screw M6x25:13','Socket Head Cap Screw M6x25:13',#66931,
#66970,'Socket Head Cap Screw M6x25:13');
#1014=NEXT_ASSEMBLY_USAGE_OCCURRENCE('Socket Head Cap Screw M6x25:14',
'Socket Head Cap Screw M6x25:14','Socket Head Cap Screw M6x25:14',#66931,
#66970,'Socket Head Cap Screw M6x25:14');
#1015=NEXT_ASSEMBLY_USAGE_OCCURRENCE('Socket Head Cap Screw M6x25:15',
'Socket Head Cap Screw M6x25:15','Socket Head Cap Screw M6x25:15',#66931,
#66970,'Socket Head Cap Screw M6x25:15');
#1016=NEXT_ASSEMBLY_USAGE_OCCURRENCE('Socket Head Cap Screw M6x25:16',
'Socket Head Cap Screw M6x25:16','Socket Head Cap Screw M6x25:16',#66931,
#66970,'Socket Head Cap Screw M6x25:16');
#1017=NEXT_ASSEMBLY_USAGE_OCCURRENCE('Socket Head Cap Screw M6x25:17',
'Socket Head Cap Screw M6x25:17','Socket Head Cap Screw M6x25:17',#66931,
#66970,'Socket Head Cap Screw M6x25:17');
#1018=NEXT_ASSEMBLY_USAGE_OCCURRENCE('Socket Head Cap Screw M6x25:18',
'Socket Head Cap Screw M6x25:18','Socket Head Cap Screw M6x25:18',#66931,
#66970,'Socket Head Cap Screw M6x25:18');
#1019=NEXT_ASSEMBLY_USAGE_OCCURRENCE('Socket Head Cap Screw M6x25:19',
'Socket Head Cap Screw M6x25:19','Socket Head Cap Screw M6x25:19',#66931,
#66970,'Socket Head Cap Screw M6x25:19');
#1020=NEXT_ASSEMBLY_USAGE_OCCURRENCE('Socket Head Cap Screw M6x25:20',
'Socket Head Cap Screw M6x25:20','Socket Head Cap Screw M6x25:20',#66931,
#66970,'Socket Head Cap Screw M6x25:20');
#1021=NEXT_ASSEMBLY_USAGE_OCCURRENCE('Socket Head Cap Screw M6x25:21',
'Socket Head Cap Screw M6x25:21','Socket Head Cap Screw M6x25:21',#66931,
#66970,'Socket Head Cap Screw M6x25:21');
#1022=NEXT_ASSEMBLY_USAGE_OCCURRENCE('Socket Head Cap Screw M6x25:22',
'Socket Head Cap Screw M6x25:22','Socket Head Cap Screw M6x25:22',#66931,
#66970,'Socket Head Cap Screw M6x25:22');
#1023=NEXT_ASSEMBLY_USAGE_OCCURRENCE('Socket Head Cap Screw M6x25:23',
'Socket Head Cap Screw M6x25:23','Socket Head Cap Screw M6x25:23',#66931,
#66970,'Socket Head Cap Screw M6x25:23');
#1024=NEXT_ASSEMBLY_USAGE_OCCURRENCE('Socket Head Cap Screw M6x20:2',
'Socket Head Cap Screw M6x20:2','Socket Head Cap Screw M6x20:2',#66931,
#66967,'Socket Head Cap Screw M6x20:2');
#1025=NEXT_ASSEMBLY_USAGE_OCCURRENCE('Low Head Cap Screw M6x25:4',
'Low Head Cap Screw M6x25:4','Low Head Cap Screw M6x25:4',#66931,#66968,
'Low Head Cap Screw M6x25:4');
#1026=NEXT_ASSEMBLY_USAGE_OCCURRENCE('Low Head Cap Screw M6x25:5',
'Low Head Cap Screw M6x25:5','Low Head Cap Screw M6x25:5',#66931,#66968,
'Low Head Cap Screw M6x25:5');
#1027=NEXT_ASSEMBLY_USAGE_OCCURRENCE('Low Head Cap Screw M6x25:6',
'Low Head Cap Screw M6x25:6','Low Head Cap Screw M6x25:6',#66931,#66968,
'Low Head Cap Screw M6x25:6');
#1028=NEXT_ASSEMBLY_USAGE_OCCURRENCE('Socket Head Cap Screw M6x25:24',
'Socket Head Cap Screw M6x25:24','Socket Head Cap Screw M6x25:24',#66931,
#66970,'Socket Head Cap Screw M6x25:24');
#1029=NEXT_ASSEMBLY_USAGE_OCCURRENCE('Linear Slider Spacer:2',
'Linear Slider Spacer:2','Linear Slider Spacer:2',#66931,#66969,
'Linear Slider Spacer:2');
#1030=NEXT_ASSEMBLY_USAGE_OCCURRENCE('Socket Head Cap Screw M6x25:25',
'Socket Head Cap Screw M6x25:25','Socket Head Cap Screw M6x25:25',#66931,
#66970,'Socket Head Cap Screw M6x25:25');
#1031=NEXT_ASSEMBLY_USAGE_OCCURRENCE('Socket Head Cap Screw M6x25:26',
'Socket Head Cap Screw M6x25:26','Socket Head Cap Screw M6x25:26',#66931,
#66970,'Socket Head Cap Screw M6x25:26');
#1032=NEXT_ASSEMBLY_USAGE_OCCURRENCE('Socket Head Cap Screw M6x25:27',
'Socket Head Cap Screw M6x25:27','Socket Head Cap Screw M6x25:27',#66931,
#66970,'Socket Head Cap Screw M6x25:27');
#1033=NEXT_ASSEMBLY_USAGE_OCCURRENCE('Socket Head Cap Screw M6x25:28',
'Socket Head Cap Screw M6x25:28','Socket Head Cap Screw M6x25:28',#66931,
#66970,'Socket Head Cap Screw M6x25:28');
#1034=NEXT_ASSEMBLY_USAGE_OCCURRENCE('Socket Head Cap Screw M6x25:29',
'Socket Head Cap Screw M6x25:29','Socket Head Cap Screw M6x25:29',#66931,
#66970,'Socket Head Cap Screw M6x25:29');
#1035=NEXT_ASSEMBLY_USAGE_OCCURRENCE('Socket Head Cap Screw M6x25:30',
'Socket Head Cap Screw M6x25:30','Socket Head Cap Screw M6x25:30',#66931,
#66970,'Socket Head Cap Screw M6x25:30');
#1036=SHAPE_REPRESENTATION_RELATIONSHIP('SRR','None',#66891,#1067);
#1037=SHAPE_REPRESENTATION_RELATIONSHIP('SRR','None',#66893,#1068);
#1038=SHAPE_REPRESENTATION_RELATIONSHIP('SRR','None',#66894,#1069);
#1039=SHAPE_REPRESENTATION_RELATIONSHIP('SRR','None',#66896,#1070);
#1040=SHAPE_REPRESENTATION_RELATIONSHIP('SRR','None',#66897,#1071);
#1041=SHAPE_REPRESENTATION_RELATIONSHIP('SRR','None',#66898,#1072);
#1042=SHAPE_REPRESENTATION_RELATIONSHIP('SRR','None',#66900,#1073);
#1043=SHAPE_REPRESENTATION_RELATIONSHIP('SRR','None',#66901,#1074);
#1044=SHAPE_REPRESENTATION_RELATIONSHIP('SRR','None',#66902,#1075);
#1045=SHAPE_REPRESENTATION_RELATIONSHIP('SRR','None',#66904,#1076);
#1046=SHAPE_REPRESENTATION_RELATIONSHIP('SRR','None',#66905,#1077);
#1047=SHAPE_REPRESENTATION_RELATIONSHIP('SRR','None',#66907,#1078);
#1048=SHAPE_REPRESENTATION_RELATIONSHIP('SRR','None',#66908,#1079);
#1049=SHAPE_REPRESENTATION_RELATIONSHIP('SRR','None',#66910,#1080);
#1050=SHAPE_REPRESENTATION_RELATIONSHIP('SRR','None',#66911,#1081);
#1051=SHAPE_REPRESENTATION_RELATIONSHIP('SRR','None',#66912,#1082);
#1052=SHAPE_REPRESENTATION_RELATIONSHIP('SRR','None',#66913,#1083);
#1053=SHAPE_REPRESENTATION_RELATIONSHIP('SRR','None',#66916,#1084);
#1054=SHAPE_REPRESENTATION_RELATIONSHIP('SRR','None',#66917,#1085);
#1055=SHAPE_REPRESENTATION_RELATIONSHIP('SRR','None',#66918,#1086);
#1056=SHAPE_REPRESENTATION_RELATIONSHIP('SRR','None',#66919,#1087);
#1057=SHAPE_REPRESENTATION_RELATIONSHIP('SRR','None',#66920,#1088);
#1058=SHAPE_REPRESENTATION_RELATIONSHIP('SRR','None',#66921,#1089);
#1059=SHAPE_REPRESENTATION_RELATIONSHIP('SRR','None',#66922,#1090);
#1060=SHAPE_REPRESENTATION_RELATIONSHIP('SRR','None',#66923,#1091);
#1061=SHAPE_REPRESENTATION_RELATIONSHIP('SRR','None',#66924,#1092);
#1062=SHAPE_REPRESENTATION_RELATIONSHIP('SRR','None',#66925,#1093);
#1063=SHAPE_REPRESENTATION_RELATIONSHIP('SRR','None',#66926,#1094);
#1064=SHAPE_REPRESENTATION_RELATIONSHIP('SRR','None',#66927,#1095);
#1065=SHAPE_REPRESENTATION_RELATIONSHIP('SRR','None',#66928,#1096);
#1066=SHAPE_REPRESENTATION_RELATIONSHIP('SRR','None',#66929,#1097);
#1067=ADVANCED_BREP_SHAPE_REPRESENTATION('',(#1133),#66682);
#1068=ADVANCED_BREP_SHAPE_REPRESENTATION('',(#1134),#66684);
#1069=ADVANCED_BREP_SHAPE_REPRESENTATION('',(#1135),#66685);
#1070=ADVANCED_BREP_SHAPE_REPRESENTATION('',(#1136),#66687);
#1071=ADVANCED_BREP_SHAPE_REPRESENTATION('',(#1137),#66688);
#1072=ADVANCED_BREP_SHAPE_REPRESENTATION('',(#1138),#66689);
#1073=ADVANCED_BREP_SHAPE_REPRESENTATION('',(#1139),#66691);
#1074=ADVANCED_BREP_SHAPE_REPRESENTATION('',(#1140),#66692);
#1075=ADVANCED_BREP_SHAPE_REPRESENTATION('',(#1141),#66693);
#1076=ADVANCED_BREP_SHAPE_REPRESENTATION('',(#1142),#66695);
#1077=ADVANCED_BREP_SHAPE_REPRESENTATION('',(#1143),#66696);
#1078=ADVANCED_BREP_SHAPE_REPRESENTATION('',(#1144),#66698);
#1079=ADVANCED_BREP_SHAPE_REPRESENTATION('',(#1145),#66699);
#1080=ADVANCED_BREP_SHAPE_REPRESENTATION('',(#1146),#66701);
#1081=ADVANCED_BREP_SHAPE_REPRESENTATION('',(#1147),#66702);
#1082=ADVANCED_BREP_SHAPE_REPRESENTATION('',(#1148),#66703);
#1083=ADVANCED_BREP_SHAPE_REPRESENTATION('',(#1149),#66704);
#1084=ADVANCED_BREP_SHAPE_REPRESENTATION('',(#1150),#66707);
#1085=ADVANCED_BREP_SHAPE_REPRESENTATION('',(#1151),#66708);
#1086=ADVANCED_BREP_SHAPE_REPRESENTATION('',(#1152),#66709);
#1087=ADVANCED_BREP_SHAPE_REPRESENTATION('',(#1153),#66710);
#1088=ADVANCED_BREP_SHAPE_REPRESENTATION('',(#1154,#1155),#66711);
#1089=ADVANCED_BREP_SHAPE_REPRESENTATION('',(#1156),#66712);
#1090=ADVANCED_BREP_SHAPE_REPRESENTATION('',(#1157),#66713);
#1091=ADVANCED_BREP_SHAPE_REPRESENTATION('',(#1158),#66714);
#1092=ADVANCED_BREP_SHAPE_REPRESENTATION('',(#1159,#1160),#66715);
#1093=ADVANCED_BREP_SHAPE_REPRESENTATION('',(#1161),#66716);
#1094=ADVANCED_BREP_SHAPE_REPRESENTATION('',(#1162),#66717);
#1095=ADVANCED_BREP_SHAPE_REPRESENTATION('',(#1163,#1164,#1165),#66718);
#1096=ADVANCED_BREP_SHAPE_REPRESENTATION('',(#1166),#66719);
#1097=ADVANCED_BREP_SHAPE_REPRESENTATION('',(#1167),#66720);
#1098=STYLED_ITEM('',(#67095),#1133);
#1099=STYLED_ITEM('',(#67095),#1134);
#1100=STYLED_ITEM('',(#67095),#1135);
#1101=STYLED_ITEM('',(#67095),#1136);
#1102=STYLED_ITEM('',(#67095),#1137);
#1103=STYLED_ITEM('',(#67095),#1138);
#1104=STYLED_ITEM('',(#67095),#1139);
#1105=STYLED_ITEM('',(#67095),#1140);
#1106=STYLED_ITEM('',(#67095),#1141);
#1107=STYLED_ITEM('',(#67095),#1142);
#1108=STYLED_ITEM('',(#67095),#1143);
#1109=STYLED_ITEM('',(#67095),#1144);
#1110=STYLED_ITEM('',(#67095),#1145);
#1111=STYLED_ITEM('',(#67095),#1146);
#1112=STYLED_ITEM('',(#67095),#1147);
#1113=STYLED_ITEM('',(#67095),#1148);
#1114=STYLED_ITEM('',(#67095),#1149);
#1115=STYLED_ITEM('',(#67095),#1150);
#1116=STYLED_ITEM('',(#67095),#1151);
#1117=STYLED_ITEM('',(#67095),#1152);
#1118=STYLED_ITEM('',(#67095),#1153);
#1119=STYLED_ITEM('',(#67095),#1154);
#1120=STYLED_ITEM('',(#67095),#1155);
#1121=STYLED_ITEM('',(#67095),#1156);
#1122=STYLED_ITEM('',(#67095),#1157);
#1123=STYLED_ITEM('',(#67095),#1158);
#1124=STYLED_ITEM('',(#67095),#1159);
#1125=STYLED_ITEM('',(#67095),#1160);
#1126=STYLED_ITEM('',(#67095),#1161);
#1127=STYLED_ITEM('',(#67095),#1162);
#1128=STYLED_ITEM('',(#67095),#1163);
#1129=STYLED_ITEM('',(#67095),#1164);
#1130=STYLED_ITEM('',(#67095),#1165);
#1131=STYLED_ITEM('',(#67095),#1166);
#1132=STYLED_ITEM('',(#67095),#1167);
#1133=MANIFOLD_SOLID_BREP('Body1',#25664);
#1134=MANIFOLD_SOLID_BREP('Body1',#25665);
#1135=MANIFOLD_SOLID_BREP('Body1',#25666);
#1136=MANIFOLD_SOLID_BREP('Body1',#25667);
#1137=MANIFOLD_SOLID_BREP('Body1',#25668);
#1138=MANIFOLD_SOLID_BREP('Body1',#25669);
#1139=MANIFOLD_SOLID_BREP('Body1',#25670);
#1140=MANIFOLD_SOLID_BREP('Body1',#25671);
#1141=MANIFOLD_SOLID_BREP('Body1',#25672);
#1142=MANIFOLD_SOLID_BREP('Body1',#25673);
#1143=MANIFOLD_SOLID_BREP('Body1',#25674);
#1144=MANIFOLD_SOLID_BREP('Body1',#25675);
#1145=MANIFOLD_SOLID_BREP('Body1',#25676);
#1146=MANIFOLD_SOLID_BREP('Body1',#25677);
#1147=MANIFOLD_SOLID_BREP('Body1',#25678);
#1148=MANIFOLD_SOLID_BREP('Body1',#25679);
#1149=MANIFOLD_SOLID_BREP('Body1',#25680);
#1150=MANIFOLD_SOLID_BREP('Body1',#25681);
#1151=MANIFOLD_SOLID_BREP('Body1',#25682);
#1152=MANIFOLD_SOLID_BREP('Body1',#25683);
#1153=MANIFOLD_SOLID_BREP('Body1',#25684);
#1154=MANIFOLD_SOLID_BREP('Body1',#25685);
#1155=MANIFOLD_SOLID_BREP('Body2',#25686);
#1156=MANIFOLD_SOLID_BREP('Body1',#25687);
#1157=MANIFOLD_SOLID_BREP('Body1',#25688);
#1158=MANIFOLD_SOLID_BREP('Body1',#25689);
#1159=MANIFOLD_SOLID_BREP('Body1',#25690);
#1160=MANIFOLD_SOLID_BREP('Body2',#25691);
#1161=MANIFOLD_SOLID_BREP('Body1',#25692);
#1162=MANIFOLD_SOLID_BREP('Body1',#25693);
#1163=MANIFOLD_SOLID_BREP('Body1',#25694);
#1164=MANIFOLD_SOLID_BREP('Body2',#25695);
#1165=MANIFOLD_SOLID_BREP('Body3',#25696);
#1166=MANIFOLD_SOLID_BREP('Body1',#25697);
#1167=MANIFOLD_SOLID_BREP('Body1',#25698);
#1168=FACE_BOUND('',#3720,.T.);
#1169=FACE_BOUND('',#3721,.T.);
#1170=FACE_BOUND('',#3722,.T.);
#1171=FACE_BOUND('',#3723,.T.);
#1172=FACE_BOUND('',#3724,.T.);
#1173=FACE_BOUND('',#3725,.T.);
#1174=FACE_BOUND('',#3727,.T.);
#1175=FACE_BOUND('',#3728,.T.);
#1176=FACE_BOUND('',#3729,.T.);
#1177=FACE_BOUND('',#3730,.T.);
#1178=FACE_BOUND('',#3731,.T.);
#1179=FACE_BOUND('',#3732,.T.);
#1180=FACE_BOUND('',#3752,.T.);
#1181=FACE_BOUND('',#3753,.T.);
#1182=FACE_BOUND('',#3754,.T.);
#1183=FACE_BOUND('',#3755,.T.);
#1184=FACE_BOUND('',#3761,.T.);
#1185=FACE_BOUND('',#3762,.T.);
#1186=FACE_BOUND('',#3763,.T.);
#1187=FACE_BOUND('',#3764,.T.);
#1188=FACE_BOUND('',#3778,.T.);
#1189=FACE_BOUND('',#3779,.T.);
#1190=FACE_BOUND('',#3780,.T.);
#1191=FACE_BOUND('',#3781,.T.);
#1192=FACE_BOUND('',#3782,.T.);
#1193=FACE_BOUND('',#3783,.T.);
#1194=FACE_BOUND('',#3784,.T.);
#1195=FACE_BOUND('',#3785,.T.);
#1196=FACE_BOUND('',#3786,.T.);
#1197=FACE_BOUND('',#3792,.T.);
#1198=FACE_BOUND('',#3793,.T.);
#1199=FACE_BOUND('',#3794,.T.);
#1200=FACE_BOUND('',#3795,.T.);
#1201=FACE_BOUND('',#3796,.T.);
#1202=FACE_BOUND('',#3797,.T.);
#1203=FACE_BOUND('',#3798,.T.);
#1204=FACE_BOUND('',#3799,.T.);
#1205=FACE_BOUND('',#3800,.T.);
#1206=FACE_BOUND('',#3802,.T.);
#1207=FACE_BOUND('',#3804,.T.);
#1208=FACE_BOUND('',#3806,.T.);
#1209=FACE_BOUND('',#3815,.T.);
#1210=FACE_BOUND('',#3816,.T.);
#1211=FACE_BOUND('',#3817,.T.);
#1212=FACE_BOUND('',#3818,.T.);
#1213=FACE_BOUND('',#3819,.T.);
#1214=FACE_BOUND('',#3820,.T.);
#1215=FACE_BOUND('',#3821,.T.);
#1216=FACE_BOUND('',#3824,.T.);
#1217=FACE_BOUND('',#3825,.T.);
#1218=FACE_BOUND('',#3826,.T.);
#1219=FACE_BOUND('',#3827,.T.);
#1220=FACE_BOUND('',#3828,.T.);
#1221=FACE_BOUND('',#3829,.T.);
#1222=FACE_BOUND('',#3830,.T.);
#1223=FACE_BOUND('',#3847,.T.);
#1224=FACE_BOUND('',#3848,.T.);
#1225=FACE_BOUND('',#3849,.T.);
#1226=FACE_BOUND('',#3850,.T.);
#1227=FACE_BOUND('',#3851,.T.);
#1228=FACE_BOUND('',#3852,.T.);
#1229=FACE_BOUND('',#3854,.T.);
#1230=FACE_BOUND('',#3855,.T.);
#1231=FACE_BOUND('',#3856,.T.);
#1232=FACE_BOUND('',#3857,.T.);
#1233=FACE_BOUND('',#3858,.T.);
#1234=FACE_BOUND('',#3859,.T.);
#1235=FACE_BOUND('',#3871,.T.);
#1236=FACE_BOUND('',#3872,.T.);
#1237=FACE_BOUND('',#3873,.T.);
#1238=FACE_BOUND('',#3874,.T.);
#1239=FACE_BOUND('',#3875,.T.);
#1240=FACE_BOUND('',#3876,.T.);
#1241=FACE_BOUND('',#3878,.T.);
#1242=FACE_BOUND('',#3879,.T.);
#1243=FACE_BOUND('',#3880,.T.);
#1244=FACE_BOUND('',#3881,.T.);
#1245=FACE_BOUND('',#3882,.T.);
#1246=FACE_BOUND('',#3883,.T.);
#1247=FACE_BOUND('',#3970,.T.);
#1248=FACE_BOUND('',#3971,.T.);
#1249=FACE_BOUND('',#3972,.T.);
#1250=FACE_BOUND('',#3973,.T.);
#1251=FACE_BOUND('',#3974,.T.);
#1252=FACE_BOUND('',#3975,.T.);
#1253=FACE_BOUND('',#3976,.T.);
#1254=FACE_BOUND('',#3977,.T.);
#1255=FACE_BOUND('',#3978,.T.);
#1256=FACE_BOUND('',#3979,.T.);
#1257=FACE_BOUND('',#3980,.T.);
#1258=FACE_BOUND('',#3981,.T.);
#1259=FACE_BOUND('',#3982,.T.);
#1260=FACE_BOUND('',#3983,.T.);
#1261=FACE_BOUND('',#3984,.T.);
#1262=FACE_BOUND('',#4023,.T.);
#1263=FACE_BOUND('',#4025,.T.);
#1264=FACE_BOUND('',#4027,.T.);
#1265=FACE_BOUND('',#4029,.T.);
#1266=FACE_BOUND('',#4031,.T.);
#1267=FACE_BOUND('',#4033,.T.);
#1268=FACE_BOUND('',#4035,.T.);
#1269=FACE_BOUND('',#4037,.T.);
#1270=FACE_BOUND('',#4039,.T.);
#1271=FACE_BOUND('',#4041,.T.);
#1272=FACE_BOUND('',#4043,.T.);
#1273=FACE_BOUND('',#4045,.T.);
#1274=FACE_BOUND('',#4047,.T.);
#1275=FACE_BOUND('',#4049,.T.);
#1276=FACE_BOUND('',#4051,.T.);
#1277=FACE_BOUND('',#4113,.T.);
#1278=FACE_BOUND('',#4116,.T.);
#1279=FACE_BOUND('',#4131,.T.);
#1280=FACE_BOUND('',#4229,.T.);
#1281=FACE_BOUND('',#4242,.T.);
#1282=FACE_BOUND('',#4250,.T.);
#1283=FACE_BOUND('',#4253,.T.);
#1284=FACE_BOUND('',#4258,.T.);
#1285=FACE_BOUND('',#4306,.T.);
#1286=FACE_BOUND('',#4311,.T.);
#1287=FACE_BOUND('',#4313,.T.);
#1288=FACE_BOUND('',#4320,.T.);
#1289=FACE_BOUND('',#4321,.T.);
#1290=FACE_BOUND('',#4330,.T.);
#1291=FACE_BOUND('',#4331,.T.);
#1292=FACE_BOUND('',#4337,.T.);
#1293=FACE_BOUND('',#4343,.T.);
#1294=FACE_BOUND('',#4350,.T.);
#1295=FACE_BOUND('',#4355,.T.);
#1296=FACE_BOUND('',#4390,.T.);
#1297=FACE_BOUND('',#4402,.T.);
#1298=FACE_BOUND('',#4404,.T.);
#1299=FACE_BOUND('',#4423,.T.);
#1300=FACE_BOUND('',#4425,.T.);
#1301=FACE_BOUND('',#4456,.T.);
#1302=FACE_BOUND('',#4471,.T.);
#1303=FACE_BOUND('',#4473,.T.);
#1304=FACE_BOUND('',#4475,.T.);
#1305=FACE_BOUND('',#4477,.T.);
#1306=FACE_BOUND('',#4479,.T.);
#1307=FACE_BOUND('',#4498,.T.);
#1308=FACE_BOUND('',#4503,.T.);
#1309=FACE_BOUND('',#4504,.T.);
#1310=FACE_BOUND('',#4505,.T.);
#1311=FACE_BOUND('',#4506,.T.);
#1312=FACE_BOUND('',#4507,.T.);
#1313=FACE_BOUND('',#4508,.T.);
#1314=FACE_BOUND('',#4509,.T.);
#1315=FACE_BOUND('',#4513,.T.);
#1316=FACE_BOUND('',#4518,.T.);
#1317=FACE_BOUND('',#4519,.T.);
#1318=FACE_BOUND('',#4520,.T.);
#1319=FACE_BOUND('',#4521,.T.);
#1320=FACE_BOUND('',#4522,.T.);
#1321=FACE_BOUND('',#4523,.T.);
#1322=FACE_BOUND('',#4524,.T.);
#1323=FACE_BOUND('',#4526,.T.);
#1324=FACE_BOUND('',#4528,.T.);
#1325=FACE_BOUND('',#4530,.T.);
#1326=FACE_BOUND('',#4532,.T.);
#1327=FACE_BOUND('',#4534,.T.);
#1328=FACE_BOUND('',#4545,.T.);
#1329=FACE_BOUND('',#4549,.T.);
#1330=FACE_BOUND('',#4550,.T.);
#1331=FACE_BOUND('',#4554,.T.);
#1332=FACE_BOUND('',#4561,.T.);
#1333=FACE_BOUND('',#4563,.T.);
#1334=FACE_BOUND('',#4565,.T.);
#1335=FACE_BOUND('',#4567,.T.);
#1336=FACE_BOUND('',#4569,.T.);
#1337=FACE_BOUND('',#4571,.T.);
#1338=FACE_BOUND('',#4577,.T.);
#1339=FACE_BOUND('',#4578,.T.);
#1340=FACE_BOUND('',#4580,.T.);
#1341=FACE_BOUND('',#4581,.T.);
#1342=FACE_BOUND('',#4614,.T.);
#1343=FACE_BOUND('',#4616,.T.);
#1344=FACE_BOUND('',#4618,.T.);
#1345=FACE_BOUND('',#4620,.T.);
#1346=FACE_BOUND('',#4622,.T.);
#1347=FACE_BOUND('',#4624,.T.);
#1348=FACE_BOUND('',#4625,.T.);
#1349=FACE_BOUND('',#4629,.T.);
#1350=FACE_BOUND('',#4630,.T.);
#1351=FACE_BOUND('',#4631,.T.);
#1352=FACE_BOUND('',#4632,.T.);
#1353=FACE_BOUND('',#4636,.T.);
#1354=FACE_BOUND('',#4637,.T.);
#1355=FACE_BOUND('',#4644,.T.);
#1356=FACE_BOUND('',#4646,.T.);
#1357=FACE_BOUND('',#4648,.T.);
#1358=FACE_BOUND('',#4650,.T.);
#1359=FACE_BOUND('',#4652,.T.);
#1360=FACE_BOUND('',#4654,.T.);
#1361=FACE_BOUND('',#4655,.T.);
#1362=FACE_BOUND('',#4656,.T.);
#1363=FACE_BOUND('',#4657,.T.);
#1364=FACE_BOUND('',#4658,.T.);
#1365=FACE_BOUND('',#4668,.T.);
#1366=FACE_BOUND('',#4670,.T.);
#1367=FACE_BOUND('',#4672,.T.);
#1368=FACE_BOUND('',#4674,.T.);
#1369=FACE_BOUND('',#4704,.T.);
#1370=FACE_BOUND('',#4706,.T.);
#1371=FACE_BOUND('',#4708,.T.);
#1372=FACE_BOUND('',#4710,.T.);
#1373=FACE_BOUND('',#4721,.T.);
#1374=FACE_BOUND('',#4723,.T.);
#1375=FACE_BOUND('',#4725,.T.);
#1376=FACE_BOUND('',#4729,.T.);
#1377=FACE_BOUND('',#4731,.T.);
#1378=FACE_BOUND('',#4733,.T.);
#1379=FACE_BOUND('',#4754,.T.);
#1380=FACE_BOUND('',#4756,.T.);
#1381=FACE_BOUND('',#4770,.T.);
#1382=FACE_BOUND('',#4771,.T.);
#1383=FACE_BOUND('',#4772,.T.);
#1384=FACE_BOUND('',#4773,.T.);
#1385=FACE_BOUND('',#4774,.T.);
#1386=FACE_BOUND('',#4775,.T.);
#1387=FACE_BOUND('',#4781,.T.);
#1388=FACE_BOUND('',#4782,.T.);
#1389=FACE_BOUND('',#4783,.T.);
#1390=FACE_BOUND('',#4784,.T.);
#1391=FACE_BOUND('',#4785,.T.);
#1392=FACE_BOUND('',#4786,.T.);
#1393=FACE_BOUND('',#4974,.T.);
#1394=FACE_BOUND('',#4975,.T.);
#1395=FACE_BOUND('',#4976,.T.);
#1396=FACE_BOUND('',#4977,.T.);
#1397=FACE_BOUND('',#4978,.T.);
#1398=FACE_BOUND('',#4987,.T.);
#1399=FACE_BOUND('',#4988,.T.);
#1400=FACE_BOUND('',#4989,.T.);
#1401=FACE_BOUND('',#4990,.T.);
#1402=FACE_BOUND('',#4991,.T.);
#1403=FACE_BOUND('',#4993,.T.);
#1404=FACE_BOUND('',#5004,.T.);
#1405=FACE_BOUND('',#5008,.T.);
#1406=FACE_BOUND('',#5020,.T.);
#1407=FACE_BOUND('',#5024,.T.);
#1408=FACE_BOUND('',#5046,.T.);
#1409=FACE_BOUND('',#5047,.T.);
#1410=FACE_BOUND('',#5052,.T.);
#1411=FACE_BOUND('',#5055,.T.);
#1412=FACE_BOUND('',#5058,.T.);
#1413=FACE_BOUND('',#5060,.T.);
#1414=FACE_BOUND('',#5064,.T.);
#1415=FACE_BOUND('',#5068,.T.);
#1416=FACE_BOUND('',#5071,.T.);
#1417=FACE_BOUND('',#5073,.T.);
#1418=FACE_BOUND('',#5096,.T.);
#1419=FACE_BOUND('',#5097,.T.);
#1420=FACE_BOUND('',#5098,.T.);
#1421=FACE_BOUND('',#5099,.T.);
#1422=FACE_BOUND('',#5100,.T.);
#1423=FACE_BOUND('',#5101,.T.);
#1424=FACE_BOUND('',#5102,.T.);
#1425=FACE_BOUND('',#5103,.T.);
#1426=FACE_BOUND('',#5153,.T.);
#1427=FACE_BOUND('',#5155,.T.);
#1428=FACE_BOUND('',#5166,.T.);
#1429=FACE_BOUND('',#5170,.T.);
#1430=FACE_BOUND('',#5182,.T.);
#1431=FACE_BOUND('',#5186,.T.);
#1432=FACE_BOUND('',#5208,.T.);
#1433=FACE_BOUND('',#5209,.T.);
#1434=FACE_BOUND('',#5214,.T.);
#1435=FACE_BOUND('',#5217,.T.);
#1436=FACE_BOUND('',#5220,.T.);
#1437=FACE_BOUND('',#5222,.T.);
#1438=FACE_BOUND('',#5226,.T.);
#1439=FACE_BOUND('',#5230,.T.);
#1440=FACE_BOUND('',#5233,.T.);
#1441=FACE_BOUND('',#5235,.T.);
#1442=FACE_BOUND('',#5246,.T.);
#1443=FACE_BOUND('',#5256,.T.);
#1444=FACE_BOUND('',#5257,.T.);
#1445=FACE_BOUND('',#5258,.T.);
#1446=FACE_BOUND('',#5259,.T.);
#1447=FACE_BOUND('',#5260,.T.);
#1448=FACE_BOUND('',#5261,.T.);
#1449=FACE_BOUND('',#5262,.T.);
#1450=FACE_BOUND('',#5263,.T.);
#1451=FACE_BOUND('',#5313,.T.);
#1452=FACE_BOUND('',#5357,.T.);
#1453=FACE_BOUND('',#5358,.T.);
#1454=FACE_BOUND('',#5359,.T.);
#1455=FACE_BOUND('',#5360,.T.);
#1456=FACE_BOUND('',#5361,.T.);
#1457=FACE_BOUND('',#5362,.T.);
#1458=FACE_BOUND('',#5363,.T.);
#1459=FACE_BOUND('',#5364,.T.);
#1460=FACE_BOUND('',#5365,.T.);
#1461=FACE_BOUND('',#5366,.T.);
#1462=FACE_BOUND('',#5367,.T.);
#1463=FACE_BOUND('',#5368,.T.);
#1464=FACE_BOUND('',#5369,.T.);
#1465=FACE_BOUND('',#5370,.T.);
#1466=FACE_BOUND('',#5371,.T.);
#1467=FACE_BOUND('',#5372,.T.);
#1468=FACE_BOUND('',#5373,.T.);
#1469=FACE_BOUND('',#5383,.T.);
#1470=FACE_BOUND('',#5385,.T.);
#1471=FACE_BOUND('',#5399,.T.);
#1472=FACE_BOUND('',#5402,.T.);
#1473=FACE_BOUND('',#5404,.T.);
#1474=FACE_BOUND('',#5420,.T.);
#1475=FACE_BOUND('',#5422,.T.);
#1476=FACE_BOUND('',#5440,.T.);
#1477=FACE_BOUND('',#5441,.T.);
#1478=FACE_BOUND('',#5442,.T.);
#1479=FACE_BOUND('',#5443,.T.);
#1480=FACE_BOUND('',#5444,.T.);
#1481=FACE_BOUND('',#5445,.T.);
#1482=FACE_BOUND('',#5446,.T.);
#1483=FACE_BOUND('',#5447,.T.);
#1484=FACE_BOUND('',#5448,.T.);
#1485=FACE_BOUND('',#5449,.T.);
#1486=FACE_BOUND('',#5455,.T.);
#1487=FACE_BOUND('',#5456,.T.);
#1488=FACE_BOUND('',#5457,.T.);
#1489=FACE_BOUND('',#5458,.T.);
#1490=FACE_BOUND('',#5459,.T.);
#1491=FACE_BOUND('',#5460,.T.);
#1492=FACE_BOUND('',#5461,.T.);
#1493=FACE_BOUND('',#5462,.T.);
#1494=FACE_BOUND('',#5463,.T.);
#1495=FACE_BOUND('',#5464,.T.);
#1496=FACE_BOUND('',#5473,.T.);
#1497=FACE_BOUND('',#5475,.T.);
#1498=PLANE('',#26055);
#1499=PLANE('',#26056);
#1500=PLANE('',#26057);
#1501=PLANE('',#26058);
#1502=PLANE('',#26059);
#1503=PLANE('',#26060);
#1504=PLANE('',#26061);
#1505=PLANE('',#26062);
#1506=PLANE('',#26063);
#1507=PLANE('',#26064);
#1508=PLANE('',#26065);
#1509=PLANE('',#26066);
#1510=PLANE('',#26067);
#1511=PLANE('',#26068);
#1512=PLANE('',#26083);
#1513=PLANE('',#26084);
#1514=PLANE('',#26085);
#1515=PLANE('',#26086);
#1516=PLANE('',#26087);
#1517=PLANE('',#26088);
#1518=PLANE('',#26089);
#1519=PLANE('',#26090);
#1520=PLANE('',#26091);
#1521=PLANE('',#26092);
#1522=PLANE('',#26093);
#1523=PLANE('',#26094);
#1524=PLANE('',#26132);
#1525=PLANE('',#26133);
#1526=PLANE('',#26134);
#1527=PLANE('',#26135);
#1528=PLANE('',#26136);
#1529=PLANE('',#26137);
#1530=PLANE('',#26138);
#1531=PLANE('',#26139);
#1532=PLANE('',#26140);
#1533=PLANE('',#26164);
#1534=PLANE('',#26167);
#1535=PLANE('',#26168);
#1536=PLANE('',#26171);
#1537=PLANE('',#26172);
#1538=PLANE('',#26173);
#1539=PLANE('',#26195);
#1540=PLANE('',#26196);
#1541=PLANE('',#26197);
#1542=PLANE('',#26198);
#1543=PLANE('',#26199);
#1544=PLANE('',#26200);
#1545=PLANE('',#26222);
#1546=PLANE('',#26223);
#1547=PLANE('',#26224);
#1548=PLANE('',#26225);
#1549=PLANE('',#26226);
#1550=PLANE('',#26227);
#1551=PLANE('',#26440);
#1552=PLANE('',#26441);
#1553=PLANE('',#26442);
#1554=PLANE('',#26443);
#1555=PLANE('',#26444);
#1556=PLANE('',#26445);
#1557=PLANE('',#26446);
#1558=PLANE('',#26447);
#1559=PLANE('',#26448);
#1560=PLANE('',#26449);
#1561=PLANE('',#26450);
#1562=PLANE('',#26451);
#1563=PLANE('',#26452);
#1564=PLANE('',#26453);
#1565=PLANE('',#26454);
#1566=PLANE('',#26455);
#1567=PLANE('',#26456);
#1568=PLANE('',#26457);
#1569=PLANE('',#26458);
#1570=PLANE('',#26459);
#1571=PLANE('',#26460);
#1572=PLANE('',#26461);
#1573=PLANE('',#26462);
#1574=PLANE('',#26463);
#1575=PLANE('',#26464);
#1576=PLANE('',#26465);
#1577=PLANE('',#26466);
#1578=PLANE('',#26467);
#1579=PLANE('',#26468);
#1580=PLANE('',#26469);
#1581=PLANE('',#26470);
#1582=PLANE('',#26471);
#1583=PLANE('',#26472);
#1584=PLANE('',#26473);
#1585=PLANE('',#26474);
#1586=PLANE('',#26475);
#1587=PLANE('',#26476);
#1588=PLANE('',#26477);
#1589=PLANE('',#26478);
#1590=PLANE('',#26479);
#1591=PLANE('',#26480);
#1592=PLANE('',#26481);
#1593=PLANE('',#26482);
#1594=PLANE('',#26483);
#1595=PLANE('',#26484);
#1596=PLANE('',#26485);
#1597=PLANE('',#26486);
#1598=PLANE('',#26487);
#1599=PLANE('',#26510);
#1600=PLANE('',#26533);
#1601=PLANE('',#26534);
#1602=PLANE('',#26535);
#1603=PLANE('',#26536);
#1604=PLANE('',#26537);
#1605=PLANE('',#26538);
#1606=PLANE('',#26539);
#1607=PLANE('',#26540);
#1608=PLANE('',#26541);
#1609=PLANE('',#26542);
#1610=PLANE('',#26543);
#1611=PLANE('',#26544);
#1612=PLANE('',#26545);
#1613=PLANE('',#26546);
#1614=PLANE('',#26558);
#1615=PLANE('',#26559);
#1616=PLANE('',#26560);
#1617=PLANE('',#26561);
#1618=PLANE('',#26562);
#1619=PLANE('',#26574);
#1620=PLANE('',#26575);
#1621=PLANE('',#26576);
#1622=PLANE('',#26577);
#1623=PLANE('',#26578);
#1624=PLANE('',#26579);
#1625=PLANE('',#26580);
#1626=PLANE('',#26581);
#1627=PLANE('',#26582);
#1628=PLANE('',#26583);
#1629=PLANE('',#26584);
#1630=PLANE('',#26585);
#1631=PLANE('',#26586);
#1632=PLANE('',#26587);
#1633=PLANE('',#26588);
#1634=PLANE('',#26589);
#1635=PLANE('',#26590);
#1636=PLANE('',#26591);
#1637=PLANE('',#26642);
#1638=PLANE('',#26644);
#1639=PLANE('',#26647);
#1640=PLANE('',#26650);
#1641=PLANE('',#26652);
#1642=PLANE('',#26653);
#1643=PLANE('',#26654);
#1644=PLANE('',#26655);
#1645=PLANE('',#26656);
#1646=PLANE('',#26657);
#1647=PLANE('',#26658);
#1648=PLANE('',#26659);
#1649=PLANE('',#26660);
#1650=PLANE('',#26661);
#1651=PLANE('',#26662);
#1652=PLANE('',#26663);
#1653=PLANE('',#26664);
#1654=PLANE('',#26665);
#1655=PLANE('',#26666);
#1656=PLANE('',#26667);
#1657=PLANE('',#26668);
#1658=PLANE('',#26729);
#1659=PLANE('',#26730);
#1660=PLANE('',#26731);
#1661=PLANE('',#26732);
#1662=PLANE('',#26733);
#1663=PLANE('',#26734);
#1664=PLANE('',#26735);
#1665=PLANE('',#26736);
#1666=PLANE('',#26737);
#1667=PLANE('',#26738);
#1668=PLANE('',#26739);
#1669=PLANE('',#26740);
#1670=PLANE('',#26741);
#1671=PLANE('',#26742);
#1672=PLANE('',#26743);
#1673=PLANE('',#26744);
#1674=PLANE('',#26745);
#1675=PLANE('',#26766);
#1676=PLANE('',#26769);
#1677=PLANE('',#26772);
#1678=PLANE('',#26779);
#1679=PLANE('',#26782);
#1680=PLANE('',#26785);
#1681=PLANE('',#26792);
#1682=PLANE('',#26793);
#1683=PLANE('',#26794);
#1684=PLANE('',#26801);
#1685=PLANE('',#26804);
#1686=PLANE('',#26807);
#1687=PLANE('',#26814);
#1688=PLANE('',#26817);
#1689=PLANE('',#26820);
#1690=PLANE('',#26821);
#1691=PLANE('',#26822);
#1692=PLANE('',#26823);
#1693=PLANE('',#26824);
#1694=PLANE('',#26825);
#1695=PLANE('',#26826);
#1696=PLANE('',#26827);
#1697=PLANE('',#26828);
#1698=PLANE('',#26829);
#1699=PLANE('',#26830);
#1700=PLANE('',#26831);
#1701=PLANE('',#26833);
#1702=PLANE('',#26855);
#1703=PLANE('',#26856);
#1704=PLANE('',#26859);
#1705=PLANE('',#26860);
#1706=PLANE('',#26862);
#1707=PLANE('',#26863);
#1708=PLANE('',#26864);
#1709=PLANE('',#26865);
#1710=PLANE('',#26866);
#1711=PLANE('',#26867);
#1712=PLANE('',#26868);
#1713=PLANE('',#26869);
#1714=PLANE('',#26870);
#1715=PLANE('',#26871);
#1716=PLANE('',#26874);
#1717=PLANE('',#26877);
#1718=PLANE('',#26884);
#1719=PLANE('',#26887);
#1720=PLANE('',#26890);
#1721=PLANE('',#26897);
#1722=PLANE('',#26898);
#1723=PLANE('',#26899);
#1724=PLANE('',#26906);
#1725=PLANE('',#26909);
#1726=PLANE('',#26912);
#1727=PLANE('',#26919);
#1728=PLANE('',#26922);
#1729=PLANE('',#26925);
#1730=PLANE('',#26926);
#1731=PLANE('',#26927);
#1732=PLANE('',#26928);
#1733=PLANE('',#26929);
#1734=PLANE('',#26930);
#1735=PLANE('',#26936);
#1736=PLANE('',#26937);
#1737=PLANE('',#26938);
#1738=PLANE('',#26939);
#1739=PLANE('',#26943);
#1740=PLANE('',#26964);
#1741=PLANE('',#26965);
#1742=PLANE('',#26966);
#1743=PLANE('',#26967);
#1744=PLANE('',#26968);
#1745=PLANE('',#26969);
#1746=PLANE('',#26970);
#1747=PLANE('',#26971);
#1748=PLANE('',#26974);
#1749=PLANE('',#26976);
#1750=PLANE('',#26977);
#1751=PLANE('',#26979);
#1752=PLANE('',#26980);
#1753=PLANE('',#26982);
#1754=PLANE('',#26984);
#1755=PLANE('',#26987);
#1756=PLANE('',#26988);
#1757=PLANE('',#26989);
#1758=PLANE('',#26990);
#1759=PLANE('',#26991);
#1760=PLANE('',#26992);
#1761=PLANE('',#26993);
#1762=PLANE('',#26994);
#1763=PLANE('',#26995);
#1764=PLANE('',#26996);
#1765=PLANE('',#26999);
#1766=PLANE('',#27002);
#1767=PLANE('',#27009);
#1768=PLANE('',#27012);
#1769=PLANE('',#27015);
#1770=PLANE('',#27022);
#1771=PLANE('',#27023);
#1772=PLANE('',#27024);
#1773=PLANE('',#27031);
#1774=PLANE('',#27034);
#1775=PLANE('',#27037);
#1776=PLANE('',#27044);
#1777=PLANE('',#27047);
#1778=PLANE('',#27050);
#1779=PLANE('',#27051);
#1780=PLANE('',#27052);
#1781=PLANE('',#27053);
#1782=PLANE('',#27054);
#1783=PLANE('',#27055);
#1784=PLANE('',#27056);
#1785=PLANE('',#27057);
#1786=PLANE('',#27058);
#1787=PLANE('',#27059);
#1788=PLANE('',#27060);
#1789=PLANE('',#27061);
#1790=PLANE('',#27062);
#1791=PLANE('',#27063);
#1792=PLANE('',#27064);
#1793=PLANE('',#27065);
#1794=PLANE('',#27066);
#1795=PLANE('',#27067);
#1796=PLANE('',#27068);
#1797=PLANE('',#27069);
#1798=PLANE('',#27070);
#1799=PLANE('',#27071);
#1800=PLANE('',#27072);
#1801=PLANE('',#27073);
#1802=PLANE('',#27074);
#1803=PLANE('',#27075);
#1804=PLANE('',#27077);
#1805=PLANE('',#27078);
#1806=PLANE('',#27080);
#1807=PLANE('',#27082);
#1808=PLANE('',#27083);
#1809=PLANE('',#27085);
#1810=PLANE('',#27087);
#1811=PLANE('',#27088);
#1812=PLANE('',#27089);
#1813=PLANE('',#27090);
#1814=PLANE('',#27092);
#1815=PLANE('',#27113);
#1816=PLANE('',#27114);
#1817=PLANE('',#27115);
#1818=PLANE('',#27116);
#1819=PLANE('',#27117);
#1820=PLANE('',#27118);
#1821=PLANE('',#27123);
#1822=PLANE('',#27124);
#1823=PLANE('',#27125);
#1824=PLANE('',#27136);
#1825=PLANE('',#27137);
#1826=PLANE('',#27144);
#1827=PLANE('',#27145);
#1828=PLANE('',#27156);
#1829=PLANE('',#27157);
#1830=PLANE('',#27158);
#1831=PLANE('',#27169);
#1832=PLANE('',#27170);
#1833=PLANE('',#27171);
#1834=PLANE('',#27172);
#1835=PLANE('',#27173);
#1836=PLANE('',#27174);
#1837=PLANE('',#27175);
#1838=PLANE('',#27176);
#1839=PLANE('',#27177);
#1840=PLANE('',#27178);
#1841=PLANE('',#27179);
#1842=PLANE('',#27180);
#1843=PLANE('',#27181);
#1844=PLANE('',#27182);
#1845=PLANE('',#27183);
#1846=PLANE('',#27186);
#1847=PLANE('',#27187);
#1848=PLANE('',#27222);
#1849=PLANE('',#27228);
#1850=PLANE('',#27234);
#1851=PLANE('',#27235);
#1852=PLANE('',#27236);
#1853=PLANE('',#27237);
#1854=PLANE('',#27238);
#1855=PLANE('',#27239);
#1856=PLANE('',#27240);
#1857=PLANE('',#27241);
#1858=PLANE('',#27242);
#1859=PLANE('',#27243);
#1860=PLANE('',#27244);
#1861=PLANE('',#27245);
#1862=PLANE('',#27246);
#1863=PLANE('',#27257);
#1864=PLANE('',#27258);
#1865=PLANE('',#27259);
#1866=PLANE('',#27260);
#1867=PLANE('',#27261);
#1868=PLANE('',#27262);
#1869=PLANE('',#27263);
#1870=PLANE('',#27314);
#1871=PLANE('',#27315);
#1872=PLANE('',#27316);
#1873=PLANE('',#27317);
#1874=PLANE('',#27318);
#1875=PLANE('',#27321);
#1876=PLANE('',#27322);
#1877=PLANE('',#27323);
#1878=PLANE('',#27324);
#1879=PLANE('',#27325);
#1880=PLANE('',#27369);
#1881=PLANE('',#27384);
#1882=PLANE('',#27385);
#1883=PLANE('',#27386);
#1884=PLANE('',#27387);
#1885=PLANE('',#27388);
#1886=PLANE('',#27389);
#1887=PLANE('',#27390);
#1888=PLANE('',#27391);
#1889=PLANE('',#27417);
#1890=PLANE('',#27418);
#1891=PLANE('',#27419);
#1892=PLANE('',#27420);
#1893=PLANE('',#27421);
#1894=PLANE('',#27422);
#1895=PLANE('',#27423);
#1896=PLANE('',#27424);
#1897=PLANE('',#27425);
#1898=PLANE('',#27426);
#1899=PLANE('',#27427);
#1900=PLANE('',#27428);
#1901=PLANE('',#27429);
#1902=PLANE('',#27430);
#1903=PLANE('',#27431);
#1904=PLANE('',#27432);
#1905=PLANE('',#27433);
#1906=PLANE('',#27434);
#1907=PLANE('',#27448);
#1908=PLANE('',#27453);
#1909=PLANE('',#27458);
#1910=PLANE('',#27460);
#1911=PLANE('',#27463);
#1912=PLANE('',#27465);
#1913=PLANE('',#27466);
#1914=PLANE('',#27467);
#1915=PLANE('',#27535);
#1916=PLANE('',#27536);
#1917=PLANE('',#27537);
#1918=PLANE('',#27538);
#1919=PLANE('',#27539);
#1920=PLANE('',#27540);
#1921=PLANE('',#27541);
#1922=PLANE('',#27542);
#1923=PLANE('',#27543);
#1924=PLANE('',#27544);
#1925=PLANE('',#27545);
#1926=PLANE('',#27546);
#1927=PLANE('',#27547);
#1928=PLANE('',#27548);
#1929=PLANE('',#27549);
#1930=PLANE('',#27550);
#1931=PLANE('',#27551);
#1932=PLANE('',#27552);
#1933=PLANE('',#27553);
#1934=PLANE('',#27554);
#1935=PLANE('',#27555);
#1936=PLANE('',#27556);
#1937=PLANE('',#27557);
#1938=PLANE('',#27558);
#1939=PLANE('',#27559);
#1940=PLANE('',#27560);
#1941=PLANE('',#27561);
#1942=PLANE('',#27562);
#1943=PLANE('',#27563);
#1944=PLANE('',#27564);
#1945=PLANE('',#27565);
#1946=PLANE('',#27566);
#1947=PLANE('',#27567);
#1948=PLANE('',#27568);
#1949=PLANE('',#27569);
#1950=PLANE('',#27570);
#1951=PLANE('',#27571);
#1952=PLANE('',#27572);
#1953=PLANE('',#27573);
#1954=PLANE('',#27574);
#1955=PLANE('',#27575);
#1956=PLANE('',#27576);
#1957=PLANE('',#27577);
#1958=PLANE('',#27578);
#1959=PLANE('',#27579);
#1960=PLANE('',#27580);
#1961=PLANE('',#27581);
#1962=PLANE('',#27582);
#1963=PLANE('',#27583);
#1964=PLANE('',#27584);
#1965=PLANE('',#27585);
#1966=PLANE('',#27586);
#1967=PLANE('',#27587);
#1968=PLANE('',#27588);
#1969=PLANE('',#27589);
#1970=PLANE('',#27590);
#1971=PLANE('',#27591);
#1972=PLANE('',#27592);
#1973=PLANE('',#27593);
#1974=PLANE('',#27594);
#1975=PLANE('',#27595);
#1976=PLANE('',#27596);
#1977=PLANE('',#27597);
#1978=PLANE('',#27598);
#1979=PLANE('',#27599);
#1980=PLANE('',#27600);
#1981=PLANE('',#27601);
#1982=PLANE('',#27648);
#1983=PLANE('',#27649);
#1984=PLANE('',#27650);
#1985=PLANE('',#27651);
#1986=PLANE('',#27652);
#1987=PLANE('',#27653);
#1988=PLANE('',#27654);
#1989=PLANE('',#27655);
#1990=PLANE('',#27656);
#1991=PLANE('',#27657);
#1992=PLANE('',#27658);
#1993=PLANE('',#27659);
#1994=PLANE('',#27660);
#1995=PLANE('',#27661);
#1996=PLANE('',#27662);
#1997=PLANE('',#27663);
#1998=PLANE('',#27664);
#1999=PLANE('',#27665);
#2000=PLANE('',#27666);
#2001=PLANE('',#27667);
#2002=PLANE('',#27675);
#2003=PLANE('',#27676);
#2004=PLANE('',#27700);
#2005=PLANE('',#27701);
#2006=PLANE('',#27702);
#2007=PLANE('',#27703);
#2008=PLANE('',#27704);
#2009=PLANE('',#27705);
#2010=PLANE('',#27706);
#2011=PLANE('',#27707);
#2012=PLANE('',#27708);
#2013=PLANE('',#27709);
#2014=PLANE('',#27710);
#2015=PLANE('',#27711);
#2016=PLANE('',#27715);
#2017=PLANE('',#27719);
#2018=PLANE('',#27915);
#2019=PLANE('',#27919);
#2020=PLANE('',#27923);
#2021=PLANE('',#27927);
#2022=PLANE('',#27931);
#2023=PLANE('',#27935);
#2024=PLANE('',#27939);
#2025=PLANE('',#27943);
#2026=PLANE('',#27945);
#2027=PLANE('',#27947);
#2028=PLANE('',#27950);
#2029=PLANE('',#27951);
#2030=PLANE('',#27952);
#2031=PLANE('',#27953);
#2032=PLANE('',#27954);
#2033=PLANE('',#27955);
#2034=PLANE('',#27956);
#2035=PLANE('',#27958);
#2036=PLANE('',#27966);
#2037=PLANE('',#27967);
#2038=PLANE('',#27968);
#2039=PLANE('',#27969);
#2040=PLANE('',#27970);
#2041=PLANE('',#27971);
#2042=PLANE('',#27972);
#2043=PLANE('',#27973);
#2044=PLANE('',#27974);
#2045=PLANE('',#27980);
#2046=PLANE('',#27988);
#2047=PLANE('',#27989);
#2048=PLANE('',#27990);
#2049=PLANE('',#27991);
#2050=PLANE('',#27992);
#2051=PLANE('',#27993);
#2052=PLANE('',#27994);
#2053=PLANE('',#27995);
#2054=PLANE('',#27996);
#2055=PLANE('',#28002);
#2056=PLANE('',#28007);
#2057=PLANE('',#28012);
#2058=PLANE('',#28035);
#2059=PLANE('',#28038);
#2060=PLANE('',#28043);
#2061=PLANE('',#28047);
#2062=PLANE('',#28048);
#2063=PLANE('',#28052);
#2064=PLANE('',#28058);
#2065=PLANE('',#28062);
#2066=PLANE('',#28063);
#2067=PLANE('',#28064);
#2068=PLANE('',#28070);
#2069=PLANE('',#28090);
#2070=PLANE('',#28091);
#2071=PLANE('',#28092);
#2072=PLANE('',#28093);
#2073=PLANE('',#28094);
#2074=PLANE('',#28095);
#2075=PLANE('',#28108);
#2076=PLANE('',#28110);
#2077=PLANE('',#28141);
#2078=PLANE('',#28142);
#2079=PLANE('',#28143);
#2080=PLANE('',#28144);
#2081=PLANE('',#28145);
#2082=PLANE('',#28146);
#2083=PLANE('',#28147);
#2084=PLANE('',#28148);
#2085=PLANE('',#28149);
#2086=PLANE('',#28151);
#2087=PLANE('',#28152);
#2088=PLANE('',#28154);
#2089=PLANE('',#28155);
#2090=PLANE('',#28157);
#2091=PLANE('',#28159);
#2092=PLANE('',#28160);
#2093=PLANE('',#28162);
#2094=PLANE('',#28163);
#2095=PLANE('',#28165);
#2096=PLANE('',#28173);
#2097=PLANE('',#28174);
#2098=PLANE('',#28175);
#2099=PLANE('',#28176);
#2100=PLANE('',#28177);
#2101=PLANE('',#28178);
#2102=PLANE('',#28179);
#2103=PLANE('',#28180);
#2104=PLANE('',#28182);
#2105=PLANE('',#28184);
#2106=PLANE('',#28185);
#2107=PLANE('',#28187);
#2108=PLANE('',#28190);
#2109=PLANE('',#28192);
#2110=PLANE('',#28193);
#2111=PLANE('',#28196);
#2112=PLANE('',#28197);
#2113=PLANE('',#28199);
#2114=PLANE('',#28200);
#2115=PLANE('',#28202);
#2116=PLANE('',#28203);
#2117=PLANE('',#28205);
#2118=PLANE('',#28207);
#2119=PLANE('',#28210);
#2120=PLANE('',#28212);
#2121=PLANE('',#28215);
#2122=PLANE('',#28216);
#2123=PLANE('',#28217);
#2124=PLANE('',#28218);
#2125=PLANE('',#28219);
#2126=PLANE('',#28220);
#2127=PLANE('',#28221);
#2128=PLANE('',#28223);
#2129=PLANE('',#28231);
#2130=PLANE('',#28232);
#2131=PLANE('',#28233);
#2132=PLANE('',#28234);
#2133=PLANE('',#28235);
#2134=PLANE('',#28236);
#2135=PLANE('',#28237);
#2136=PLANE('',#28238);
#2137=PLANE('',#28239);
#2138=PLANE('',#28245);
#2139=PLANE('',#28253);
#2140=PLANE('',#28254);
#2141=PLANE('',#28255);
#2142=PLANE('',#28256);
#2143=PLANE('',#28257);
#2144=PLANE('',#28258);
#2145=PLANE('',#28259);
#2146=PLANE('',#28260);
#2147=PLANE('',#28261);
#2148=PLANE('',#28267);
#2149=PLANE('',#28272);
#2150=PLANE('',#28277);
#2151=PLANE('',#28300);
#2152=PLANE('',#28303);
#2153=PLANE('',#28308);
#2154=PLANE('',#28312);
#2155=PLANE('',#28313);
#2156=PLANE('',#28317);
#2157=PLANE('',#28323);
#2158=PLANE('',#28327);
#2159=PLANE('',#28328);
#2160=PLANE('',#28329);
#2161=PLANE('',#28335);
#2162=PLANE('',#28353);
#2163=PLANE('',#28354);
#2164=PLANE('',#28355);
#2165=PLANE('',#28368);
#2166=PLANE('',#28370);
#2167=PLANE('',#28401);
#2168=PLANE('',#28402);
#2169=PLANE('',#28403);
#2170=PLANE('',#28404);
#2171=PLANE('',#28405);
#2172=PLANE('',#28406);
#2173=PLANE('',#28407);
#2174=PLANE('',#28408);
#2175=PLANE('',#28409);
#2176=PLANE('',#28411);
#2177=PLANE('',#28412);
#2178=PLANE('',#28414);
#2179=PLANE('',#28415);
#2180=PLANE('',#28417);
#2181=PLANE('',#28419);
#2182=PLANE('',#28420);
#2183=PLANE('',#28422);
#2184=PLANE('',#28423);
#2185=PLANE('',#28425);
#2186=PLANE('',#28433);
#2187=PLANE('',#28434);
#2188=PLANE('',#28435);
#2189=PLANE('',#28436);
#2190=PLANE('',#28437);
#2191=PLANE('',#28438);
#2192=PLANE('',#28439);
#2193=PLANE('',#28440);
#2194=PLANE('',#28442);
#2195=PLANE('',#28444);
#2196=PLANE('',#28445);
#2197=PLANE('',#28447);
#2198=PLANE('',#28450);
#2199=PLANE('',#28452);
#2200=PLANE('',#28453);
#2201=PLANE('',#28456);
#2202=PLANE('',#28457);
#2203=PLANE('',#28459);
#2204=PLANE('',#28460);
#2205=PLANE('',#28462);
#2206=PLANE('',#28463);
#2207=PLANE('',#28465);
#2208=PLANE('',#28467);
#2209=PLANE('',#28548);
#2210=PLANE('',#28549);
#2211=PLANE('',#28552);
#2212=PLANE('',#28553);
#2213=PLANE('',#28556);
#2214=PLANE('',#28557);
#2215=PLANE('',#28558);
#2216=PLANE('',#28559);
#2217=PLANE('',#28560);
#2218=PLANE('',#28561);
#2219=PLANE('',#28576);
#2220=PLANE('',#28577);
#2221=PLANE('',#28578);
#2222=PLANE('',#28579);
#2223=PLANE('',#28580);
#2224=PLANE('',#28581);
#2225=PLANE('',#28582);
#2226=PLANE('',#28583);
#2227=PLANE('',#28584);
#2228=PLANE('',#28585);
#2229=PLANE('',#28607);
#2230=PLANE('',#28608);
#2231=PLANE('',#28609);
#2232=PLANE('',#28610);
#2233=PLANE('',#28611);
#2234=PLANE('',#28612);
#2235=PLANE('',#28613);
#2236=PLANE('',#28614);
#2237=PLANE('',#28615);
#2238=PLANE('',#28616);
#2239=PLANE('',#28617);
#2240=PLANE('',#28618);
#2241=PLANE('',#28619);
#2242=PLANE('',#28620);
#2243=PLANE('',#28621);
#2244=PLANE('',#28622);
#2245=PLANE('',#28629);
#2246=PLANE('',#28630);
#2247=PLANE('',#28637);
#2248=PLANE('',#28638);
#2249=PLANE('',#28639);
#2250=PLANE('',#28640);
#2251=PLANE('',#28672);
#2252=PLANE('',#28673);
#2253=PLANE('',#28674);
#2254=PLANE('',#28675);
#2255=PLANE('',#28676);
#2256=PLANE('',#28677);
#2257=PLANE('',#28678);
#2258=PLANE('',#28679);
#2259=PLANE('',#28692);
#2260=PLANE('',#28693);
#2261=PLANE('',#28694);
#2262=PLANE('',#28695);
#2263=PLANE('',#28696);
#2264=PLANE('',#28697);
#2265=PLANE('',#28698);
#2266=PLANE('',#28699);
#2267=PLANE('',#28700);
#2268=PLANE('',#28701);
#2269=FACE_OUTER_BOUND('',#3711,.T.);
#2270=FACE_OUTER_BOUND('',#3712,.T.);
#2271=FACE_OUTER_BOUND('',#3713,.T.);
#2272=FACE_OUTER_BOUND('',#3714,.T.);
#2273=FACE_OUTER_BOUND('',#3715,.T.);
#2274=FACE_OUTER_BOUND('',#3716,.T.);
#2275=FACE_OUTER_BOUND('',#3717,.T.);
#2276=FACE_OUTER_BOUND('',#3718,.T.);
#2277=FACE_OUTER_BOUND('',#3719,.T.);
#2278=FACE_OUTER_BOUND('',#3726,.T.);
#2279=FACE_OUTER_BOUND('',#3733,.T.);
#2280=FACE_OUTER_BOUND('',#3734,.T.);
#2281=FACE_OUTER_BOUND('',#3735,.T.);
#2282=FACE_OUTER_BOUND('',#3736,.T.);
#2283=FACE_OUTER_BOUND('',#3737,.T.);
#2284=FACE_OUTER_BOUND('',#3738,.T.);
#2285=FACE_OUTER_BOUND('',#3739,.T.);
#2286=FACE_OUTER_BOUND('',#3740,.T.);
#2287=FACE_OUTER_BOUND('',#3741,.T.);
#2288=FACE_OUTER_BOUND('',#3742,.T.);
#2289=FACE_OUTER_BOUND('',#3743,.T.);
#2290=FACE_OUTER_BOUND('',#3744,.T.);
#2291=FACE_OUTER_BOUND('',#3745,.T.);
#2292=FACE_OUTER_BOUND('',#3746,.T.);
#2293=FACE_OUTER_BOUND('',#3747,.T.);
#2294=FACE_OUTER_BOUND('',#3748,.T.);
#2295=FACE_OUTER_BOUND('',#3749,.T.);
#2296=FACE_OUTER_BOUND('',#3750,.T.);
#2297=FACE_OUTER_BOUND('',#3751,.T.);
#2298=FACE_OUTER_BOUND('',#3756,.T.);
#2299=FACE_OUTER_BOUND('',#3757,.T.);
#2300=FACE_OUTER_BOUND('',#3758,.T.);
#2301=FACE_OUTER_BOUND('',#3759,.T.);
#2302=FACE_OUTER_BOUND('',#3760,.T.);
#2303=FACE_OUTER_BOUND('',#3765,.T.);
#2304=FACE_OUTER_BOUND('',#3766,.T.);
#2305=FACE_OUTER_BOUND('',#3767,.T.);
#2306=FACE_OUTER_BOUND('',#3768,.T.);
#2307=FACE_OUTER_BOUND('',#3769,.T.);
#2308=FACE_OUTER_BOUND('',#3770,.T.);
#2309=FACE_OUTER_BOUND('',#3771,.T.);
#2310=FACE_OUTER_BOUND('',#3772,.T.);
#2311=FACE_OUTER_BOUND('',#3773,.T.);
#2312=FACE_OUTER_BOUND('',#3774,.T.);
#2313=FACE_OUTER_BOUND('',#3775,.T.);
#2314=FACE_OUTER_BOUND('',#3776,.T.);
#2315=FACE_OUTER_BOUND('',#3777,.T.);
#2316=FACE_OUTER_BOUND('',#3787,.T.);
#2317=FACE_OUTER_BOUND('',#3788,.T.);
#2318=FACE_OUTER_BOUND('',#3789,.T.);
#2319=FACE_OUTER_BOUND('',#3790,.T.);
#2320=FACE_OUTER_BOUND('',#3791,.T.);
#2321=FACE_OUTER_BOUND('',#3801,.T.);
#2322=FACE_OUTER_BOUND('',#3803,.T.);
#2323=FACE_OUTER_BOUND('',#3805,.T.);
#2324=FACE_OUTER_BOUND('',#3807,.T.);
#2325=FACE_OUTER_BOUND('',#3808,.T.);
#2326=FACE_OUTER_BOUND('',#3809,.T.);
#2327=FACE_OUTER_BOUND('',#3810,.T.);
#2328=FACE_OUTER_BOUND('',#3811,.T.);
#2329=FACE_OUTER_BOUND('',#3812,.T.);
#2330=FACE_OUTER_BOUND('',#3813,.T.);
#2331=FACE_OUTER_BOUND('',#3814,.T.);
#2332=FACE_OUTER_BOUND('',#3822,.T.);
#2333=FACE_OUTER_BOUND('',#3823,.T.);
#2334=FACE_OUTER_BOUND('',#3831,.T.);
#2335=FACE_OUTER_BOUND('',#3832,.T.);
#2336=FACE_OUTER_BOUND('',#3833,.T.);
#2337=FACE_OUTER_BOUND('',#3834,.T.);
#2338=FACE_OUTER_BOUND('',#3835,.T.);
#2339=FACE_OUTER_BOUND('',#3836,.T.);
#2340=FACE_OUTER_BOUND('',#3837,.T.);
#2341=FACE_OUTER_BOUND('',#3838,.T.);
#2342=FACE_OUTER_BOUND('',#3839,.T.);
#2343=FACE_OUTER_BOUND('',#3840,.T.);
#2344=FACE_OUTER_BOUND('',#3841,.T.);
#2345=FACE_OUTER_BOUND('',#3842,.T.);
#2346=FACE_OUTER_BOUND('',#3843,.T.);
#2347=FACE_OUTER_BOUND('',#3844,.T.);
#2348=FACE_OUTER_BOUND('',#3845,.T.);
#2349=FACE_OUTER_BOUND('',#3846,.T.);
#2350=FACE_OUTER_BOUND('',#3853,.T.);
#2351=FACE_OUTER_BOUND('',#3860,.T.);
#2352=FACE_OUTER_BOUND('',#3861,.T.);
#2353=FACE_OUTER_BOUND('',#3862,.T.);
#2354=FACE_OUTER_BOUND('',#3863,.T.);
#2355=FACE_OUTER_BOUND('',#3864,.T.);
#2356=FACE_OUTER_BOUND('',#3865,.T.);
#2357=FACE_OUTER_BOUND('',#3866,.T.);
#2358=FACE_OUTER_BOUND('',#3867,.T.);
#2359=FACE_OUTER_BOUND('',#3868,.T.);
#2360=FACE_OUTER_BOUND('',#3869,.T.);
#2361=FACE_OUTER_BOUND('',#3870,.T.);
#2362=FACE_OUTER_BOUND('',#3877,.T.);
#2363=FACE_OUTER_BOUND('',#3884,.T.);
#2364=FACE_OUTER_BOUND('',#3885,.T.);
#2365=FACE_OUTER_BOUND('',#3886,.T.);
#2366=FACE_OUTER_BOUND('',#3887,.T.);
#2367=FACE_OUTER_BOUND('',#3888,.T.);
#2368=FACE_OUTER_BOUND('',#3889,.T.);
#2369=FACE_OUTER_BOUND('',#3890,.T.);
#2370=FACE_OUTER_BOUND('',#3891,.T.);
#2371=FACE_OUTER_BOUND('',#3892,.T.);
#2372=FACE_OUTER_BOUND('',#3893,.T.);
#2373=FACE_OUTER_BOUND('',#3894,.T.);
#2374=FACE_OUTER_BOUND('',#3895,.T.);
#2375=FACE_OUTER_BOUND('',#3896,.T.);
#2376=FACE_OUTER_BOUND('',#3897,.T.);
#2377=FACE_OUTER_BOUND('',#3898,.T.);
#2378=FACE_OUTER_BOUND('',#3899,.T.);
#2379=FACE_OUTER_BOUND('',#3900,.T.);
#2380=FACE_OUTER_BOUND('',#3901,.T.);
#2381=FACE_OUTER_BOUND('',#3902,.T.);
#2382=FACE_OUTER_BOUND('',#3903,.T.);
#2383=FACE_OUTER_BOUND('',#3904,.T.);
#2384=FACE_OUTER_BOUND('',#3905,.T.);
#2385=FACE_OUTER_BOUND('',#3906,.T.);
#2386=FACE_OUTER_BOUND('',#3907,.T.);
#2387=FACE_OUTER_BOUND('',#3908,.T.);
#2388=FACE_OUTER_BOUND('',#3909,.T.);
#2389=FACE_OUTER_BOUND('',#3910,.T.);
#2390=FACE_OUTER_BOUND('',#3911,.T.);
#2391=FACE_OUTER_BOUND('',#3912,.T.);
#2392=FACE_OUTER_BOUND('',#3913,.T.);
#2393=FACE_OUTER_BOUND('',#3914,.T.);
#2394=FACE_OUTER_BOUND('',#3915,.T.);
#2395=FACE_OUTER_BOUND('',#3916,.T.);
#2396=FACE_OUTER_BOUND('',#3917,.T.);
#2397=FACE_OUTER_BOUND('',#3918,.T.);
#2398=FACE_OUTER_BOUND('',#3919,.T.);
#2399=FACE_OUTER_BOUND('',#3920,.T.);
#2400=FACE_OUTER_BOUND('',#3921,.T.);
#2401=FACE_OUTER_BOUND('',#3922,.T.);
#2402=FACE_OUTER_BOUND('',#3923,.T.);
#2403=FACE_OUTER_BOUND('',#3924,.T.);
#2404=FACE_OUTER_BOUND('',#3925,.T.);
#2405=FACE_OUTER_BOUND('',#3926,.T.);
#2406=FACE_OUTER_BOUND('',#3927,.T.);
#2407=FACE_OUTER_BOUND('',#3928,.T.);
#2408=FACE_OUTER_BOUND('',#3929,.T.);
#2409=FACE_OUTER_BOUND('',#3930,.T.);
#2410=FACE_OUTER_BOUND('',#3931,.T.);
#2411=FACE_OUTER_BOUND('',#3932,.T.);
#2412=FACE_OUTER_BOUND('',#3933,.T.);
#2413=FACE_OUTER_BOUND('',#3934,.T.);
#2414=FACE_OUTER_BOUND('',#3935,.T.);
#2415=FACE_OUTER_BOUND('',#3936,.T.);
#2416=FACE_OUTER_BOUND('',#3937,.T.);
#2417=FACE_OUTER_BOUND('',#3938,.T.);
#2418=FACE_OUTER_BOUND('',#3939,.T.);
#2419=FACE_OUTER_BOUND('',#3940,.T.);
#2420=FACE_OUTER_BOUND('',#3941,.T.);
#2421=FACE_OUTER_BOUND('',#3942,.T.);
#2422=FACE_OUTER_BOUND('',#3943,.T.);
#2423=FACE_OUTER_BOUND('',#3944,.T.);
#2424=FACE_OUTER_BOUND('',#3945,.T.);
#2425=FACE_OUTER_BOUND('',#3946,.T.);
#2426=FACE_OUTER_BOUND('',#3947,.T.);
#2427=FACE_OUTER_BOUND('',#3948,.T.);
#2428=FACE_OUTER_BOUND('',#3949,.T.);
#2429=FACE_OUTER_BOUND('',#3950,.T.);
#2430=FACE_OUTER_BOUND('',#3951,.T.);
#2431=FACE_OUTER_BOUND('',#3952,.T.);
#2432=FACE_OUTER_BOUND('',#3953,.T.);
#2433=FACE_OUTER_BOUND('',#3954,.T.);
#2434=FACE_OUTER_BOUND('',#3955,.T.);
#2435=FACE_OUTER_BOUND('',#3956,.T.);
#2436=FACE_OUTER_BOUND('',#3957,.T.);
#2437=FACE_OUTER_BOUND('',#3958,.T.);
#2438=FACE_OUTER_BOUND('',#3959,.T.);
#2439=FACE_OUTER_BOUND('',#3960,.T.);
#2440=FACE_OUTER_BOUND('',#3961,.T.);
#2441=FACE_OUTER_BOUND('',#3962,.T.);
#2442=FACE_OUTER_BOUND('',#3963,.T.);
#2443=FACE_OUTER_BOUND('',#3964,.T.);
#2444=FACE_OUTER_BOUND('',#3965,.T.);
#2445=FACE_OUTER_BOUND('',#3966,.T.);
#2446=FACE_OUTER_BOUND('',#3967,.T.);
#2447=FACE_OUTER_BOUND('',#3968,.T.);
#2448=FACE_OUTER_BOUND('',#3969,.T.);
#2449=FACE_OUTER_BOUND('',#3985,.T.);
#2450=FACE_OUTER_BOUND('',#3986,.T.);
#2451=FACE_OUTER_BOUND('',#3987,.T.);
#2452=FACE_OUTER_BOUND('',#3988,.T.);
#2453=FACE_OUTER_BOUND('',#3989,.T.);
#2454=FACE_OUTER_BOUND('',#3990,.T.);
#2455=FACE_OUTER_BOUND('',#3991,.T.);
#2456=FACE_OUTER_BOUND('',#3992,.T.);
#2457=FACE_OUTER_BOUND('',#3993,.T.);
#2458=FACE_OUTER_BOUND('',#3994,.T.);
#2459=FACE_OUTER_BOUND('',#3995,.T.);
#2460=FACE_OUTER_BOUND('',#3996,.T.);
#2461=FACE_OUTER_BOUND('',#3997,.T.);
#2462=FACE_OUTER_BOUND('',#3998,.T.);
#2463=FACE_OUTER_BOUND('',#3999,.T.);
#2464=FACE_OUTER_BOUND('',#4000,.T.);
#2465=FACE_OUTER_BOUND('',#4001,.T.);
#2466=FACE_OUTER_BOUND('',#4002,.T.);
#2467=FACE_OUTER_BOUND('',#4003,.T.);
#2468=FACE_OUTER_BOUND('',#4004,.T.);
#2469=FACE_OUTER_BOUND('',#4005,.T.);
#2470=FACE_OUTER_BOUND('',#4006,.T.);
#2471=FACE_OUTER_BOUND('',#4007,.T.);
#2472=FACE_OUTER_BOUND('',#4008,.T.);
#2473=FACE_OUTER_BOUND('',#4009,.T.);
#2474=FACE_OUTER_BOUND('',#4010,.T.);
#2475=FACE_OUTER_BOUND('',#4011,.T.);
#2476=FACE_OUTER_BOUND('',#4012,.T.);
#2477=FACE_OUTER_BOUND('',#4013,.T.);
#2478=FACE_OUTER_BOUND('',#4014,.T.);
#2479=FACE_OUTER_BOUND('',#4015,.T.);
#2480=FACE_OUTER_BOUND('',#4016,.T.);
#2481=FACE_OUTER_BOUND('',#4017,.T.);
#2482=FACE_OUTER_BOUND('',#4018,.T.);
#2483=FACE_OUTER_BOUND('',#4019,.T.);
#2484=FACE_OUTER_BOUND('',#4020,.T.);
#2485=FACE_OUTER_BOUND('',#4021,.T.);
#2486=FACE_OUTER_BOUND('',#4022,.T.);
#2487=FACE_OUTER_BOUND('',#4024,.T.);
#2488=FACE_OUTER_BOUND('',#4026,.T.);
#2489=FACE_OUTER_BOUND('',#4028,.T.);
#2490=FACE_OUTER_BOUND('',#4030,.T.);
#2491=FACE_OUTER_BOUND('',#4032,.T.);
#2492=FACE_OUTER_BOUND('',#4034,.T.);
#2493=FACE_OUTER_BOUND('',#4036,.T.);
#2494=FACE_OUTER_BOUND('',#4038,.T.);
#2495=FACE_OUTER_BOUND('',#4040,.T.);
#2496=FACE_OUTER_BOUND('',#4042,.T.);
#2497=FACE_OUTER_BOUND('',#4044,.T.);
#2498=FACE_OUTER_BOUND('',#4046,.T.);
#2499=FACE_OUTER_BOUND('',#4048,.T.);
#2500=FACE_OUTER_BOUND('',#4050,.T.);
#2501=FACE_OUTER_BOUND('',#4052,.T.);
#2502=FACE_OUTER_BOUND('',#4053,.T.);
#2503=FACE_OUTER_BOUND('',#4054,.T.);
#2504=FACE_OUTER_BOUND('',#4055,.T.);
#2505=FACE_OUTER_BOUND('',#4056,.T.);
#2506=FACE_OUTER_BOUND('',#4057,.T.);
#2507=FACE_OUTER_BOUND('',#4058,.T.);
#2508=FACE_OUTER_BOUND('',#4059,.T.);
#2509=FACE_OUTER_BOUND('',#4060,.T.);
#2510=FACE_OUTER_BOUND('',#4061,.T.);
#2511=FACE_OUTER_BOUND('',#4062,.T.);
#2512=FACE_OUTER_BOUND('',#4063,.T.);
#2513=FACE_OUTER_BOUND('',#4064,.T.);
#2514=FACE_OUTER_BOUND('',#4065,.T.);
#2515=FACE_OUTER_BOUND('',#4066,.T.);
#2516=FACE_OUTER_BOUND('',#4067,.T.);
#2517=FACE_OUTER_BOUND('',#4068,.T.);
#2518=FACE_OUTER_BOUND('',#4069,.T.);
#2519=FACE_OUTER_BOUND('',#4070,.T.);
#2520=FACE_OUTER_BOUND('',#4071,.T.);
#2521=FACE_OUTER_BOUND('',#4072,.T.);
#2522=FACE_OUTER_BOUND('',#4073,.T.);
#2523=FACE_OUTER_BOUND('',#4074,.T.);
#2524=FACE_OUTER_BOUND('',#4075,.T.);
#2525=FACE_OUTER_BOUND('',#4076,.T.);
#2526=FACE_OUTER_BOUND('',#4077,.T.);
#2527=FACE_OUTER_BOUND('',#4078,.T.);
#2528=FACE_OUTER_BOUND('',#4079,.T.);
#2529=FACE_OUTER_BOUND('',#4080,.T.);
#2530=FACE_OUTER_BOUND('',#4081,.T.);
#2531=FACE_OUTER_BOUND('',#4082,.T.);
#2532=FACE_OUTER_BOUND('',#4083,.T.);
#2533=FACE_OUTER_BOUND('',#4084,.T.);
#2534=FACE_OUTER_BOUND('',#4085,.T.);
#2535=FACE_OUTER_BOUND('',#4086,.T.);
#2536=FACE_OUTER_BOUND('',#4087,.T.);
#2537=FACE_OUTER_BOUND('',#4088,.T.);
#2538=FACE_OUTER_BOUND('',#4089,.T.);
#2539=FACE_OUTER_BOUND('',#4090,.T.);
#2540=FACE_OUTER_BOUND('',#4091,.T.);
#2541=FACE_OUTER_BOUND('',#4092,.T.);
#2542=FACE_OUTER_BOUND('',#4093,.T.);
#2543=FACE_OUTER_BOUND('',#4094,.T.);
#2544=FACE_OUTER_BOUND('',#4095,.T.);
#2545=FACE_OUTER_BOUND('',#4096,.T.);
#2546=FACE_OUTER_BOUND('',#4097,.T.);
#2547=FACE_OUTER_BOUND('',#4098,.T.);
#2548=FACE_OUTER_BOUND('',#4099,.T.);
#2549=FACE_OUTER_BOUND('',#4100,.T.);
#2550=FACE_OUTER_BOUND('',#4101,.T.);
#2551=FACE_OUTER_BOUND('',#4102,.T.);
#2552=FACE_OUTER_BOUND('',#4103,.T.);
#2553=FACE_OUTER_BOUND('',#4104,.T.);
#2554=FACE_OUTER_BOUND('',#4105,.T.);
#2555=FACE_OUTER_BOUND('',#4106,.T.);
#2556=FACE_OUTER_BOUND('',#4107,.T.);
#2557=FACE_OUTER_BOUND('',#4108,.T.);
#2558=FACE_OUTER_BOUND('',#4109,.T.);
#2559=FACE_OUTER_BOUND('',#4110,.T.);
#2560=FACE_OUTER_BOUND('',#4111,.T.);
#2561=FACE_OUTER_BOUND('',#4112,.T.);
#2562=FACE_OUTER_BOUND('',#4114,.T.);
#2563=FACE_OUTER_BOUND('',#4115,.T.);
#2564=FACE_OUTER_BOUND('',#4117,.T.);
#2565=FACE_OUTER_BOUND('',#4118,.T.);
#2566=FACE_OUTER_BOUND('',#4119,.T.);
#2567=FACE_OUTER_BOUND('',#4120,.T.);
#2568=FACE_OUTER_BOUND('',#4121,.T.);
#2569=FACE_OUTER_BOUND('',#4122,.T.);
#2570=FACE_OUTER_BOUND('',#4123,.T.);
#2571=FACE_OUTER_BOUND('',#4124,.T.);
#2572=FACE_OUTER_BOUND('',#4125,.T.);
#2573=FACE_OUTER_BOUND('',#4126,.T.);
#2574=FACE_OUTER_BOUND('',#4127,.T.);
#2575=FACE_OUTER_BOUND('',#4128,.T.);
#2576=FACE_OUTER_BOUND('',#4129,.T.);
#2577=FACE_OUTER_BOUND('',#4130,.T.);
#2578=FACE_OUTER_BOUND('',#4132,.T.);
#2579=FACE_OUTER_BOUND('',#4133,.T.);
#2580=FACE_OUTER_BOUND('',#4134,.T.);
#2581=FACE_OUTER_BOUND('',#4135,.T.);
#2582=FACE_OUTER_BOUND('',#4136,.T.);
#2583=FACE_OUTER_BOUND('',#4137,.T.);
#2584=FACE_OUTER_BOUND('',#4138,.T.);
#2585=FACE_OUTER_BOUND('',#4139,.T.);
#2586=FACE_OUTER_BOUND('',#4140,.T.);
#2587=FACE_OUTER_BOUND('',#4141,.T.);
#2588=FACE_OUTER_BOUND('',#4142,.T.);
#2589=FACE_OUTER_BOUND('',#4143,.T.);
#2590=FACE_OUTER_BOUND('',#4144,.T.);
#2591=FACE_OUTER_BOUND('',#4145,.T.);
#2592=FACE_OUTER_BOUND('',#4146,.T.);
#2593=FACE_OUTER_BOUND('',#4147,.T.);
#2594=FACE_OUTER_BOUND('',#4148,.T.);
#2595=FACE_OUTER_BOUND('',#4149,.T.);
#2596=FACE_OUTER_BOUND('',#4150,.T.);
#2597=FACE_OUTER_BOUND('',#4151,.T.);
#2598=FACE_OUTER_BOUND('',#4152,.T.);
#2599=FACE_OUTER_BOUND('',#4153,.T.);
#2600=FACE_OUTER_BOUND('',#4154,.T.);
#2601=FACE_OUTER_BOUND('',#4155,.T.);
#2602=FACE_OUTER_BOUND('',#4156,.T.);
#2603=FACE_OUTER_BOUND('',#4157,.T.);
#2604=FACE_OUTER_BOUND('',#4158,.T.);
#2605=FACE_OUTER_BOUND('',#4159,.T.);
#2606=FACE_OUTER_BOUND('',#4160,.T.);
#2607=FACE_OUTER_BOUND('',#4161,.T.);
#2608=FACE_OUTER_BOUND('',#4162,.T.);
#2609=FACE_OUTER_BOUND('',#4163,.T.);
#2610=FACE_OUTER_BOUND('',#4164,.T.);
#2611=FACE_OUTER_BOUND('',#4165,.T.);
#2612=FACE_OUTER_BOUND('',#4166,.T.);
#2613=FACE_OUTER_BOUND('',#4167,.T.);
#2614=FACE_OUTER_BOUND('',#4168,.T.);
#2615=FACE_OUTER_BOUND('',#4169,.T.);
#2616=FACE_OUTER_BOUND('',#4170,.T.);
#2617=FACE_OUTER_BOUND('',#4171,.T.);
#2618=FACE_OUTER_BOUND('',#4172,.T.);
#2619=FACE_OUTER_BOUND('',#4173,.T.);
#2620=FACE_OUTER_BOUND('',#4174,.T.);
#2621=FACE_OUTER_BOUND('',#4175,.T.);
#2622=FACE_OUTER_BOUND('',#4176,.T.);
#2623=FACE_OUTER_BOUND('',#4177,.T.);
#2624=FACE_OUTER_BOUND('',#4178,.T.);
#2625=FACE_OUTER_BOUND('',#4179,.T.);
#2626=FACE_OUTER_BOUND('',#4180,.T.);
#2627=FACE_OUTER_BOUND('',#4181,.T.);
#2628=FACE_OUTER_BOUND('',#4182,.T.);
#2629=FACE_OUTER_BOUND('',#4183,.T.);
#2630=FACE_OUTER_BOUND('',#4184,.T.);
#2631=FACE_OUTER_BOUND('',#4185,.T.);
#2632=FACE_OUTER_BOUND('',#4186,.T.);
#2633=FACE_OUTER_BOUND('',#4187,.T.);
#2634=FACE_OUTER_BOUND('',#4188,.T.);
#2635=FACE_OUTER_BOUND('',#4189,.T.);
#2636=FACE_OUTER_BOUND('',#4190,.T.);
#2637=FACE_OUTER_BOUND('',#4191,.T.);
#2638=FACE_OUTER_BOUND('',#4192,.T.);
#2639=FACE_OUTER_BOUND('',#4193,.T.);
#2640=FACE_OUTER_BOUND('',#4194,.T.);
#2641=FACE_OUTER_BOUND('',#4195,.T.);
#2642=FACE_OUTER_BOUND('',#4196,.T.);
#2643=FACE_OUTER_BOUND('',#4197,.T.);
#2644=FACE_OUTER_BOUND('',#4198,.T.);
#2645=FACE_OUTER_BOUND('',#4199,.T.);
#2646=FACE_OUTER_BOUND('',#4200,.T.);
#2647=FACE_OUTER_BOUND('',#4201,.T.);
#2648=FACE_OUTER_BOUND('',#4202,.T.);
#2649=FACE_OUTER_BOUND('',#4203,.T.);
#2650=FACE_OUTER_BOUND('',#4204,.T.);
#2651=FACE_OUTER_BOUND('',#4205,.T.);
#2652=FACE_OUTER_BOUND('',#4206,.T.);
#2653=FACE_OUTER_BOUND('',#4207,.T.);
#2654=FACE_OUTER_BOUND('',#4208,.T.);
#2655=FACE_OUTER_BOUND('',#4209,.T.);
#2656=FACE_OUTER_BOUND('',#4210,.T.);
#2657=FACE_OUTER_BOUND('',#4211,.T.);
#2658=FACE_OUTER_BOUND('',#4212,.T.);
#2659=FACE_OUTER_BOUND('',#4213,.T.);
#2660=FACE_OUTER_BOUND('',#4214,.T.);
#2661=FACE_OUTER_BOUND('',#4215,.T.);
#2662=FACE_OUTER_BOUND('',#4216,.T.);
#2663=FACE_OUTER_BOUND('',#4217,.T.);
#2664=FACE_OUTER_BOUND('',#4218,.T.);
#2665=FACE_OUTER_BOUND('',#4219,.T.);
#2666=FACE_OUTER_BOUND('',#4220,.T.);
#2667=FACE_OUTER_BOUND('',#4221,.T.);
#2668=FACE_OUTER_BOUND('',#4222,.T.);
#2669=FACE_OUTER_BOUND('',#4223,.T.);
#2670=FACE_OUTER_BOUND('',#4224,.T.);
#2671=FACE_OUTER_BOUND('',#4225,.T.);
#2672=FACE_OUTER_BOUND('',#4226,.T.);
#2673=FACE_OUTER_BOUND('',#4227,.T.);
#2674=FACE_OUTER_BOUND('',#4228,.T.);
#2675=FACE_OUTER_BOUND('',#4230,.T.);
#2676=FACE_OUTER_BOUND('',#4231,.T.);
#2677=FACE_OUTER_BOUND('',#4232,.T.);
#2678=FACE_OUTER_BOUND('',#4233,.T.);
#2679=FACE_OUTER_BOUND('',#4234,.T.);
#2680=FACE_OUTER_BOUND('',#4235,.T.);
#2681=FACE_OUTER_BOUND('',#4236,.T.);
#2682=FACE_OUTER_BOUND('',#4237,.T.);
#2683=FACE_OUTER_BOUND('',#4238,.T.);
#2684=FACE_OUTER_BOUND('',#4239,.T.);
#2685=FACE_OUTER_BOUND('',#4240,.T.);
#2686=FACE_OUTER_BOUND('',#4241,.T.);
#2687=FACE_OUTER_BOUND('',#4243,.T.);
#2688=FACE_OUTER_BOUND('',#4244,.T.);
#2689=FACE_OUTER_BOUND('',#4245,.T.);
#2690=FACE_OUTER_BOUND('',#4246,.T.);
#2691=FACE_OUTER_BOUND('',#4247,.T.);
#2692=FACE_OUTER_BOUND('',#4248,.T.);
#2693=FACE_OUTER_BOUND('',#4249,.T.);
#2694=FACE_OUTER_BOUND('',#4251,.T.);
#2695=FACE_OUTER_BOUND('',#4252,.T.);
#2696=FACE_OUTER_BOUND('',#4254,.T.);
#2697=FACE_OUTER_BOUND('',#4255,.T.);
#2698=FACE_OUTER_BOUND('',#4256,.T.);
#2699=FACE_OUTER_BOUND('',#4257,.T.);
#2700=FACE_OUTER_BOUND('',#4259,.T.);
#2701=FACE_OUTER_BOUND('',#4260,.T.);
#2702=FACE_OUTER_BOUND('',#4261,.T.);
#2703=FACE_OUTER_BOUND('',#4262,.T.);
#2704=FACE_OUTER_BOUND('',#4263,.T.);
#2705=FACE_OUTER_BOUND('',#4264,.T.);
#2706=FACE_OUTER_BOUND('',#4265,.T.);
#2707=FACE_OUTER_BOUND('',#4266,.T.);
#2708=FACE_OUTER_BOUND('',#4267,.T.);
#2709=FACE_OUTER_BOUND('',#4268,.T.);
#2710=FACE_OUTER_BOUND('',#4269,.T.);
#2711=FACE_OUTER_BOUND('',#4270,.T.);
#2712=FACE_OUTER_BOUND('',#4271,.T.);
#2713=FACE_OUTER_BOUND('',#4272,.T.);
#2714=FACE_OUTER_BOUND('',#4273,.T.);
#2715=FACE_OUTER_BOUND('',#4274,.T.);
#2716=FACE_OUTER_BOUND('',#4275,.T.);
#2717=FACE_OUTER_BOUND('',#4276,.T.);
#2718=FACE_OUTER_BOUND('',#4277,.T.);
#2719=FACE_OUTER_BOUND('',#4278,.T.);
#2720=FACE_OUTER_BOUND('',#4279,.T.);
#2721=FACE_OUTER_BOUND('',#4280,.T.);
#2722=FACE_OUTER_BOUND('',#4281,.T.);
#2723=FACE_OUTER_BOUND('',#4282,.T.);
#2724=FACE_OUTER_BOUND('',#4283,.T.);
#2725=FACE_OUTER_BOUND('',#4284,.T.);
#2726=FACE_OUTER_BOUND('',#4285,.T.);
#2727=FACE_OUTER_BOUND('',#4286,.T.);
#2728=FACE_OUTER_BOUND('',#4287,.T.);
#2729=FACE_OUTER_BOUND('',#4288,.T.);
#2730=FACE_OUTER_BOUND('',#4289,.T.);
#2731=FACE_OUTER_BOUND('',#4290,.T.);
#2732=FACE_OUTER_BOUND('',#4291,.T.);
#2733=FACE_OUTER_BOUND('',#4292,.T.);
#2734=FACE_OUTER_BOUND('',#4293,.T.);
#2735=FACE_OUTER_BOUND('',#4294,.T.);
#2736=FACE_OUTER_BOUND('',#4295,.T.);
#2737=FACE_OUTER_BOUND('',#4296,.T.);
#2738=FACE_OUTER_BOUND('',#4297,.T.);
#2739=FACE_OUTER_BOUND('',#4298,.T.);
#2740=FACE_OUTER_BOUND('',#4299,.T.);
#2741=FACE_OUTER_BOUND('',#4300,.T.);
#2742=FACE_OUTER_BOUND('',#4301,.T.);
#2743=FACE_OUTER_BOUND('',#4302,.T.);
#2744=FACE_OUTER_BOUND('',#4303,.T.);
#2745=FACE_OUTER_BOUND('',#4304,.T.);
#2746=FACE_OUTER_BOUND('',#4305,.T.);
#2747=FACE_OUTER_BOUND('',#4307,.T.);
#2748=FACE_OUTER_BOUND('',#4308,.T.);
#2749=FACE_OUTER_BOUND('',#4309,.T.);
#2750=FACE_OUTER_BOUND('',#4310,.T.);
#2751=FACE_OUTER_BOUND('',#4312,.T.);
#2752=FACE_OUTER_BOUND('',#4314,.T.);
#2753=FACE_OUTER_BOUND('',#4315,.T.);
#2754=FACE_OUTER_BOUND('',#4316,.T.);
#2755=FACE_OUTER_BOUND('',#4317,.T.);
#2756=FACE_OUTER_BOUND('',#4318,.T.);
#2757=FACE_OUTER_BOUND('',#4319,.T.);
#2758=FACE_OUTER_BOUND('',#4322,.T.);
#2759=FACE_OUTER_BOUND('',#4323,.T.);
#2760=FACE_OUTER_BOUND('',#4324,.T.);
#2761=FACE_OUTER_BOUND('',#4325,.T.);
#2762=FACE_OUTER_BOUND('',#4326,.T.);
#2763=FACE_OUTER_BOUND('',#4327,.T.);
#2764=FACE_OUTER_BOUND('',#4328,.T.);
#2765=FACE_OUTER_BOUND('',#4329,.T.);
#2766=FACE_OUTER_BOUND('',#4332,.T.);
#2767=FACE_OUTER_BOUND('',#4333,.T.);
#2768=FACE_OUTER_BOUND('',#4334,.T.);
#2769=FACE_OUTER_BOUND('',#4335,.T.);
#2770=FACE_OUTER_BOUND('',#4336,.T.);
#2771=FACE_OUTER_BOUND('',#4338,.T.);
#2772=FACE_OUTER_BOUND('',#4339,.T.);
#2773=FACE_OUTER_BOUND('',#4340,.T.);
#2774=FACE_OUTER_BOUND('',#4341,.T.);
#2775=FACE_OUTER_BOUND('',#4342,.T.);
#2776=FACE_OUTER_BOUND('',#4344,.T.);
#2777=FACE_OUTER_BOUND('',#4345,.T.);
#2778=FACE_OUTER_BOUND('',#4346,.T.);
#2779=FACE_OUTER_BOUND('',#4347,.T.);
#2780=FACE_OUTER_BOUND('',#4348,.T.);
#2781=FACE_OUTER_BOUND('',#4349,.T.);
#2782=FACE_OUTER_BOUND('',#4351,.T.);
#2783=FACE_OUTER_BOUND('',#4352,.T.);
#2784=FACE_OUTER_BOUND('',#4353,.T.);
#2785=FACE_OUTER_BOUND('',#4354,.T.);
#2786=FACE_OUTER_BOUND('',#4356,.T.);
#2787=FACE_OUTER_BOUND('',#4357,.T.);
#2788=FACE_OUTER_BOUND('',#4358,.T.);
#2789=FACE_OUTER_BOUND('',#4359,.T.);
#2790=FACE_OUTER_BOUND('',#4360,.T.);
#2791=FACE_OUTER_BOUND('',#4361,.T.);
#2792=FACE_OUTER_BOUND('',#4362,.T.);
#2793=FACE_OUTER_BOUND('',#4363,.T.);
#2794=FACE_OUTER_BOUND('',#4364,.T.);
#2795=FACE_OUTER_BOUND('',#4365,.T.);
#2796=FACE_OUTER_BOUND('',#4366,.T.);
#2797=FACE_OUTER_BOUND('',#4367,.T.);
#2798=FACE_OUTER_BOUND('',#4368,.T.);
#2799=FACE_OUTER_BOUND('',#4369,.T.);
#2800=FACE_OUTER_BOUND('',#4370,.T.);
#2801=FACE_OUTER_BOUND('',#4371,.T.);
#2802=FACE_OUTER_BOUND('',#4372,.T.);
#2803=FACE_OUTER_BOUND('',#4373,.T.);
#2804=FACE_OUTER_BOUND('',#4374,.T.);
#2805=FACE_OUTER_BOUND('',#4375,.T.);
#2806=FACE_OUTER_BOUND('',#4376,.T.);
#2807=FACE_OUTER_BOUND('',#4377,.T.);
#2808=FACE_OUTER_BOUND('',#4378,.T.);
#2809=FACE_OUTER_BOUND('',#4379,.T.);
#2810=FACE_OUTER_BOUND('',#4380,.T.);
#2811=FACE_OUTER_BOUND('',#4381,.T.);
#2812=FACE_OUTER_BOUND('',#4382,.T.);
#2813=FACE_OUTER_BOUND('',#4383,.T.);
#2814=FACE_OUTER_BOUND('',#4384,.T.);
#2815=FACE_OUTER_BOUND('',#4385,.T.);
#2816=FACE_OUTER_BOUND('',#4386,.T.);
#2817=FACE_OUTER_BOUND('',#4387,.T.);
#2818=FACE_OUTER_BOUND('',#4388,.T.);
#2819=FACE_OUTER_BOUND('',#4389,.T.);
#2820=FACE_OUTER_BOUND('',#4391,.T.);
#2821=FACE_OUTER_BOUND('',#4392,.T.);
#2822=FACE_OUTER_BOUND('',#4393,.T.);
#2823=FACE_OUTER_BOUND('',#4394,.T.);
#2824=FACE_OUTER_BOUND('',#4395,.T.);
#2825=FACE_OUTER_BOUND('',#4396,.T.);
#2826=FACE_OUTER_BOUND('',#4397,.T.);
#2827=FACE_OUTER_BOUND('',#4398,.T.);
#2828=FACE_OUTER_BOUND('',#4399,.T.);
#2829=FACE_OUTER_BOUND('',#4400,.T.);
#2830=FACE_OUTER_BOUND('',#4401,.T.);
#2831=FACE_OUTER_BOUND('',#4403,.T.);
#2832=FACE_OUTER_BOUND('',#4405,.T.);
#2833=FACE_OUTER_BOUND('',#4406,.T.);
#2834=FACE_OUTER_BOUND('',#4407,.T.);
#2835=FACE_OUTER_BOUND('',#4408,.T.);
#2836=FACE_OUTER_BOUND('',#4409,.T.);
#2837=FACE_OUTER_BOUND('',#4410,.T.);
#2838=FACE_OUTER_BOUND('',#4411,.T.);
#2839=FACE_OUTER_BOUND('',#4412,.T.);
#2840=FACE_OUTER_BOUND('',#4413,.T.);
#2841=FACE_OUTER_BOUND('',#4414,.T.);
#2842=FACE_OUTER_BOUND('',#4415,.T.);
#2843=FACE_OUTER_BOUND('',#4416,.T.);
#2844=FACE_OUTER_BOUND('',#4417,.T.);
#2845=FACE_OUTER_BOUND('',#4418,.T.);
#2846=FACE_OUTER_BOUND('',#4419,.T.);
#2847=FACE_OUTER_BOUND('',#4420,.T.);
#2848=FACE_OUTER_BOUND('',#4421,.T.);
#2849=FACE_OUTER_BOUND('',#4422,.T.);
#2850=FACE_OUTER_BOUND('',#4424,.T.);
#2851=FACE_OUTER_BOUND('',#4426,.T.);
#2852=FACE_OUTER_BOUND('',#4427,.T.);
#2853=FACE_OUTER_BOUND('',#4428,.T.);
#2854=FACE_OUTER_BOUND('',#4429,.T.);
#2855=FACE_OUTER_BOUND('',#4430,.T.);
#2856=FACE_OUTER_BOUND('',#4431,.T.);
#2857=FACE_OUTER_BOUND('',#4432,.T.);
#2858=FACE_OUTER_BOUND('',#4433,.T.);
#2859=FACE_OUTER_BOUND('',#4434,.T.);
#2860=FACE_OUTER_BOUND('',#4435,.T.);
#2861=FACE_OUTER_BOUND('',#4436,.T.);
#2862=FACE_OUTER_BOUND('',#4437,.T.);
#2863=FACE_OUTER_BOUND('',#4438,.T.);
#2864=FACE_OUTER_BOUND('',#4439,.T.);
#2865=FACE_OUTER_BOUND('',#4440,.T.);
#2866=FACE_OUTER_BOUND('',#4441,.T.);
#2867=FACE_OUTER_BOUND('',#4442,.T.);
#2868=FACE_OUTER_BOUND('',#4443,.T.);
#2869=FACE_OUTER_BOUND('',#4444,.T.);
#2870=FACE_OUTER_BOUND('',#4445,.T.);
#2871=FACE_OUTER_BOUND('',#4446,.T.);
#2872=FACE_OUTER_BOUND('',#4447,.T.);
#2873=FACE_OUTER_BOUND('',#4448,.T.);
#2874=FACE_OUTER_BOUND('',#4449,.T.);
#2875=FACE_OUTER_BOUND('',#4450,.T.);
#2876=FACE_OUTER_BOUND('',#4451,.T.);
#2877=FACE_OUTER_BOUND('',#4452,.T.);
#2878=FACE_OUTER_BOUND('',#4453,.T.);
#2879=FACE_OUTER_BOUND('',#4454,.T.);
#2880=FACE_OUTER_BOUND('',#4455,.T.);
#2881=FACE_OUTER_BOUND('',#4457,.T.);
#2882=FACE_OUTER_BOUND('',#4458,.T.);
#2883=FACE_OUTER_BOUND('',#4459,.T.);
#2884=FACE_OUTER_BOUND('',#4460,.T.);
#2885=FACE_OUTER_BOUND('',#4461,.T.);
#2886=FACE_OUTER_BOUND('',#4462,.T.);
#2887=FACE_OUTER_BOUND('',#4463,.T.);
#2888=FACE_OUTER_BOUND('',#4464,.T.);
#2889=FACE_OUTER_BOUND('',#4465,.T.);
#2890=FACE_OUTER_BOUND('',#4466,.T.);
#2891=FACE_OUTER_BOUND('',#4467,.T.);
#2892=FACE_OUTER_BOUND('',#4468,.T.);
#2893=FACE_OUTER_BOUND('',#4469,.T.);
#2894=FACE_OUTER_BOUND('',#4470,.T.);
#2895=FACE_OUTER_BOUND('',#4472,.T.);
#2896=FACE_OUTER_BOUND('',#4474,.T.);
#2897=FACE_OUTER_BOUND('',#4476,.T.);
#2898=FACE_OUTER_BOUND('',#4478,.T.);
#2899=FACE_OUTER_BOUND('',#4480,.T.);
#2900=FACE_OUTER_BOUND('',#4481,.T.);
#2901=FACE_OUTER_BOUND('',#4482,.T.);
#2902=FACE_OUTER_BOUND('',#4483,.T.);
#2903=FACE_OUTER_BOUND('',#4484,.T.);
#2904=FACE_OUTER_BOUND('',#4485,.T.);
#2905=FACE_OUTER_BOUND('',#4486,.T.);
#2906=FACE_OUTER_BOUND('',#4487,.T.);
#2907=FACE_OUTER_BOUND('',#4488,.T.);
#2908=FACE_OUTER_BOUND('',#4489,.T.);
#2909=FACE_OUTER_BOUND('',#4490,.T.);
#2910=FACE_OUTER_BOUND('',#4491,.T.);
#2911=FACE_OUTER_BOUND('',#4492,.T.);
#2912=FACE_OUTER_BOUND('',#4493,.T.);
#2913=FACE_OUTER_BOUND('',#4494,.T.);
#2914=FACE_OUTER_BOUND('',#4495,.T.);
#2915=FACE_OUTER_BOUND('',#4496,.T.);
#2916=FACE_OUTER_BOUND('',#4497,.T.);
#2917=FACE_OUTER_BOUND('',#4499,.T.);
#2918=FACE_OUTER_BOUND('',#4500,.T.);
#2919=FACE_OUTER_BOUND('',#4501,.T.);
#2920=FACE_OUTER_BOUND('',#4502,.T.);
#2921=FACE_OUTER_BOUND('',#4510,.T.);
#2922=FACE_OUTER_BOUND('',#4511,.T.);
#2923=FACE_OUTER_BOUND('',#4512,.T.);
#2924=FACE_OUTER_BOUND('',#4514,.T.);
#2925=FACE_OUTER_BOUND('',#4515,.T.);
#2926=FACE_OUTER_BOUND('',#4516,.T.);
#2927=FACE_OUTER_BOUND('',#4517,.T.);
#2928=FACE_OUTER_BOUND('',#4525,.T.);
#2929=FACE_OUTER_BOUND('',#4527,.T.);
#2930=FACE_OUTER_BOUND('',#4529,.T.);
#2931=FACE_OUTER_BOUND('',#4531,.T.);
#2932=FACE_OUTER_BOUND('',#4533,.T.);
#2933=FACE_OUTER_BOUND('',#4535,.T.);
#2934=FACE_OUTER_BOUND('',#4536,.T.);
#2935=FACE_OUTER_BOUND('',#4537,.T.);
#2936=FACE_OUTER_BOUND('',#4538,.T.);
#2937=FACE_OUTER_BOUND('',#4539,.T.);
#2938=FACE_OUTER_BOUND('',#4540,.T.);
#2939=FACE_OUTER_BOUND('',#4541,.T.);
#2940=FACE_OUTER_BOUND('',#4542,.T.);
#2941=FACE_OUTER_BOUND('',#4543,.T.);
#2942=FACE_OUTER_BOUND('',#4544,.T.);
#2943=FACE_OUTER_BOUND('',#4546,.T.);
#2944=FACE_OUTER_BOUND('',#4547,.T.);
#2945=FACE_OUTER_BOUND('',#4548,.T.);
#2946=FACE_OUTER_BOUND('',#4551,.T.);
#2947=FACE_OUTER_BOUND('',#4552,.T.);
#2948=FACE_OUTER_BOUND('',#4553,.T.);
#2949=FACE_OUTER_BOUND('',#4555,.T.);
#2950=FACE_OUTER_BOUND('',#4556,.T.);
#2951=FACE_OUTER_BOUND('',#4557,.T.);
#2952=FACE_OUTER_BOUND('',#4558,.T.);
#2953=FACE_OUTER_BOUND('',#4559,.T.);
#2954=FACE_OUTER_BOUND('',#4560,.T.);
#2955=FACE_OUTER_BOUND('',#4562,.T.);
#2956=FACE_OUTER_BOUND('',#4564,.T.);
#2957=FACE_OUTER_BOUND('',#4566,.T.);
#2958=FACE_OUTER_BOUND('',#4568,.T.);
#2959=FACE_OUTER_BOUND('',#4570,.T.);
#2960=FACE_OUTER_BOUND('',#4572,.T.);
#2961=FACE_OUTER_BOUND('',#4573,.T.);
#2962=FACE_OUTER_BOUND('',#4574,.T.);
#2963=FACE_OUTER_BOUND('',#4575,.T.);
#2964=FACE_OUTER_BOUND('',#4576,.T.);
#2965=FACE_OUTER_BOUND('',#4579,.T.);
#2966=FACE_OUTER_BOUND('',#4582,.T.);
#2967=FACE_OUTER_BOUND('',#4583,.T.);
#2968=FACE_OUTER_BOUND('',#4584,.T.);
#2969=FACE_OUTER_BOUND('',#4585,.T.);
#2970=FACE_OUTER_BOUND('',#4586,.T.);
#2971=FACE_OUTER_BOUND('',#4587,.T.);
#2972=FACE_OUTER_BOUND('',#4588,.T.);
#2973=FACE_OUTER_BOUND('',#4589,.T.);
#2974=FACE_OUTER_BOUND('',#4590,.T.);
#2975=FACE_OUTER_BOUND('',#4591,.T.);
#2976=FACE_OUTER_BOUND('',#4592,.T.);
#2977=FACE_OUTER_BOUND('',#4593,.T.);
#2978=FACE_OUTER_BOUND('',#4594,.T.);
#2979=FACE_OUTER_BOUND('',#4595,.T.);
#2980=FACE_OUTER_BOUND('',#4596,.T.);
#2981=FACE_OUTER_BOUND('',#4597,.T.);
#2982=FACE_OUTER_BOUND('',#4598,.T.);
#2983=FACE_OUTER_BOUND('',#4599,.T.);
#2984=FACE_OUTER_BOUND('',#4600,.T.);
#2985=FACE_OUTER_BOUND('',#4601,.T.);
#2986=FACE_OUTER_BOUND('',#4602,.T.);
#2987=FACE_OUTER_BOUND('',#4603,.T.);
#2988=FACE_OUTER_BOUND('',#4604,.T.);
#2989=FACE_OUTER_BOUND('',#4605,.T.);
#2990=FACE_OUTER_BOUND('',#4606,.T.);
#2991=FACE_OUTER_BOUND('',#4607,.T.);
#2992=FACE_OUTER_BOUND('',#4608,.T.);
#2993=FACE_OUTER_BOUND('',#4609,.T.);
#2994=FACE_OUTER_BOUND('',#4610,.T.);
#2995=FACE_OUTER_BOUND('',#4611,.T.);
#2996=FACE_OUTER_BOUND('',#4612,.T.);
#2997=FACE_OUTER_BOUND('',#4613,.T.);
#2998=FACE_OUTER_BOUND('',#4615,.T.);
#2999=FACE_OUTER_BOUND('',#4617,.T.);
#3000=FACE_OUTER_BOUND('',#4619,.T.);
#3001=FACE_OUTER_BOUND('',#4621,.T.);
#3002=FACE_OUTER_BOUND('',#4623,.T.);
#3003=FACE_OUTER_BOUND('',#4626,.T.);
#3004=FACE_OUTER_BOUND('',#4627,.T.);
#3005=FACE_OUTER_BOUND('',#4628,.T.);
#3006=FACE_OUTER_BOUND('',#4633,.T.);
#3007=FACE_OUTER_BOUND('',#4634,.T.);
#3008=FACE_OUTER_BOUND('',#4635,.T.);
#3009=FACE_OUTER_BOUND('',#4638,.T.);
#3010=FACE_OUTER_BOUND('',#4639,.T.);
#3011=FACE_OUTER_BOUND('',#4640,.T.);
#3012=FACE_OUTER_BOUND('',#4641,.T.);
#3013=FACE_OUTER_BOUND('',#4642,.T.);
#3014=FACE_OUTER_BOUND('',#4643,.T.);
#3015=FACE_OUTER_BOUND('',#4645,.T.);
#3016=FACE_OUTER_BOUND('',#4647,.T.);
#3017=FACE_OUTER_BOUND('',#4649,.T.);
#3018=FACE_OUTER_BOUND('',#4651,.T.);
#3019=FACE_OUTER_BOUND('',#4653,.T.);
#3020=FACE_OUTER_BOUND('',#4659,.T.);
#3021=FACE_OUTER_BOUND('',#4660,.T.);
#3022=FACE_OUTER_BOUND('',#4661,.T.);
#3023=FACE_OUTER_BOUND('',#4662,.T.);
#3024=FACE_OUTER_BOUND('',#4663,.T.);
#3025=FACE_OUTER_BOUND('',#4664,.T.);
#3026=FACE_OUTER_BOUND('',#4665,.T.);
#3027=FACE_OUTER_BOUND('',#4666,.T.);
#3028=FACE_OUTER_BOUND('',#4667,.T.);
#3029=FACE_OUTER_BOUND('',#4669,.T.);
#3030=FACE_OUTER_BOUND('',#4671,.T.);
#3031=FACE_OUTER_BOUND('',#4673,.T.);
#3032=FACE_OUTER_BOUND('',#4675,.T.);
#3033=FACE_OUTER_BOUND('',#4676,.T.);
#3034=FACE_OUTER_BOUND('',#4677,.T.);
#3035=FACE_OUTER_BOUND('',#4678,.T.);
#3036=FACE_OUTER_BOUND('',#4679,.T.);
#3037=FACE_OUTER_BOUND('',#4680,.T.);
#3038=FACE_OUTER_BOUND('',#4681,.T.);
#3039=FACE_OUTER_BOUND('',#4682,.T.);
#3040=FACE_OUTER_BOUND('',#4683,.T.);
#3041=FACE_OUTER_BOUND('',#4684,.T.);
#3042=FACE_OUTER_BOUND('',#4685,.T.);
#3043=FACE_OUTER_BOUND('',#4686,.T.);
#3044=FACE_OUTER_BOUND('',#4687,.T.);
#3045=FACE_OUTER_BOUND('',#4688,.T.);
#3046=FACE_OUTER_BOUND('',#4689,.T.);
#3047=FACE_OUTER_BOUND('',#4690,.T.);
#3048=FACE_OUTER_BOUND('',#4691,.T.);
#3049=FACE_OUTER_BOUND('',#4692,.T.);
#3050=FACE_OUTER_BOUND('',#4693,.T.);
#3051=FACE_OUTER_BOUND('',#4694,.T.);
#3052=FACE_OUTER_BOUND('',#4695,.T.);
#3053=FACE_OUTER_BOUND('',#4696,.T.);
#3054=FACE_OUTER_BOUND('',#4697,.T.);
#3055=FACE_OUTER_BOUND('',#4698,.T.);
#3056=FACE_OUTER_BOUND('',#4699,.T.);
#3057=FACE_OUTER_BOUND('',#4700,.T.);
#3058=FACE_OUTER_BOUND('',#4701,.T.);
#3059=FACE_OUTER_BOUND('',#4702,.T.);
#3060=FACE_OUTER_BOUND('',#4703,.T.);
#3061=FACE_OUTER_BOUND('',#4705,.T.);
#3062=FACE_OUTER_BOUND('',#4707,.T.);
#3063=FACE_OUTER_BOUND('',#4709,.T.);
#3064=FACE_OUTER_BOUND('',#4711,.T.);
#3065=FACE_OUTER_BOUND('',#4712,.T.);
#3066=FACE_OUTER_BOUND('',#4713,.T.);
#3067=FACE_OUTER_BOUND('',#4714,.T.);
#3068=FACE_OUTER_BOUND('',#4715,.T.);
#3069=FACE_OUTER_BOUND('',#4716,.T.);
#3070=FACE_OUTER_BOUND('',#4717,.T.);
#3071=FACE_OUTER_BOUND('',#4718,.T.);
#3072=FACE_OUTER_BOUND('',#4719,.T.);
#3073=FACE_OUTER_BOUND('',#4720,.T.);
#3074=FACE_OUTER_BOUND('',#4722,.T.);
#3075=FACE_OUTER_BOUND('',#4724,.T.);
#3076=FACE_OUTER_BOUND('',#4726,.T.);
#3077=FACE_OUTER_BOUND('',#4727,.T.);
#3078=FACE_OUTER_BOUND('',#4728,.T.);
#3079=FACE_OUTER_BOUND('',#4730,.T.);
#3080=FACE_OUTER_BOUND('',#4732,.T.);
#3081=FACE_OUTER_BOUND('',#4734,.T.);
#3082=FACE_OUTER_BOUND('',#4735,.T.);
#3083=FACE_OUTER_BOUND('',#4736,.T.);
#3084=FACE_OUTER_BOUND('',#4737,.T.);
#3085=FACE_OUTER_BOUND('',#4738,.T.);
#3086=FACE_OUTER_BOUND('',#4739,.T.);
#3087=FACE_OUTER_BOUND('',#4740,.T.);
#3088=FACE_OUTER_BOUND('',#4741,.T.);
#3089=FACE_OUTER_BOUND('',#4742,.T.);
#3090=FACE_OUTER_BOUND('',#4743,.T.);
#3091=FACE_OUTER_BOUND('',#4744,.T.);
#3092=FACE_OUTER_BOUND('',#4745,.T.);
#3093=FACE_OUTER_BOUND('',#4746,.T.);
#3094=FACE_OUTER_BOUND('',#4747,.T.);
#3095=FACE_OUTER_BOUND('',#4748,.T.);
#3096=FACE_OUTER_BOUND('',#4749,.T.);
#3097=FACE_OUTER_BOUND('',#4750,.T.);
#3098=FACE_OUTER_BOUND('',#4751,.T.);
#3099=FACE_OUTER_BOUND('',#4752,.T.);
#3100=FACE_OUTER_BOUND('',#4753,.T.);
#3101=FACE_OUTER_BOUND('',#4755,.T.);
#3102=FACE_OUTER_BOUND('',#4757,.T.);
#3103=FACE_OUTER_BOUND('',#4758,.T.);
#3104=FACE_OUTER_BOUND('',#4759,.T.);
#3105=FACE_OUTER_BOUND('',#4760,.T.);
#3106=FACE_OUTER_BOUND('',#4761,.T.);
#3107=FACE_OUTER_BOUND('',#4762,.T.);
#3108=FACE_OUTER_BOUND('',#4763,.T.);
#3109=FACE_OUTER_BOUND('',#4764,.T.);
#3110=FACE_OUTER_BOUND('',#4765,.T.);
#3111=FACE_OUTER_BOUND('',#4766,.T.);
#3112=FACE_OUTER_BOUND('',#4767,.T.);
#3113=FACE_OUTER_BOUND('',#4768,.T.);
#3114=FACE_OUTER_BOUND('',#4769,.T.);
#3115=FACE_OUTER_BOUND('',#4776,.T.);
#3116=FACE_OUTER_BOUND('',#4777,.T.);
#3117=FACE_OUTER_BOUND('',#4778,.T.);
#3118=FACE_OUTER_BOUND('',#4779,.T.);
#3119=FACE_OUTER_BOUND('',#4780,.T.);
#3120=FACE_OUTER_BOUND('',#4787,.T.);
#3121=FACE_OUTER_BOUND('',#4788,.T.);
#3122=FACE_OUTER_BOUND('',#4789,.T.);
#3123=FACE_OUTER_BOUND('',#4790,.T.);
#3124=FACE_OUTER_BOUND('',#4791,.T.);
#3125=FACE_OUTER_BOUND('',#4792,.T.);
#3126=FACE_OUTER_BOUND('',#4793,.T.);
#3127=FACE_OUTER_BOUND('',#4794,.T.);
#3128=FACE_OUTER_BOUND('',#4795,.T.);
#3129=FACE_OUTER_BOUND('',#4796,.T.);
#3130=FACE_OUTER_BOUND('',#4797,.T.);
#3131=FACE_OUTER_BOUND('',#4798,.T.);
#3132=FACE_OUTER_BOUND('',#4799,.T.);
#3133=FACE_OUTER_BOUND('',#4800,.T.);
#3134=FACE_OUTER_BOUND('',#4801,.T.);
#3135=FACE_OUTER_BOUND('',#4802,.T.);
#3136=FACE_OUTER_BOUND('',#4803,.T.);
#3137=FACE_OUTER_BOUND('',#4804,.T.);
#3138=FACE_OUTER_BOUND('',#4805,.T.);
#3139=FACE_OUTER_BOUND('',#4806,.T.);
#3140=FACE_OUTER_BOUND('',#4807,.T.);
#3141=FACE_OUTER_BOUND('',#4808,.T.);
#3142=FACE_OUTER_BOUND('',#4809,.T.);
#3143=FACE_OUTER_BOUND('',#4810,.T.);
#3144=FACE_OUTER_BOUND('',#4811,.T.);
#3145=FACE_OUTER_BOUND('',#4812,.T.);
#3146=FACE_OUTER_BOUND('',#4813,.T.);
#3147=FACE_OUTER_BOUND('',#4814,.T.);
#3148=FACE_OUTER_BOUND('',#4815,.T.);
#3149=FACE_OUTER_BOUND('',#4816,.T.);
#3150=FACE_OUTER_BOUND('',#4817,.T.);
#3151=FACE_OUTER_BOUND('',#4818,.T.);
#3152=FACE_OUTER_BOUND('',#4819,.T.);
#3153=FACE_OUTER_BOUND('',#4820,.T.);
#3154=FACE_OUTER_BOUND('',#4821,.T.);
#3155=FACE_OUTER_BOUND('',#4822,.T.);
#3156=FACE_OUTER_BOUND('',#4823,.T.);
#3157=FACE_OUTER_BOUND('',#4824,.T.);
#3158=FACE_OUTER_BOUND('',#4825,.T.);
#3159=FACE_OUTER_BOUND('',#4826,.T.);
#3160=FACE_OUTER_BOUND('',#4827,.T.);
#3161=FACE_OUTER_BOUND('',#4828,.T.);
#3162=FACE_OUTER_BOUND('',#4829,.T.);
#3163=FACE_OUTER_BOUND('',#4830,.T.);
#3164=FACE_OUTER_BOUND('',#4831,.T.);
#3165=FACE_OUTER_BOUND('',#4832,.T.);
#3166=FACE_OUTER_BOUND('',#4833,.T.);
#3167=FACE_OUTER_BOUND('',#4834,.T.);
#3168=FACE_OUTER_BOUND('',#4835,.T.);
#3169=FACE_OUTER_BOUND('',#4836,.T.);
#3170=FACE_OUTER_BOUND('',#4837,.T.);
#3171=FACE_OUTER_BOUND('',#4838,.T.);
#3172=FACE_OUTER_BOUND('',#4839,.T.);
#3173=FACE_OUTER_BOUND('',#4840,.T.);
#3174=FACE_OUTER_BOUND('',#4841,.T.);
#3175=FACE_OUTER_BOUND('',#4842,.T.);
#3176=FACE_OUTER_BOUND('',#4843,.T.);
#3177=FACE_OUTER_BOUND('',#4844,.T.);
#3178=FACE_OUTER_BOUND('',#4845,.T.);
#3179=FACE_OUTER_BOUND('',#4846,.T.);
#3180=FACE_OUTER_BOUND('',#4847,.T.);
#3181=FACE_OUTER_BOUND('',#4848,.T.);
#3182=FACE_OUTER_BOUND('',#4849,.T.);
#3183=FACE_OUTER_BOUND('',#4850,.T.);
#3184=FACE_OUTER_BOUND('',#4851,.T.);
#3185=FACE_OUTER_BOUND('',#4852,.T.);
#3186=FACE_OUTER_BOUND('',#4853,.T.);
#3187=FACE_OUTER_BOUND('',#4854,.T.);
#3188=FACE_OUTER_BOUND('',#4855,.T.);
#3189=FACE_OUTER_BOUND('',#4856,.T.);
#3190=FACE_OUTER_BOUND('',#4857,.T.);
#3191=FACE_OUTER_BOUND('',#4858,.T.);
#3192=FACE_OUTER_BOUND('',#4859,.T.);
#3193=FACE_OUTER_BOUND('',#4860,.T.);
#3194=FACE_OUTER_BOUND('',#4861,.T.);
#3195=FACE_OUTER_BOUND('',#4862,.T.);
#3196=FACE_OUTER_BOUND('',#4863,.T.);
#3197=FACE_OUTER_BOUND('',#4864,.T.);
#3198=FACE_OUTER_BOUND('',#4865,.T.);
#3199=FACE_OUTER_BOUND('',#4866,.T.);
#3200=FACE_OUTER_BOUND('',#4867,.T.);
#3201=FACE_OUTER_BOUND('',#4868,.T.);
#3202=FACE_OUTER_BOUND('',#4869,.T.);
#3203=FACE_OUTER_BOUND('',#4870,.T.);
#3204=FACE_OUTER_BOUND('',#4871,.T.);
#3205=FACE_OUTER_BOUND('',#4872,.T.);
#3206=FACE_OUTER_BOUND('',#4873,.T.);
#3207=FACE_OUTER_BOUND('',#4874,.T.);
#3208=FACE_OUTER_BOUND('',#4875,.T.);
#3209=FACE_OUTER_BOUND('',#4876,.T.);
#3210=FACE_OUTER_BOUND('',#4877,.T.);
#3211=FACE_OUTER_BOUND('',#4878,.T.);
#3212=FACE_OUTER_BOUND('',#4879,.T.);
#3213=FACE_OUTER_BOUND('',#4880,.T.);
#3214=FACE_OUTER_BOUND('',#4881,.T.);
#3215=FACE_OUTER_BOUND('',#4882,.T.);
#3216=FACE_OUTER_BOUND('',#4883,.T.);
#3217=FACE_OUTER_BOUND('',#4884,.T.);
#3218=FACE_OUTER_BOUND('',#4885,.T.);
#3219=FACE_OUTER_BOUND('',#4886,.T.);
#3220=FACE_OUTER_BOUND('',#4887,.T.);
#3221=FACE_OUTER_BOUND('',#4888,.T.);
#3222=FACE_OUTER_BOUND('',#4889,.T.);
#3223=FACE_OUTER_BOUND('',#4890,.T.);
#3224=FACE_OUTER_BOUND('',#4891,.T.);
#3225=FACE_OUTER_BOUND('',#4892,.T.);
#3226=FACE_OUTER_BOUND('',#4893,.T.);
#3227=FACE_OUTER_BOUND('',#4894,.T.);
#3228=FACE_OUTER_BOUND('',#4895,.T.);
#3229=FACE_OUTER_BOUND('',#4896,.T.);
#3230=FACE_OUTER_BOUND('',#4897,.T.);
#3231=FACE_OUTER_BOUND('',#4898,.T.);
#3232=FACE_OUTER_BOUND('',#4899,.T.);
#3233=FACE_OUTER_BOUND('',#4900,.T.);
#3234=FACE_OUTER_BOUND('',#4901,.T.);
#3235=FACE_OUTER_BOUND('',#4902,.T.);
#3236=FACE_OUTER_BOUND('',#4903,.T.);
#3237=FACE_OUTER_BOUND('',#4904,.T.);
#3238=FACE_OUTER_BOUND('',#4905,.T.);
#3239=FACE_OUTER_BOUND('',#4906,.T.);
#3240=FACE_OUTER_BOUND('',#4907,.T.);
#3241=FACE_OUTER_BOUND('',#4908,.T.);
#3242=FACE_OUTER_BOUND('',#4909,.T.);
#3243=FACE_OUTER_BOUND('',#4910,.T.);
#3244=FACE_OUTER_BOUND('',#4911,.T.);
#3245=FACE_OUTER_BOUND('',#4912,.T.);
#3246=FACE_OUTER_BOUND('',#4913,.T.);
#3247=FACE_OUTER_BOUND('',#4914,.T.);
#3248=FACE_OUTER_BOUND('',#4915,.T.);
#3249=FACE_OUTER_BOUND('',#4916,.T.);
#3250=FACE_OUTER_BOUND('',#4917,.T.);
#3251=FACE_OUTER_BOUND('',#4918,.T.);
#3252=FACE_OUTER_BOUND('',#4919,.T.);
#3253=FACE_OUTER_BOUND('',#4920,.T.);
#3254=FACE_OUTER_BOUND('',#4921,.T.);
#3255=FACE_OUTER_BOUND('',#4922,.T.);
#3256=FACE_OUTER_BOUND('',#4923,.T.);
#3257=FACE_OUTER_BOUND('',#4924,.T.);
#3258=FACE_OUTER_BOUND('',#4925,.T.);
#3259=FACE_OUTER_BOUND('',#4926,.T.);
#3260=FACE_OUTER_BOUND('',#4927,.T.);
#3261=FACE_OUTER_BOUND('',#4928,.T.);
#3262=FACE_OUTER_BOUND('',#4929,.T.);
#3263=FACE_OUTER_BOUND('',#4930,.T.);
#3264=FACE_OUTER_BOUND('',#4931,.T.);
#3265=FACE_OUTER_BOUND('',#4932,.T.);
#3266=FACE_OUTER_BOUND('',#4933,.T.);
#3267=FACE_OUTER_BOUND('',#4934,.T.);
#3268=FACE_OUTER_BOUND('',#4935,.T.);
#3269=FACE_OUTER_BOUND('',#4936,.T.);
#3270=FACE_OUTER_BOUND('',#4937,.T.);
#3271=FACE_OUTER_BOUND('',#4938,.T.);
#3272=FACE_OUTER_BOUND('',#4939,.T.);
#3273=FACE_OUTER_BOUND('',#4940,.T.);
#3274=FACE_OUTER_BOUND('',#4941,.T.);
#3275=FACE_OUTER_BOUND('',#4942,.T.);
#3276=FACE_OUTER_BOUND('',#4943,.T.);
#3277=FACE_OUTER_BOUND('',#4944,.T.);
#3278=FACE_OUTER_BOUND('',#4945,.T.);
#3279=FACE_OUTER_BOUND('',#4946,.T.);
#3280=FACE_OUTER_BOUND('',#4947,.T.);
#3281=FACE_OUTER_BOUND('',#4948,.T.);
#3282=FACE_OUTER_BOUND('',#4949,.T.);
#3283=FACE_OUTER_BOUND('',#4950,.T.);
#3284=FACE_OUTER_BOUND('',#4951,.T.);
#3285=FACE_OUTER_BOUND('',#4952,.T.);
#3286=FACE_OUTER_BOUND('',#4953,.T.);
#3287=FACE_OUTER_BOUND('',#4954,.T.);
#3288=FACE_OUTER_BOUND('',#4955,.T.);
#3289=FACE_OUTER_BOUND('',#4956,.T.);
#3290=FACE_OUTER_BOUND('',#4957,.T.);
#3291=FACE_OUTER_BOUND('',#4958,.T.);
#3292=FACE_OUTER_BOUND('',#4959,.T.);
#3293=FACE_OUTER_BOUND('',#4960,.T.);
#3294=FACE_OUTER_BOUND('',#4961,.T.);
#3295=FACE_OUTER_BOUND('',#4962,.T.);
#3296=FACE_OUTER_BOUND('',#4963,.T.);
#3297=FACE_OUTER_BOUND('',#4964,.T.);
#3298=FACE_OUTER_BOUND('',#4965,.T.);
#3299=FACE_OUTER_BOUND('',#4966,.T.);
#3300=FACE_OUTER_BOUND('',#4967,.T.);
#3301=FACE_OUTER_BOUND('',#4968,.T.);
#3302=FACE_OUTER_BOUND('',#4969,.T.);
#3303=FACE_OUTER_BOUND('',#4970,.T.);
#3304=FACE_OUTER_BOUND('',#4971,.T.);
#3305=FACE_OUTER_BOUND('',#4972,.T.);
#3306=FACE_OUTER_BOUND('',#4973,.T.);
#3307=FACE_OUTER_BOUND('',#4979,.T.);
#3308=FACE_OUTER_BOUND('',#4980,.T.);
#3309=FACE_OUTER_BOUND('',#4981,.T.);
#3310=FACE_OUTER_BOUND('',#4982,.T.);
#3311=FACE_OUTER_BOUND('',#4983,.T.);
#3312=FACE_OUTER_BOUND('',#4984,.T.);
#3313=FACE_OUTER_BOUND('',#4985,.T.);
#3314=FACE_OUTER_BOUND('',#4986,.T.);
#3315=FACE_OUTER_BOUND('',#4992,.T.);
#3316=FACE_OUTER_BOUND('',#4994,.T.);
#3317=FACE_OUTER_BOUND('',#4995,.T.);
#3318=FACE_OUTER_BOUND('',#4996,.T.);
#3319=FACE_OUTER_BOUND('',#4997,.T.);
#3320=FACE_OUTER_BOUND('',#4998,.T.);
#3321=FACE_OUTER_BOUND('',#4999,.T.);
#3322=FACE_OUTER_BOUND('',#5000,.T.);
#3323=FACE_OUTER_BOUND('',#5001,.T.);
#3324=FACE_OUTER_BOUND('',#5002,.T.);
#3325=FACE_OUTER_BOUND('',#5003,.T.);
#3326=FACE_OUTER_BOUND('',#5005,.T.);
#3327=FACE_OUTER_BOUND('',#5006,.T.);
#3328=FACE_OUTER_BOUND('',#5007,.T.);
#3329=FACE_OUTER_BOUND('',#5009,.T.);
#3330=FACE_OUTER_BOUND('',#5010,.T.);
#3331=FACE_OUTER_BOUND('',#5011,.T.);
#3332=FACE_OUTER_BOUND('',#5012,.T.);
#3333=FACE_OUTER_BOUND('',#5013,.T.);
#3334=FACE_OUTER_BOUND('',#5014,.T.);
#3335=FACE_OUTER_BOUND('',#5015,.T.);
#3336=FACE_OUTER_BOUND('',#5016,.T.);
#3337=FACE_OUTER_BOUND('',#5017,.T.);
#3338=FACE_OUTER_BOUND('',#5018,.T.);
#3339=FACE_OUTER_BOUND('',#5019,.T.);
#3340=FACE_OUTER_BOUND('',#5021,.T.);
#3341=FACE_OUTER_BOUND('',#5022,.T.);
#3342=FACE_OUTER_BOUND('',#5023,.T.);
#3343=FACE_OUTER_BOUND('',#5025,.T.);
#3344=FACE_OUTER_BOUND('',#5026,.T.);
#3345=FACE_OUTER_BOUND('',#5027,.T.);
#3346=FACE_OUTER_BOUND('',#5028,.T.);
#3347=FACE_OUTER_BOUND('',#5029,.T.);
#3348=FACE_OUTER_BOUND('',#5030,.T.);
#3349=FACE_OUTER_BOUND('',#5031,.T.);
#3350=FACE_OUTER_BOUND('',#5032,.T.);
#3351=FACE_OUTER_BOUND('',#5033,.T.);
#3352=FACE_OUTER_BOUND('',#5034,.T.);
#3353=FACE_OUTER_BOUND('',#5035,.T.);
#3354=FACE_OUTER_BOUND('',#5036,.T.);
#3355=FACE_OUTER_BOUND('',#5037,.T.);
#3356=FACE_OUTER_BOUND('',#5038,.T.);
#3357=FACE_OUTER_BOUND('',#5039,.T.);
#3358=FACE_OUTER_BOUND('',#5040,.T.);
#3359=FACE_OUTER_BOUND('',#5041,.T.);
#3360=FACE_OUTER_BOUND('',#5042,.T.);
#3361=FACE_OUTER_BOUND('',#5043,.T.);
#3362=FACE_OUTER_BOUND('',#5044,.T.);
#3363=FACE_OUTER_BOUND('',#5045,.T.);
#3364=FACE_OUTER_BOUND('',#5048,.T.);
#3365=FACE_OUTER_BOUND('',#5049,.T.);
#3366=FACE_OUTER_BOUND('',#5050,.T.);
#3367=FACE_OUTER_BOUND('',#5051,.T.);
#3368=FACE_OUTER_BOUND('',#5053,.T.);
#3369=FACE_OUTER_BOUND('',#5054,.T.);
#3370=FACE_OUTER_BOUND('',#5056,.T.);
#3371=FACE_OUTER_BOUND('',#5057,.T.);
#3372=FACE_OUTER_BOUND('',#5059,.T.);
#3373=FACE_OUTER_BOUND('',#5061,.T.);
#3374=FACE_OUTER_BOUND('',#5062,.T.);
#3375=FACE_OUTER_BOUND('',#5063,.T.);
#3376=FACE_OUTER_BOUND('',#5065,.T.);
#3377=FACE_OUTER_BOUND('',#5066,.T.);
#3378=FACE_OUTER_BOUND('',#5067,.T.);
#3379=FACE_OUTER_BOUND('',#5069,.T.);
#3380=FACE_OUTER_BOUND('',#5070,.T.);
#3381=FACE_OUTER_BOUND('',#5072,.T.);
#3382=FACE_OUTER_BOUND('',#5074,.T.);
#3383=FACE_OUTER_BOUND('',#5075,.T.);
#3384=FACE_OUTER_BOUND('',#5076,.T.);
#3385=FACE_OUTER_BOUND('',#5077,.T.);
#3386=FACE_OUTER_BOUND('',#5078,.T.);
#3387=FACE_OUTER_BOUND('',#5079,.T.);
#3388=FACE_OUTER_BOUND('',#5080,.T.);
#3389=FACE_OUTER_BOUND('',#5081,.T.);
#3390=FACE_OUTER_BOUND('',#5082,.T.);
#3391=FACE_OUTER_BOUND('',#5083,.T.);
#3392=FACE_OUTER_BOUND('',#5084,.T.);
#3393=FACE_OUTER_BOUND('',#5085,.T.);
#3394=FACE_OUTER_BOUND('',#5086,.T.);
#3395=FACE_OUTER_BOUND('',#5087,.T.);
#3396=FACE_OUTER_BOUND('',#5088,.T.);
#3397=FACE_OUTER_BOUND('',#5089,.T.);
#3398=FACE_OUTER_BOUND('',#5090,.T.);
#3399=FACE_OUTER_BOUND('',#5091,.T.);
#3400=FACE_OUTER_BOUND('',#5092,.T.);
#3401=FACE_OUTER_BOUND('',#5093,.T.);
#3402=FACE_OUTER_BOUND('',#5094,.T.);
#3403=FACE_OUTER_BOUND('',#5095,.T.);
#3404=FACE_OUTER_BOUND('',#5104,.T.);
#3405=FACE_OUTER_BOUND('',#5105,.T.);
#3406=FACE_OUTER_BOUND('',#5106,.T.);
#3407=FACE_OUTER_BOUND('',#5107,.T.);
#3408=FACE_OUTER_BOUND('',#5108,.T.);
#3409=FACE_OUTER_BOUND('',#5109,.T.);
#3410=FACE_OUTER_BOUND('',#5110,.T.);
#3411=FACE_OUTER_BOUND('',#5111,.T.);
#3412=FACE_OUTER_BOUND('',#5112,.T.);
#3413=FACE_OUTER_BOUND('',#5113,.T.);
#3414=FACE_OUTER_BOUND('',#5114,.T.);
#3415=FACE_OUTER_BOUND('',#5115,.T.);
#3416=FACE_OUTER_BOUND('',#5116,.T.);
#3417=FACE_OUTER_BOUND('',#5117,.T.);
#3418=FACE_OUTER_BOUND('',#5118,.T.);
#3419=FACE_OUTER_BOUND('',#5119,.T.);
#3420=FACE_OUTER_BOUND('',#5120,.T.);
#3421=FACE_OUTER_BOUND('',#5121,.T.);
#3422=FACE_OUTER_BOUND('',#5122,.T.);
#3423=FACE_OUTER_BOUND('',#5123,.T.);
#3424=FACE_OUTER_BOUND('',#5124,.T.);
#3425=FACE_OUTER_BOUND('',#5125,.T.);
#3426=FACE_OUTER_BOUND('',#5126,.T.);
#3427=FACE_OUTER_BOUND('',#5127,.T.);
#3428=FACE_OUTER_BOUND('',#5128,.T.);
#3429=FACE_OUTER_BOUND('',#5129,.T.);
#3430=FACE_OUTER_BOUND('',#5130,.T.);
#3431=FACE_OUTER_BOUND('',#5131,.T.);
#3432=FACE_OUTER_BOUND('',#5132,.T.);
#3433=FACE_OUTER_BOUND('',#5133,.T.);
#3434=FACE_OUTER_BOUND('',#5134,.T.);
#3435=FACE_OUTER_BOUND('',#5135,.T.);
#3436=FACE_OUTER_BOUND('',#5136,.T.);
#3437=FACE_OUTER_BOUND('',#5137,.T.);
#3438=FACE_OUTER_BOUND('',#5138,.T.);
#3439=FACE_OUTER_BOUND('',#5139,.T.);
#3440=FACE_OUTER_BOUND('',#5140,.T.);
#3441=FACE_OUTER_BOUND('',#5141,.T.);
#3442=FACE_OUTER_BOUND('',#5142,.T.);
#3443=FACE_OUTER_BOUND('',#5143,.T.);
#3444=FACE_OUTER_BOUND('',#5144,.T.);
#3445=FACE_OUTER_BOUND('',#5145,.T.);
#3446=FACE_OUTER_BOUND('',#5146,.T.);
#3447=FACE_OUTER_BOUND('',#5147,.T.);
#3448=FACE_OUTER_BOUND('',#5148,.T.);
#3449=FACE_OUTER_BOUND('',#5149,.T.);
#3450=FACE_OUTER_BOUND('',#5150,.T.);
#3451=FACE_OUTER_BOUND('',#5151,.T.);
#3452=FACE_OUTER_BOUND('',#5152,.T.);
#3453=FACE_OUTER_BOUND('',#5154,.T.);
#3454=FACE_OUTER_BOUND('',#5156,.T.);
#3455=FACE_OUTER_BOUND('',#5157,.T.);
#3456=FACE_OUTER_BOUND('',#5158,.T.);
#3457=FACE_OUTER_BOUND('',#5159,.T.);
#3458=FACE_OUTER_BOUND('',#5160,.T.);
#3459=FACE_OUTER_BOUND('',#5161,.T.);
#3460=FACE_OUTER_BOUND('',#5162,.T.);
#3461=FACE_OUTER_BOUND('',#5163,.T.);
#3462=FACE_OUTER_BOUND('',#5164,.T.);
#3463=FACE_OUTER_BOUND('',#5165,.T.);
#3464=FACE_OUTER_BOUND('',#5167,.T.);
#3465=FACE_OUTER_BOUND('',#5168,.T.);
#3466=FACE_OUTER_BOUND('',#5169,.T.);
#3467=FACE_OUTER_BOUND('',#5171,.T.);
#3468=FACE_OUTER_BOUND('',#5172,.T.);
#3469=FACE_OUTER_BOUND('',#5173,.T.);
#3470=FACE_OUTER_BOUND('',#5174,.T.);
#3471=FACE_OUTER_BOUND('',#5175,.T.);
#3472=FACE_OUTER_BOUND('',#5176,.T.);
#3473=FACE_OUTER_BOUND('',#5177,.T.);
#3474=FACE_OUTER_BOUND('',#5178,.T.);
#3475=FACE_OUTER_BOUND('',#5179,.T.);
#3476=FACE_OUTER_BOUND('',#5180,.T.);
#3477=FACE_OUTER_BOUND('',#5181,.T.);
#3478=FACE_OUTER_BOUND('',#5183,.T.);
#3479=FACE_OUTER_BOUND('',#5184,.T.);
#3480=FACE_OUTER_BOUND('',#5185,.T.);
#3481=FACE_OUTER_BOUND('',#5187,.T.);
#3482=FACE_OUTER_BOUND('',#5188,.T.);
#3483=FACE_OUTER_BOUND('',#5189,.T.);
#3484=FACE_OUTER_BOUND('',#5190,.T.);
#3485=FACE_OUTER_BOUND('',#5191,.T.);
#3486=FACE_OUTER_BOUND('',#5192,.T.);
#3487=FACE_OUTER_BOUND('',#5193,.T.);
#3488=FACE_OUTER_BOUND('',#5194,.T.);
#3489=FACE_OUTER_BOUND('',#5195,.T.);
#3490=FACE_OUTER_BOUND('',#5196,.T.);
#3491=FACE_OUTER_BOUND('',#5197,.T.);
#3492=FACE_OUTER_BOUND('',#5198,.T.);
#3493=FACE_OUTER_BOUND('',#5199,.T.);
#3494=FACE_OUTER_BOUND('',#5200,.T.);
#3495=FACE_OUTER_BOUND('',#5201,.T.);
#3496=FACE_OUTER_BOUND('',#5202,.T.);
#3497=FACE_OUTER_BOUND('',#5203,.T.);
#3498=FACE_OUTER_BOUND('',#5204,.T.);
#3499=FACE_OUTER_BOUND('',#5205,.T.);
#3500=FACE_OUTER_BOUND('',#5206,.T.);
#3501=FACE_OUTER_BOUND('',#5207,.T.);
#3502=FACE_OUTER_BOUND('',#5210,.T.);
#3503=FACE_OUTER_BOUND('',#5211,.T.);
#3504=FACE_OUTER_BOUND('',#5212,.T.);
#3505=FACE_OUTER_BOUND('',#5213,.T.);
#3506=FACE_OUTER_BOUND('',#5215,.T.);
#3507=FACE_OUTER_BOUND('',#5216,.T.);
#3508=FACE_OUTER_BOUND('',#5218,.T.);
#3509=FACE_OUTER_BOUND('',#5219,.T.);
#3510=FACE_OUTER_BOUND('',#5221,.T.);
#3511=FACE_OUTER_BOUND('',#5223,.T.);
#3512=FACE_OUTER_BOUND('',#5224,.T.);
#3513=FACE_OUTER_BOUND('',#5225,.T.);
#3514=FACE_OUTER_BOUND('',#5227,.T.);
#3515=FACE_OUTER_BOUND('',#5228,.T.);
#3516=FACE_OUTER_BOUND('',#5229,.T.);
#3517=FACE_OUTER_BOUND('',#5231,.T.);
#3518=FACE_OUTER_BOUND('',#5232,.T.);
#3519=FACE_OUTER_BOUND('',#5234,.T.);
#3520=FACE_OUTER_BOUND('',#5236,.T.);
#3521=FACE_OUTER_BOUND('',#5237,.T.);
#3522=FACE_OUTER_BOUND('',#5238,.T.);
#3523=FACE_OUTER_BOUND('',#5239,.T.);
#3524=FACE_OUTER_BOUND('',#5240,.T.);
#3525=FACE_OUTER_BOUND('',#5241,.T.);
#3526=FACE_OUTER_BOUND('',#5242,.T.);
#3527=FACE_OUTER_BOUND('',#5243,.T.);
#3528=FACE_OUTER_BOUND('',#5244,.T.);
#3529=FACE_OUTER_BOUND('',#5245,.T.);
#3530=FACE_OUTER_BOUND('',#5247,.T.);
#3531=FACE_OUTER_BOUND('',#5248,.T.);
#3532=FACE_OUTER_BOUND('',#5249,.T.);
#3533=FACE_OUTER_BOUND('',#5250,.T.);
#3534=FACE_OUTER_BOUND('',#5251,.T.);
#3535=FACE_OUTER_BOUND('',#5252,.T.);
#3536=FACE_OUTER_BOUND('',#5253,.T.);
#3537=FACE_OUTER_BOUND('',#5254,.T.);
#3538=FACE_OUTER_BOUND('',#5255,.T.);
#3539=FACE_OUTER_BOUND('',#5264,.T.);
#3540=FACE_OUTER_BOUND('',#5265,.T.);
#3541=FACE_OUTER_BOUND('',#5266,.T.);
#3542=FACE_OUTER_BOUND('',#5267,.T.);
#3543=FACE_OUTER_BOUND('',#5268,.T.);
#3544=FACE_OUTER_BOUND('',#5269,.T.);
#3545=FACE_OUTER_BOUND('',#5270,.T.);
#3546=FACE_OUTER_BOUND('',#5271,.T.);
#3547=FACE_OUTER_BOUND('',#5272,.T.);
#3548=FACE_OUTER_BOUND('',#5273,.T.);
#3549=FACE_OUTER_BOUND('',#5274,.T.);
#3550=FACE_OUTER_BOUND('',#5275,.T.);
#3551=FACE_OUTER_BOUND('',#5276,.T.);
#3552=FACE_OUTER_BOUND('',#5277,.T.);
#3553=FACE_OUTER_BOUND('',#5278,.T.);
#3554=FACE_OUTER_BOUND('',#5279,.T.);
#3555=FACE_OUTER_BOUND('',#5280,.T.);
#3556=FACE_OUTER_BOUND('',#5281,.T.);
#3557=FACE_OUTER_BOUND('',#5282,.T.);
#3558=FACE_OUTER_BOUND('',#5283,.T.);
#3559=FACE_OUTER_BOUND('',#5284,.T.);
#3560=FACE_OUTER_BOUND('',#5285,.T.);
#3561=FACE_OUTER_BOUND('',#5286,.T.);
#3562=FACE_OUTER_BOUND('',#5287,.T.);
#3563=FACE_OUTER_BOUND('',#5288,.T.);
#3564=FACE_OUTER_BOUND('',#5289,.T.);
#3565=FACE_OUTER_BOUND('',#5290,.T.);
#3566=FACE_OUTER_BOUND('',#5291,.T.);
#3567=FACE_OUTER_BOUND('',#5292,.T.);
#3568=FACE_OUTER_BOUND('',#5293,.T.);
#3569=FACE_OUTER_BOUND('',#5294,.T.);
#3570=FACE_OUTER_BOUND('',#5295,.T.);
#3571=FACE_OUTER_BOUND('',#5296,.T.);
#3572=FACE_OUTER_BOUND('',#5297,.T.);
#3573=FACE_OUTER_BOUND('',#5298,.T.);
#3574=FACE_OUTER_BOUND('',#5299,.T.);
#3575=FACE_OUTER_BOUND('',#5300,.T.);
#3576=FACE_OUTER_BOUND('',#5301,.T.);
#3577=FACE_OUTER_BOUND('',#5302,.T.);
#3578=FACE_OUTER_BOUND('',#5303,.T.);
#3579=FACE_OUTER_BOUND('',#5304,.T.);
#3580=FACE_OUTER_BOUND('',#5305,.T.);
#3581=FACE_OUTER_BOUND('',#5306,.T.);
#3582=FACE_OUTER_BOUND('',#5307,.T.);
#3583=FACE_OUTER_BOUND('',#5308,.T.);
#3584=FACE_OUTER_BOUND('',#5309,.T.);
#3585=FACE_OUTER_BOUND('',#5310,.T.);
#3586=FACE_OUTER_BOUND('',#5311,.T.);
#3587=FACE_OUTER_BOUND('',#5312,.T.);
#3588=FACE_OUTER_BOUND('',#5314,.T.);
#3589=FACE_OUTER_BOUND('',#5315,.T.);
#3590=FACE_OUTER_BOUND('',#5316,.T.);
#3591=FACE_OUTER_BOUND('',#5317,.T.);
#3592=FACE_OUTER_BOUND('',#5318,.T.);
#3593=FACE_OUTER_BOUND('',#5319,.T.);
#3594=FACE_OUTER_BOUND('',#5320,.T.);
#3595=FACE_OUTER_BOUND('',#5321,.T.);
#3596=FACE_OUTER_BOUND('',#5322,.T.);
#3597=FACE_OUTER_BOUND('',#5323,.T.);
#3598=FACE_OUTER_BOUND('',#5324,.T.);
#3599=FACE_OUTER_BOUND('',#5325,.T.);
#3600=FACE_OUTER_BOUND('',#5326,.T.);
#3601=FACE_OUTER_BOUND('',#5327,.T.);
#3602=FACE_OUTER_BOUND('',#5328,.T.);
#3603=FACE_OUTER_BOUND('',#5329,.T.);
#3604=FACE_OUTER_BOUND('',#5330,.T.);
#3605=FACE_OUTER_BOUND('',#5331,.T.);
#3606=FACE_OUTER_BOUND('',#5332,.T.);
#3607=FACE_OUTER_BOUND('',#5333,.T.);
#3608=FACE_OUTER_BOUND('',#5334,.T.);
#3609=FACE_OUTER_BOUND('',#5335,.T.);
#3610=FACE_OUTER_BOUND('',#5336,.T.);
#3611=FACE_OUTER_BOUND('',#5337,.T.);
#3612=FACE_OUTER_BOUND('',#5338,.T.);
#3613=FACE_OUTER_BOUND('',#5339,.T.);
#3614=FACE_OUTER_BOUND('',#5340,.T.);
#3615=FACE_OUTER_BOUND('',#5341,.T.);
#3616=FACE_OUTER_BOUND('',#5342,.T.);
#3617=FACE_OUTER_BOUND('',#5343,.T.);
#3618=FACE_OUTER_BOUND('',#5344,.T.);
#3619=FACE_OUTER_BOUND('',#5345,.T.);
#3620=FACE_OUTER_BOUND('',#5346,.T.);
#3621=FACE_OUTER_BOUND('',#5347,.T.);
#3622=FACE_OUTER_BOUND('',#5348,.T.);
#3623=FACE_OUTER_BOUND('',#5349,.T.);
#3624=FACE_OUTER_BOUND('',#5350,.T.);
#3625=FACE_OUTER_BOUND('',#5351,.T.);
#3626=FACE_OUTER_BOUND('',#5352,.T.);
#3627=FACE_OUTER_BOUND('',#5353,.T.);
#3628=FACE_OUTER_BOUND('',#5354,.T.);
#3629=FACE_OUTER_BOUND('',#5355,.T.);
#3630=FACE_OUTER_BOUND('',#5356,.T.);
#3631=FACE_OUTER_BOUND('',#5374,.T.);
#3632=FACE_OUTER_BOUND('',#5375,.T.);
#3633=FACE_OUTER_BOUND('',#5376,.T.);
#3634=FACE_OUTER_BOUND('',#5377,.T.);
#3635=FACE_OUTER_BOUND('',#5378,.T.);
#3636=FACE_OUTER_BOUND('',#5379,.T.);
#3637=FACE_OUTER_BOUND('',#5380,.T.);
#3638=FACE_OUTER_BOUND('',#5381,.T.);
#3639=FACE_OUTER_BOUND('',#5382,.T.);
#3640=FACE_OUTER_BOUND('',#5384,.T.);
#3641=FACE_OUTER_BOUND('',#5386,.T.);
#3642=FACE_OUTER_BOUND('',#5387,.T.);
#3643=FACE_OUTER_BOUND('',#5388,.T.);
#3644=FACE_OUTER_BOUND('',#5389,.T.);
#3645=FACE_OUTER_BOUND('',#5390,.T.);
#3646=FACE_OUTER_BOUND('',#5391,.T.);
#3647=FACE_OUTER_BOUND('',#5392,.T.);
#3648=FACE_OUTER_BOUND('',#5393,.T.);
#3649=FACE_OUTER_BOUND('',#5394,.T.);
#3650=FACE_OUTER_BOUND('',#5395,.T.);
#3651=FACE_OUTER_BOUND('',#5396,.T.);
#3652=FACE_OUTER_BOUND('',#5397,.T.);
#3653=FACE_OUTER_BOUND('',#5398,.T.);
#3654=FACE_OUTER_BOUND('',#5400,.T.);
#3655=FACE_OUTER_BOUND('',#5401,.T.);
#3656=FACE_OUTER_BOUND('',#5403,.T.);
#3657=FACE_OUTER_BOUND('',#5405,.T.);
#3658=FACE_OUTER_BOUND('',#5406,.T.);
#3659=FACE_OUTER_BOUND('',#5407,.T.);
#3660=FACE_OUTER_BOUND('',#5408,.T.);
#3661=FACE_OUTER_BOUND('',#5409,.T.);
#3662=FACE_OUTER_BOUND('',#5410,.T.);
#3663=FACE_OUTER_BOUND('',#5411,.T.);
#3664=FACE_OUTER_BOUND('',#5412,.T.);
#3665=FACE_OUTER_BOUND('',#5413,.T.);
#3666=FACE_OUTER_BOUND('',#5414,.T.);
#3667=FACE_OUTER_BOUND('',#5415,.T.);
#3668=FACE_OUTER_BOUND('',#5416,.T.);
#3669=FACE_OUTER_BOUND('',#5417,.T.);
#3670=FACE_OUTER_BOUND('',#5418,.T.);
#3671=FACE_OUTER_BOUND('',#5419,.T.);
#3672=FACE_OUTER_BOUND('',#5421,.T.);
#3673=FACE_OUTER_BOUND('',#5423,.T.);
#3674=FACE_OUTER_BOUND('',#5424,.T.);
#3675=FACE_OUTER_BOUND('',#5425,.T.);
#3676=FACE_OUTER_BOUND('',#5426,.T.);
#3677=FACE_OUTER_BOUND('',#5427,.T.);
#3678=FACE_OUTER_BOUND('',#5428,.T.);
#3679=FACE_OUTER_BOUND('',#5429,.T.);
#3680=FACE_OUTER_BOUND('',#5430,.T.);
#3681=FACE_OUTER_BOUND('',#5431,.T.);
#3682=FACE_OUTER_BOUND('',#5432,.T.);
#3683=FACE_OUTER_BOUND('',#5433,.T.);
#3684=FACE_OUTER_BOUND('',#5434,.T.);
#3685=FACE_OUTER_BOUND('',#5435,.T.);
#3686=FACE_OUTER_BOUND('',#5436,.T.);
#3687=FACE_OUTER_BOUND('',#5437,.T.);
#3688=FACE_OUTER_BOUND('',#5438,.T.);
#3689=FACE_OUTER_BOUND('',#5439,.T.);
#3690=FACE_OUTER_BOUND('',#5450,.T.);
#3691=FACE_OUTER_BOUND('',#5451,.T.);
#3692=FACE_OUTER_BOUND('',#5452,.T.);
#3693=FACE_OUTER_BOUND('',#5453,.T.);
#3694=FACE_OUTER_BOUND('',#5454,.T.);
#3695=FACE_OUTER_BOUND('',#5465,.T.);
#3696=FACE_OUTER_BOUND('',#5466,.T.);
#3697=FACE_OUTER_BOUND('',#5467,.T.);
#3698=FACE_OUTER_BOUND('',#5468,.T.);
#3699=FACE_OUTER_BOUND('',#5469,.T.);
#3700=FACE_OUTER_BOUND('',#5470,.T.);
#3701=FACE_OUTER_BOUND('',#5471,.T.);
#3702=FACE_OUTER_BOUND('',#5472,.T.);
#3703=FACE_OUTER_BOUND('',#5474,.T.);
#3704=FACE_OUTER_BOUND('',#5476,.T.);
#3705=FACE_OUTER_BOUND('',#5477,.T.);
#3706=FACE_OUTER_BOUND('',#5478,.T.);
#3707=FACE_OUTER_BOUND('',#5479,.T.);
#3708=FACE_OUTER_BOUND('',#5480,.T.);
#3709=FACE_OUTER_BOUND('',#5481,.T.);
#3710=FACE_OUTER_BOUND('',#5482,.T.);
#3711=EDGE_LOOP('',(#16594,#16595,#16596,#16597));
#3712=EDGE_LOOP('',(#16598,#16599,#16600,#16601));
#3713=EDGE_LOOP('',(#16602,#16603,#16604,#16605));
#3714=EDGE_LOOP('',(#16606,#16607,#16608,#16609));
#3715=EDGE_LOOP('',(#16610,#16611,#16612,#16613));
#3716=EDGE_LOOP('',(#16614,#16615,#16616,#16617));
#3717=EDGE_LOOP('',(#16618,#16619,#16620,#16621));
#3718=EDGE_LOOP('',(#16622,#16623,#16624,#16625));
#3719=EDGE_LOOP('',(#16626,#16627,#16628,#16629));
#3720=EDGE_LOOP('',(#16630));
#3721=EDGE_LOOP('',(#16631));
#3722=EDGE_LOOP('',(#16632));
#3723=EDGE_LOOP('',(#16633));
#3724=EDGE_LOOP('',(#16634,#16635,#16636,#16637));
#3725=EDGE_LOOP('',(#16638,#16639,#16640,#16641));
#3726=EDGE_LOOP('',(#16642,#16643,#16644,#16645));
#3727=EDGE_LOOP('',(#16646));
#3728=EDGE_LOOP('',(#16647));
#3729=EDGE_LOOP('',(#16648));
#3730=EDGE_LOOP('',(#16649));
#3731=EDGE_LOOP('',(#16650,#16651,#16652,#16653));
#3732=EDGE_LOOP('',(#16654,#16655,#16656,#16657));
#3733=EDGE_LOOP('',(#16658,#16659,#16660,#16661));
#3734=EDGE_LOOP('',(#16662,#16663,#16664,#16665));
#3735=EDGE_LOOP('',(#16666,#16667,#16668,#16669));
#3736=EDGE_LOOP('',(#16670,#16671,#16672,#16673));
#3737=EDGE_LOOP('',(#16674,#16675,#16676,#16677));
#3738=EDGE_LOOP('',(#16678,#16679,#16680,#16681));
#3739=EDGE_LOOP('',(#16682,#16683,#16684,#16685));
#3740=EDGE_LOOP('',(#16686,#16687,#16688,#16689));
#3741=EDGE_LOOP('',(#16690,#16691,#16692,#16693));
#3742=EDGE_LOOP('',(#16694,#16695,#16696,#16697));
#3743=EDGE_LOOP('',(#16698,#16699,#16700,#16701));
#3744=EDGE_LOOP('',(#16702,#16703,#16704,#16705));
#3745=EDGE_LOOP('',(#16706,#16707,#16708,#16709));
#3746=EDGE_LOOP('',(#16710,#16711,#16712,#16713,#16714,#16715));
#3747=EDGE_LOOP('',(#16716,#16717,#16718,#16719,#16720,#16721));
#3748=EDGE_LOOP('',(#16722,#16723,#16724,#16725,#16726,#16727));
#3749=EDGE_LOOP('',(#16728,#16729,#16730,#16731,#16732,#16733));
#3750=EDGE_LOOP('',(#16734,#16735,#16736,#16737));
#3751=EDGE_LOOP('',(#16738,#16739,#16740,#16741));
#3752=EDGE_LOOP('',(#16742));
#3753=EDGE_LOOP('',(#16743));
#3754=EDGE_LOOP('',(#16744));
#3755=EDGE_LOOP('',(#16745));
#3756=EDGE_LOOP('',(#16746,#16747,#16748,#16749));
#3757=EDGE_LOOP('',(#16750,#16751,#16752,#16753));
#3758=EDGE_LOOP('',(#16754,#16755,#16756,#16757));
#3759=EDGE_LOOP('',(#16758,#16759,#16760,#16761));
#3760=EDGE_LOOP('',(#16762,#16763,#16764,#16765,#16766,#16767,#16768,#16769));
#3761=EDGE_LOOP('',(#16770));
#3762=EDGE_LOOP('',(#16771));
#3763=EDGE_LOOP('',(#16772));
#3764=EDGE_LOOP('',(#16773));
#3765=EDGE_LOOP('',(#16774,#16775,#16776,#16777));
#3766=EDGE_LOOP('',(#16778,#16779,#16780,#16781));
#3767=EDGE_LOOP('',(#16782,#16783,#16784,#16785));
#3768=EDGE_LOOP('',(#16786,#16787,#16788,#16789));
#3769=EDGE_LOOP('',(#16790,#16791,#16792,#16793));
#3770=EDGE_LOOP('',(#16794,#16795,#16796,#16797));
#3771=EDGE_LOOP('',(#16798,#16799,#16800,#16801));
#3772=EDGE_LOOP('',(#16802,#16803,#16804,#16805));
#3773=EDGE_LOOP('',(#16806,#16807,#16808,#16809));
#3774=EDGE_LOOP('',(#16810,#16811,#16812,#16813));
#3775=EDGE_LOOP('',(#16814,#16815,#16816,#16817));
#3776=EDGE_LOOP('',(#16818,#16819,#16820,#16821));
#3777=EDGE_LOOP('',(#16822,#16823,#16824,#16825));
#3778=EDGE_LOOP('',(#16826));
#3779=EDGE_LOOP('',(#16827));
#3780=EDGE_LOOP('',(#16828));
#3781=EDGE_LOOP('',(#16829));
#3782=EDGE_LOOP('',(#16830));
#3783=EDGE_LOOP('',(#16831));
#3784=EDGE_LOOP('',(#16832));
#3785=EDGE_LOOP('',(#16833));
#3786=EDGE_LOOP('',(#16834));
#3787=EDGE_LOOP('',(#16835,#16836,#16837,#16838));
#3788=EDGE_LOOP('',(#16839,#16840,#16841,#16842));
#3789=EDGE_LOOP('',(#16843,#16844,#16845,#16846));
#3790=EDGE_LOOP('',(#16847,#16848,#16849,#16850));
#3791=EDGE_LOOP('',(#16851,#16852,#16853,#16854));
#3792=EDGE_LOOP('',(#16855));
#3793=EDGE_LOOP('',(#16856));
#3794=EDGE_LOOP('',(#16857));
#3795=EDGE_LOOP('',(#16858));
#3796=EDGE_LOOP('',(#16859));
#3797=EDGE_LOOP('',(#16860));
#3798=EDGE_LOOP('',(#16861));
#3799=EDGE_LOOP('',(#16862));
#3800=EDGE_LOOP('',(#16863));
#3801=EDGE_LOOP('',(#16864));
#3802=EDGE_LOOP('',(#16865));
#3803=EDGE_LOOP('',(#16866));
#3804=EDGE_LOOP('',(#16867));
#3805=EDGE_LOOP('',(#16868));
#3806=EDGE_LOOP('',(#16869));
#3807=EDGE_LOOP('',(#16870,#16871,#16872,#16873));
#3808=EDGE_LOOP('',(#16874,#16875,#16876,#16877));
#3809=EDGE_LOOP('',(#16878,#16879,#16880,#16881));
#3810=EDGE_LOOP('',(#16882,#16883,#16884,#16885));
#3811=EDGE_LOOP('',(#16886,#16887,#16888,#16889));
#3812=EDGE_LOOP('',(#16890,#16891,#16892,#16893));
#3813=EDGE_LOOP('',(#16894,#16895,#16896,#16897));
#3814=EDGE_LOOP('',(#16898,#16899,#16900,#16901,#16902,#16903));
#3815=EDGE_LOOP('',(#16904));
#3816=EDGE_LOOP('',(#16905));
#3817=EDGE_LOOP('',(#16906));
#3818=EDGE_LOOP('',(#16907));
#3819=EDGE_LOOP('',(#16908));
#3820=EDGE_LOOP('',(#16909));
#3821=EDGE_LOOP('',(#16910));
#3822=EDGE_LOOP('',(#16911,#16912,#16913,#16914));
#3823=EDGE_LOOP('',(#16915,#16916,#16917,#16918,#16919,#16920));
#3824=EDGE_LOOP('',(#16921));
#3825=EDGE_LOOP('',(#16922));
#3826=EDGE_LOOP('',(#16923));
#3827=EDGE_LOOP('',(#16924));
#3828=EDGE_LOOP('',(#16925));
#3829=EDGE_LOOP('',(#16926));
#3830=EDGE_LOOP('',(#16927));
#3831=EDGE_LOOP('',(#16928,#16929,#16930,#16931));
#3832=EDGE_LOOP('',(#16932,#16933,#16934,#16935));
#3833=EDGE_LOOP('',(#16936,#16937,#16938,#16939));
#3834=EDGE_LOOP('',(#16940,#16941,#16942,#16943));
#3835=EDGE_LOOP('',(#16944,#16945,#16946,#16947));
#3836=EDGE_LOOP('',(#16948,#16949,#16950,#16951));
#3837=EDGE_LOOP('',(#16952,#16953,#16954,#16955));
#3838=EDGE_LOOP('',(#16956,#16957,#16958,#16959));
#3839=EDGE_LOOP('',(#16960,#16961,#16962,#16963));
#3840=EDGE_LOOP('',(#16964,#16965,#16966,#16967));
#3841=EDGE_LOOP('',(#16968,#16969,#16970,#16971));
#3842=EDGE_LOOP('',(#16972,#16973,#16974,#16975));
#3843=EDGE_LOOP('',(#16976,#16977,#16978,#16979));
#3844=EDGE_LOOP('',(#16980,#16981,#16982,#16983));
#3845=EDGE_LOOP('',(#16984,#16985,#16986,#16987));
#3846=EDGE_LOOP('',(#16988,#16989,#16990,#16991));
#3847=EDGE_LOOP('',(#16992));
#3848=EDGE_LOOP('',(#16993));
#3849=EDGE_LOOP('',(#16994));
#3850=EDGE_LOOP('',(#16995));
#3851=EDGE_LOOP('',(#16996));
#3852=EDGE_LOOP('',(#16997));
#3853=EDGE_LOOP('',(#16998,#16999,#17000,#17001));
#3854=EDGE_LOOP('',(#17002));
#3855=EDGE_LOOP('',(#17003));
#3856=EDGE_LOOP('',(#17004));
#3857=EDGE_LOOP('',(#17005));
#3858=EDGE_LOOP('',(#17006));
#3859=EDGE_LOOP('',(#17007));
#3860=EDGE_LOOP('',(#17008,#17009,#17010,#17011));
#3861=EDGE_LOOP('',(#17012,#17013,#17014,#17015));
#3862=EDGE_LOOP('',(#17016,#17017,#17018,#17019));
#3863=EDGE_LOOP('',(#17020,#17021,#17022,#17023));
#3864=EDGE_LOOP('',(#17024,#17025,#17026,#17027));
#3865=EDGE_LOOP('',(#17028,#17029,#17030,#17031));
#3866=EDGE_LOOP('',(#17032,#17033,#17034,#17035));
#3867=EDGE_LOOP('',(#17036,#17037,#17038,#17039));
#3868=EDGE_LOOP('',(#17040,#17041,#17042,#17043));
#3869=EDGE_LOOP('',(#17044,#17045,#17046,#17047));
#3870=EDGE_LOOP('',(#17048,#17049,#17050,#17051));
#3871=EDGE_LOOP('',(#17052));
#3872=EDGE_LOOP('',(#17053));
#3873=EDGE_LOOP('',(#17054));
#3874=EDGE_LOOP('',(#17055));
#3875=EDGE_LOOP('',(#17056));
#3876=EDGE_LOOP('',(#17057));
#3877=EDGE_LOOP('',(#17058,#17059,#17060,#17061));
#3878=EDGE_LOOP('',(#17062));
#3879=EDGE_LOOP('',(#17063));
#3880=EDGE_LOOP('',(#17064));
#3881=EDGE_LOOP('',(#17065));
#3882=EDGE_LOOP('',(#17066));
#3883=EDGE_LOOP('',(#17067));
#3884=EDGE_LOOP('',(#17068,#17069,#17070,#17071));
#3885=EDGE_LOOP('',(#17072,#17073,#17074,#17075,#17076,#17077,#17078,#17079,
#17080,#17081,#17082,#17083));
#3886=EDGE_LOOP('',(#17084,#17085,#17086,#17087));
#3887=EDGE_LOOP('',(#17088,#17089,#17090,#17091,#17092,#17093,#17094,#17095,
#17096,#17097,#17098,#17099));
#3888=EDGE_LOOP('',(#17100,#17101,#17102,#17103));
#3889=EDGE_LOOP('',(#17104,#17105,#17106,#17107,#17108,#17109,#17110,#17111,
#17112,#17113,#17114,#17115));
#3890=EDGE_LOOP('',(#17116,#17117,#17118,#17119));
#3891=EDGE_LOOP('',(#17120,#17121,#17122,#17123,#17124,#17125,#17126,#17127,
#17128,#17129,#17130,#17131));
#3892=EDGE_LOOP('',(#17132,#17133,#17134,#17135));
#3893=EDGE_LOOP('',(#17136,#17137,#17138,#17139,#17140,#17141,#17142,#17143,
#17144,#17145,#17146,#17147));
#3894=EDGE_LOOP('',(#17148,#17149,#17150,#17151));
#3895=EDGE_LOOP('',(#17152,#17153,#17154,#17155,#17156,#17157,#17158,#17159,
#17160,#17161,#17162,#17163));
#3896=EDGE_LOOP('',(#17164,#17165,#17166,#17167));
#3897=EDGE_LOOP('',(#17168,#17169,#17170,#17171,#17172,#17173,#17174,#17175,
#17176,#17177,#17178,#17179));
#3898=EDGE_LOOP('',(#17180,#17181,#17182,#17183));
#3899=EDGE_LOOP('',(#17184,#17185,#17186,#17187,#17188,#17189,#17190,#17191,
#17192,#17193,#17194,#17195));
#3900=EDGE_LOOP('',(#17196,#17197,#17198,#17199));
#3901=EDGE_LOOP('',(#17200,#17201,#17202,#17203,#17204,#17205,#17206,#17207,
#17208,#17209,#17210,#17211));
#3902=EDGE_LOOP('',(#17212,#17213,#17214,#17215));
#3903=EDGE_LOOP('',(#17216,#17217,#17218,#17219,#17220,#17221,#17222,#17223,
#17224,#17225,#17226,#17227));
#3904=EDGE_LOOP('',(#17228,#17229,#17230,#17231));
#3905=EDGE_LOOP('',(#17232,#17233,#17234,#17235,#17236,#17237,#17238,#17239,
#17240,#17241,#17242,#17243));
#3906=EDGE_LOOP('',(#17244,#17245,#17246,#17247));
#3907=EDGE_LOOP('',(#17248,#17249,#17250,#17251,#17252,#17253,#17254,#17255,
#17256,#17257,#17258,#17259));
#3908=EDGE_LOOP('',(#17260,#17261,#17262,#17263));
#3909=EDGE_LOOP('',(#17264,#17265,#17266,#17267,#17268,#17269,#17270,#17271,
#17272,#17273,#17274,#17275));
#3910=EDGE_LOOP('',(#17276,#17277,#17278,#17279));
#3911=EDGE_LOOP('',(#17280,#17281,#17282,#17283,#17284,#17285,#17286,#17287,
#17288,#17289,#17290,#17291));
#3912=EDGE_LOOP('',(#17292,#17293,#17294,#17295));
#3913=EDGE_LOOP('',(#17296,#17297,#17298,#17299,#17300,#17301,#17302,#17303,
#17304,#17305,#17306,#17307));
#3914=EDGE_LOOP('',(#17308,#17309,#17310,#17311));
#3915=EDGE_LOOP('',(#17312,#17313,#17314,#17315));
#3916=EDGE_LOOP('',(#17316,#17317,#17318,#17319,#17320,#17321,#17322,#17323,
#17324,#17325,#17326,#17327,#17328,#17329,#17330,#17331,#17332,#17333,#17334,
#17335,#17336,#17337,#17338,#17339,#17340,#17341,#17342,#17343,#17344,#17345,
#17346,#17347,#17348,#17349));
#3917=EDGE_LOOP('',(#17350,#17351,#17352,#17353,#17354));
#3918=EDGE_LOOP('',(#17355,#17356,#17357,#17358,#17359,#17360,#17361,#17362,
#17363,#17364,#17365,#17366,#17367,#17368,#17369,#17370,#17371,#17372,#17373,
#17374,#17375,#17376,#17377,#17378,#17379,#17380,#17381,#17382,#17383,#17384,
#17385,#17386,#17387,#17388));
#3919=EDGE_LOOP('',(#17389,#17390,#17391,#17392));
#3920=EDGE_LOOP('',(#17393,#17394,#17395,#17396,#17397));
#3921=EDGE_LOOP('',(#17398,#17399,#17400,#17401));
#3922=EDGE_LOOP('',(#17402,#17403,#17404,#17405));
#3923=EDGE_LOOP('',(#17406,#17407,#17408,#17409,#17410));
#3924=EDGE_LOOP('',(#17411,#17412,#17413,#17414));
#3925=EDGE_LOOP('',(#17415,#17416,#17417,#17418));
#3926=EDGE_LOOP('',(#17419,#17420,#17421,#17422,#17423));
#3927=EDGE_LOOP('',(#17424,#17425,#17426,#17427));
#3928=EDGE_LOOP('',(#17428,#17429,#17430,#17431));
#3929=EDGE_LOOP('',(#17432,#17433,#17434,#17435,#17436));
#3930=EDGE_LOOP('',(#17437,#17438,#17439,#17440));
#3931=EDGE_LOOP('',(#17441,#17442,#17443,#17444));
#3932=EDGE_LOOP('',(#17445,#17446,#17447,#17448,#17449));
#3933=EDGE_LOOP('',(#17450,#17451,#17452,#17453));
#3934=EDGE_LOOP('',(#17454,#17455,#17456,#17457));
#3935=EDGE_LOOP('',(#17458,#17459,#17460,#17461,#17462));
#3936=EDGE_LOOP('',(#17463,#17464,#17465,#17466));
#3937=EDGE_LOOP('',(#17467,#17468,#17469,#17470));
#3938=EDGE_LOOP('',(#17471,#17472,#17473,#17474,#17475));
#3939=EDGE_LOOP('',(#17476,#17477,#17478,#17479));
#3940=EDGE_LOOP('',(#17480,#17481,#17482,#17483));
#3941=EDGE_LOOP('',(#17484,#17485,#17486,#17487,#17488));
#3942=EDGE_LOOP('',(#17489,#17490,#17491,#17492));
#3943=EDGE_LOOP('',(#17493,#17494,#17495,#17496));
#3944=EDGE_LOOP('',(#17497,#17498,#17499,#17500,#17501));
#3945=EDGE_LOOP('',(#17502,#17503,#17504,#17505));
#3946=EDGE_LOOP('',(#17506,#17507,#17508,#17509,#17510));
#3947=EDGE_LOOP('',(#17511,#17512,#17513,#17514));
#3948=EDGE_LOOP('',(#17515,#17516,#17517,#17518));
#3949=EDGE_LOOP('',(#17519,#17520,#17521,#17522));
#3950=EDGE_LOOP('',(#17523,#17524,#17525,#17526,#17527));
#3951=EDGE_LOOP('',(#17528,#17529,#17530,#17531));
#3952=EDGE_LOOP('',(#17532,#17533,#17534,#17535));
#3953=EDGE_LOOP('',(#17536,#17537,#17538,#17539,#17540));
#3954=EDGE_LOOP('',(#17541,#17542,#17543,#17544));
#3955=EDGE_LOOP('',(#17545,#17546,#17547,#17548,#17549));
#3956=EDGE_LOOP('',(#17550,#17551,#17552,#17553));
#3957=EDGE_LOOP('',(#17554,#17555,#17556,#17557));
#3958=EDGE_LOOP('',(#17558,#17559,#17560,#17561));
#3959=EDGE_LOOP('',(#17562,#17563,#17564,#17565));
#3960=EDGE_LOOP('',(#17566,#17567,#17568,#17569));
#3961=EDGE_LOOP('',(#17570,#17571,#17572,#17573,#17574,#17575,#17576,#17577,
#17578,#17579,#17580,#17581,#17582,#17583,#17584,#17585,#17586,#17587,#17588,
#17589,#17590,#17591,#17592,#17593,#17594,#17595,#17596,#17597,#17598,#17599,
#17600,#17601,#17602,#17603,#17604,#17605,#17606,#17607,#17608,#17609,#17610,
#17611,#17612,#17613,#17614,#17615));
#3962=EDGE_LOOP('',(#17616,#17617,#17618,#17619,#17620,#17621,#17622,#17623,
#17624,#17625,#17626,#17627,#17628,#17629,#17630,#17631,#17632,#17633,#17634,
#17635,#17636,#17637,#17638,#17639,#17640,#17641,#17642,#17643,#17644,#17645,
#17646,#17647,#17648,#17649,#17650,#17651,#17652,#17653,#17654,#17655,#17656,
#17657,#17658,#17659,#17660,#17661));
#3963=EDGE_LOOP('',(#17662,#17663,#17664,#17665));
#3964=EDGE_LOOP('',(#17666,#17667,#17668,#17669));
#3965=EDGE_LOOP('',(#17670,#17671,#17672,#17673));
#3966=EDGE_LOOP('',(#17674,#17675,#17676,#17677));
#3967=EDGE_LOOP('',(#17678,#17679,#17680,#17681));
#3968=EDGE_LOOP('',(#17682,#17683,#17684,#17685));
#3969=EDGE_LOOP('',(#17686,#17687,#17688,#17689));
#3970=EDGE_LOOP('',(#17690));
#3971=EDGE_LOOP('',(#17691));
#3972=EDGE_LOOP('',(#17692));
#3973=EDGE_LOOP('',(#17693));
#3974=EDGE_LOOP('',(#17694));
#3975=EDGE_LOOP('',(#17695));
#3976=EDGE_LOOP('',(#17696));
#3977=EDGE_LOOP('',(#17697));
#3978=EDGE_LOOP('',(#17698));
#3979=EDGE_LOOP('',(#17699));
#3980=EDGE_LOOP('',(#17700));
#3981=EDGE_LOOP('',(#17701));
#3982=EDGE_LOOP('',(#17702));
#3983=EDGE_LOOP('',(#17703));
#3984=EDGE_LOOP('',(#17704));
#3985=EDGE_LOOP('',(#17705,#17706,#17707,#17708));
#3986=EDGE_LOOP('',(#17709,#17710,#17711,#17712));
#3987=EDGE_LOOP('',(#17713,#17714,#17715,#17716));
#3988=EDGE_LOOP('',(#17717,#17718,#17719,#17720));
#3989=EDGE_LOOP('',(#17721,#17722,#17723,#17724));
#3990=EDGE_LOOP('',(#17725,#17726,#17727,#17728));
#3991=EDGE_LOOP('',(#17729,#17730,#17731,#17732));
#3992=EDGE_LOOP('',(#17733,#17734,#17735,#17736));
#3993=EDGE_LOOP('',(#17737,#17738,#17739,#17740));
#3994=EDGE_LOOP('',(#17741,#17742,#17743,#17744));
#3995=EDGE_LOOP('',(#17745,#17746,#17747,#17748));
#3996=EDGE_LOOP('',(#17749,#17750,#17751,#17752));
#3997=EDGE_LOOP('',(#17753,#17754,#17755,#17756));
#3998=EDGE_LOOP('',(#17757,#17758,#17759,#17760));
#3999=EDGE_LOOP('',(#17761,#17762,#17763,#17764));
#4000=EDGE_LOOP('',(#17765,#17766,#17767,#17768));
#4001=EDGE_LOOP('',(#17769,#17770,#17771,#17772));
#4002=EDGE_LOOP('',(#17773,#17774,#17775,#17776));
#4003=EDGE_LOOP('',(#17777,#17778,#17779,#17780));
#4004=EDGE_LOOP('',(#17781,#17782,#17783,#17784));
#4005=EDGE_LOOP('',(#17785,#17786,#17787,#17788));
#4006=EDGE_LOOP('',(#17789,#17790,#17791,#17792));
#4007=EDGE_LOOP('',(#17793,#17794,#17795,#17796));
#4008=EDGE_LOOP('',(#17797,#17798,#17799,#17800));
#4009=EDGE_LOOP('',(#17801,#17802,#17803,#17804));
#4010=EDGE_LOOP('',(#17805,#17806,#17807,#17808));
#4011=EDGE_LOOP('',(#17809,#17810,#17811,#17812));
#4012=EDGE_LOOP('',(#17813,#17814,#17815,#17816));
#4013=EDGE_LOOP('',(#17817,#17818,#17819,#17820));
#4014=EDGE_LOOP('',(#17821,#17822,#17823,#17824));
#4015=EDGE_LOOP('',(#17825,#17826,#17827,#17828));
#4016=EDGE_LOOP('',(#17829,#17830,#17831,#17832));
#4017=EDGE_LOOP('',(#17833,#17834,#17835,#17836));
#4018=EDGE_LOOP('',(#17837,#17838,#17839,#17840));
#4019=EDGE_LOOP('',(#17841,#17842,#17843,#17844));
#4020=EDGE_LOOP('',(#17845,#17846,#17847,#17848,#17849));
#4021=EDGE_LOOP('',(#17850,#17851,#17852,#17853));
#4022=EDGE_LOOP('',(#17854));
#4023=EDGE_LOOP('',(#17855));
#4024=EDGE_LOOP('',(#17856));
#4025=EDGE_LOOP('',(#17857));
#4026=EDGE_LOOP('',(#17858));
#4027=EDGE_LOOP('',(#17859));
#4028=EDGE_LOOP('',(#17860));
#4029=EDGE_LOOP('',(#17861));
#4030=EDGE_LOOP('',(#17862));
#4031=EDGE_LOOP('',(#17863));
#4032=EDGE_LOOP('',(#17864));
#4033=EDGE_LOOP('',(#17865));
#4034=EDGE_LOOP('',(#17866));
#4035=EDGE_LOOP('',(#17867));
#4036=EDGE_LOOP('',(#17868));
#4037=EDGE_LOOP('',(#17869));
#4038=EDGE_LOOP('',(#17870));
#4039=EDGE_LOOP('',(#17871));
#4040=EDGE_LOOP('',(#17872));
#4041=EDGE_LOOP('',(#17873));
#4042=EDGE_LOOP('',(#17874));
#4043=EDGE_LOOP('',(#17875));
#4044=EDGE_LOOP('',(#17876));
#4045=EDGE_LOOP('',(#17877));
#4046=EDGE_LOOP('',(#17878));
#4047=EDGE_LOOP('',(#17879));
#4048=EDGE_LOOP('',(#17880));
#4049=EDGE_LOOP('',(#17881));
#4050=EDGE_LOOP('',(#17882));
#4051=EDGE_LOOP('',(#17883));
#4052=EDGE_LOOP('',(#17884,#17885,#17886,#17887));
#4053=EDGE_LOOP('',(#17888,#17889,#17890,#17891));
#4054=EDGE_LOOP('',(#17892,#17893,#17894,#17895));
#4055=EDGE_LOOP('',(#17896,#17897,#17898));
#4056=EDGE_LOOP('',(#17899,#17900,#17901));
#4057=EDGE_LOOP('',(#17902,#17903,#17904,#17905));
#4058=EDGE_LOOP('',(#17906,#17907,#17908,#17909));
#4059=EDGE_LOOP('',(#17910,#17911,#17912,#17913));
#4060=EDGE_LOOP('',(#17914,#17915,#17916,#17917));
#4061=EDGE_LOOP('',(#17918,#17919,#17920,#17921));
#4062=EDGE_LOOP('',(#17922,#17923,#17924,#17925));
#4063=EDGE_LOOP('',(#17926,#17927,#17928,#17929));
#4064=EDGE_LOOP('',(#17930,#17931,#17932,#17933,#17934,#17935,#17936));
#4065=EDGE_LOOP('',(#17937,#17938,#17939));
#4066=EDGE_LOOP('',(#17940,#17941,#17942));
#4067=EDGE_LOOP('',(#17943,#17944,#17945,#17946,#17947,#17948,#17949));
#4068=EDGE_LOOP('',(#17950,#17951,#17952,#17953,#17954,#17955,#17956,#17957,
#17958,#17959));
#4069=EDGE_LOOP('',(#17960,#17961,#17962,#17963,#17964));
#4070=EDGE_LOOP('',(#17965,#17966,#17967,#17968));
#4071=EDGE_LOOP('',(#17969,#17970,#17971,#17972));
#4072=EDGE_LOOP('',(#17973,#17974,#17975,#17976));
#4073=EDGE_LOOP('',(#17977,#17978,#17979,#17980));
#4074=EDGE_LOOP('',(#17981,#17982,#17983,#17984));
#4075=EDGE_LOOP('',(#17985,#17986,#17987,#17988));
#4076=EDGE_LOOP('',(#17989,#17990,#17991,#17992));
#4077=EDGE_LOOP('',(#17993,#17994,#17995,#17996));
#4078=EDGE_LOOP('',(#17997,#17998,#17999,#18000));
#4079=EDGE_LOOP('',(#18001,#18002,#18003,#18004));
#4080=EDGE_LOOP('',(#18005,#18006,#18007,#18008));
#4081=EDGE_LOOP('',(#18009,#18010,#18011,#18012));
#4082=EDGE_LOOP('',(#18013,#18014,#18015,#18016));
#4083=EDGE_LOOP('',(#18017,#18018,#18019,#18020));
#4084=EDGE_LOOP('',(#18021,#18022,#18023,#18024));
#4085=EDGE_LOOP('',(#18025,#18026,#18027,#18028));
#4086=EDGE_LOOP('',(#18029,#18030,#18031,#18032));
#4087=EDGE_LOOP('',(#18033,#18034,#18035,#18036));
#4088=EDGE_LOOP('',(#18037,#18038,#18039,#18040));
#4089=EDGE_LOOP('',(#18041,#18042,#18043,#18044));
#4090=EDGE_LOOP('',(#18045,#18046,#18047,#18048));
#4091=EDGE_LOOP('',(#18049,#18050,#18051,#18052));
#4092=EDGE_LOOP('',(#18053,#18054,#18055,#18056));
#4093=EDGE_LOOP('',(#18057,#18058,#18059,#18060));
#4094=EDGE_LOOP('',(#18061,#18062,#18063,#18064));
#4095=EDGE_LOOP('',(#18065,#18066,#18067,#18068));
#4096=EDGE_LOOP('',(#18069,#18070,#18071,#18072));
#4097=EDGE_LOOP('',(#18073,#18074,#18075,#18076));
#4098=EDGE_LOOP('',(#18077,#18078,#18079,#18080));
#4099=EDGE_LOOP('',(#18081,#18082,#18083,#18084));
#4100=EDGE_LOOP('',(#18085,#18086,#18087,#18088));
#4101=EDGE_LOOP('',(#18089,#18090,#18091,#18092));
#4102=EDGE_LOOP('',(#18093,#18094,#18095,#18096));
#4103=EDGE_LOOP('',(#18097,#18098,#18099,#18100));
#4104=EDGE_LOOP('',(#18101,#18102,#18103,#18104));
#4105=EDGE_LOOP('',(#18105,#18106,#18107,#18108));
#4106=EDGE_LOOP('',(#18109,#18110,#18111,#18112));
#4107=EDGE_LOOP('',(#18113,#18114,#18115,#18116));
#4108=EDGE_LOOP('',(#18117,#18118,#18119,#18120));
#4109=EDGE_LOOP('',(#18121,#18122,#18123,#18124));
#4110=EDGE_LOOP('',(#18125,#18126,#18127,#18128));
#4111=EDGE_LOOP('',(#18129,#18130,#18131,#18132));
#4112=EDGE_LOOP('',(#18133));
#4113=EDGE_LOOP('',(#18134));
#4114=EDGE_LOOP('',(#18135,#18136,#18137,#18138));
#4115=EDGE_LOOP('',(#18139,#18140,#18141,#18142,#18143,#18144,#18145,#18146,
#18147,#18148,#18149,#18150,#18151,#18152,#18153,#18154,#18155,#18156,#18157,
#18158,#18159,#18160,#18161,#18162,#18163,#18164,#18165,#18166,#18167,#18168,
#18169,#18170,#18171,#18172,#18173,#18174,#18175,#18176,#18177,#18178,#18179,
#18180,#18181,#18182));
#4116=EDGE_LOOP('',(#18183));
#4117=EDGE_LOOP('',(#18184,#18185,#18186,#18187));
#4118=EDGE_LOOP('',(#18188,#18189,#18190,#18191));
#4119=EDGE_LOOP('',(#18192,#18193,#18194,#18195));
#4120=EDGE_LOOP('',(#18196,#18197,#18198,#18199));
#4121=EDGE_LOOP('',(#18200,#18201,#18202,#18203));
#4122=EDGE_LOOP('',(#18204,#18205,#18206,#18207));
#4123=EDGE_LOOP('',(#18208,#18209,#18210,#18211));
#4124=EDGE_LOOP('',(#18212,#18213,#18214,#18215));
#4125=EDGE_LOOP('',(#18216,#18217,#18218,#18219));
#4126=EDGE_LOOP('',(#18220,#18221,#18222,#18223));
#4127=EDGE_LOOP('',(#18224,#18225,#18226,#18227));
#4128=EDGE_LOOP('',(#18228,#18229,#18230,#18231));
#4129=EDGE_LOOP('',(#18232,#18233,#18234,#18235,#18236,#18237));
#4130=EDGE_LOOP('',(#18238,#18239,#18240,#18241,#18242,#18243,#18244,#18245,
#18246,#18247,#18248,#18249,#18250,#18251,#18252,#18253,#18254,#18255,#18256,
#18257,#18258,#18259,#18260,#18261,#18262,#18263,#18264,#18265,#18266,#18267,
#18268,#18269,#18270,#18271,#18272,#18273,#18274,#18275,#18276,#18277,#18278,
#18279,#18280,#18281));
#4131=EDGE_LOOP('',(#18282,#18283,#18284,#18285,#18286,#18287,#18288,#18289,
#18290,#18291,#18292,#18293,#18294,#18295,#18296,#18297,#18298,#18299,#18300,
#18301,#18302,#18303,#18304,#18305,#18306,#18307,#18308,#18309,#18310,#18311,
#18312,#18313,#18314,#18315,#18316,#18317,#18318,#18319,#18320,#18321,#18322,
#18323,#18324,#18325));
#4132=EDGE_LOOP('',(#18326,#18327,#18328,#18329));
#4133=EDGE_LOOP('',(#18330,#18331,#18332,#18333));
#4134=EDGE_LOOP('',(#18334,#18335,#18336,#18337));
#4135=EDGE_LOOP('',(#18338,#18339,#18340,#18341));
#4136=EDGE_LOOP('',(#18342,#18343,#18344,#18345));
#4137=EDGE_LOOP('',(#18346,#18347,#18348,#18349));
#4138=EDGE_LOOP('',(#18350,#18351,#18352,#18353));
#4139=EDGE_LOOP('',(#18354,#18355,#18356,#18357));
#4140=EDGE_LOOP('',(#18358,#18359,#18360,#18361));
#4141=EDGE_LOOP('',(#18362,#18363,#18364,#18365));
#4142=EDGE_LOOP('',(#18366,#18367,#18368,#18369));
#4143=EDGE_LOOP('',(#18370,#18371,#18372,#18373));
#4144=EDGE_LOOP('',(#18374,#18375,#18376,#18377));
#4145=EDGE_LOOP('',(#18378,#18379,#18380,#18381));
#4146=EDGE_LOOP('',(#18382,#18383,#18384,#18385));
#4147=EDGE_LOOP('',(#18386,#18387,#18388,#18389));
#4148=EDGE_LOOP('',(#18390,#18391,#18392,#18393));
#4149=EDGE_LOOP('',(#18394,#18395,#18396,#18397));
#4150=EDGE_LOOP('',(#18398,#18399,#18400,#18401));
#4151=EDGE_LOOP('',(#18402,#18403,#18404,#18405));
#4152=EDGE_LOOP('',(#18406,#18407,#18408,#18409));
#4153=EDGE_LOOP('',(#18410,#18411,#18412,#18413));
#4154=EDGE_LOOP('',(#18414,#18415,#18416,#18417));
#4155=EDGE_LOOP('',(#18418,#18419,#18420,#18421));
#4156=EDGE_LOOP('',(#18422,#18423,#18424,#18425));
#4157=EDGE_LOOP('',(#18426,#18427,#18428,#18429));
#4158=EDGE_LOOP('',(#18430,#18431,#18432,#18433));
#4159=EDGE_LOOP('',(#18434,#18435,#18436,#18437));
#4160=EDGE_LOOP('',(#18438,#18439,#18440,#18441));
#4161=EDGE_LOOP('',(#18442,#18443,#18444,#18445));
#4162=EDGE_LOOP('',(#18446,#18447,#18448,#18449));
#4163=EDGE_LOOP('',(#18450,#18451,#18452,#18453));
#4164=EDGE_LOOP('',(#18454,#18455,#18456,#18457));
#4165=EDGE_LOOP('',(#18458,#18459,#18460,#18461));
#4166=EDGE_LOOP('',(#18462,#18463,#18464,#18465));
#4167=EDGE_LOOP('',(#18466,#18467,#18468,#18469));
#4168=EDGE_LOOP('',(#18470,#18471,#18472,#18473));
#4169=EDGE_LOOP('',(#18474,#18475,#18476,#18477));
#4170=EDGE_LOOP('',(#18478,#18479,#18480,#18481));
#4171=EDGE_LOOP('',(#18482,#18483,#18484,#18485));
#4172=EDGE_LOOP('',(#18486,#18487,#18488,#18489));
#4173=EDGE_LOOP('',(#18490,#18491,#18492,#18493));
#4174=EDGE_LOOP('',(#18494,#18495,#18496,#18497));
#4175=EDGE_LOOP('',(#18498,#18499,#18500,#18501));
#4176=EDGE_LOOP('',(#18502));
#4177=EDGE_LOOP('',(#18503,#18504,#18505,#18506));
#4178=EDGE_LOOP('',(#18507,#18508,#18509,#18510,#18511,#18512,#18513,#18514,
#18515,#18516,#18517,#18518,#18519,#18520,#18521,#18522,#18523,#18524,#18525,
#18526,#18527,#18528,#18529,#18530,#18531,#18532,#18533,#18534,#18535,#18536,
#18537,#18538,#18539,#18540,#18541,#18542,#18543,#18544,#18545,#18546,#18547,
#18548,#18549,#18550,#18551,#18552,#18553,#18554));
#4179=EDGE_LOOP('',(#18555,#18556,#18557,#18558));
#4180=EDGE_LOOP('',(#18559,#18560,#18561,#18562));
#4181=EDGE_LOOP('',(#18563,#18564,#18565,#18566));
#4182=EDGE_LOOP('',(#18567));
#4183=EDGE_LOOP('',(#18568,#18569,#18570,#18571));
#4184=EDGE_LOOP('',(#18572,#18573,#18574,#18575));
#4185=EDGE_LOOP('',(#18576,#18577,#18578,#18579));
#4186=EDGE_LOOP('',(#18580,#18581,#18582,#18583));
#4187=EDGE_LOOP('',(#18584,#18585,#18586,#18587));
#4188=EDGE_LOOP('',(#18588,#18589,#18590,#18591,#18592,#18593,#18594,#18595));
#4189=EDGE_LOOP('',(#18596,#18597,#18598,#18599));
#4190=EDGE_LOOP('',(#18600,#18601,#18602,#18603));
#4191=EDGE_LOOP('',(#18604,#18605,#18606,#18607));
#4192=EDGE_LOOP('',(#18608,#18609,#18610,#18611));
#4193=EDGE_LOOP('',(#18612,#18613,#18614,#18615));
#4194=EDGE_LOOP('',(#18616,#18617,#18618,#18619));
#4195=EDGE_LOOP('',(#18620,#18621,#18622,#18623));
#4196=EDGE_LOOP('',(#18624,#18625,#18626,#18627));
#4197=EDGE_LOOP('',(#18628,#18629,#18630,#18631));
#4198=EDGE_LOOP('',(#18632,#18633,#18634,#18635));
#4199=EDGE_LOOP('',(#18636,#18637,#18638,#18639));
#4200=EDGE_LOOP('',(#18640,#18641,#18642,#18643));
#4201=EDGE_LOOP('',(#18644,#18645,#18646,#18647));
#4202=EDGE_LOOP('',(#18648,#18649,#18650,#18651));
#4203=EDGE_LOOP('',(#18652,#18653,#18654,#18655));
#4204=EDGE_LOOP('',(#18656,#18657,#18658,#18659));
#4205=EDGE_LOOP('',(#18660,#18661,#18662,#18663));
#4206=EDGE_LOOP('',(#18664,#18665,#18666,#18667));
#4207=EDGE_LOOP('',(#18668,#18669,#18670,#18671));
#4208=EDGE_LOOP('',(#18672,#18673,#18674,#18675));
#4209=EDGE_LOOP('',(#18676,#18677,#18678,#18679));
#4210=EDGE_LOOP('',(#18680,#18681,#18682,#18683));
#4211=EDGE_LOOP('',(#18684,#18685,#18686,#18687));
#4212=EDGE_LOOP('',(#18688,#18689,#18690,#18691));
#4213=EDGE_LOOP('',(#18692,#18693,#18694,#18695));
#4214=EDGE_LOOP('',(#18696,#18697,#18698,#18699));
#4215=EDGE_LOOP('',(#18700,#18701,#18702,#18703));
#4216=EDGE_LOOP('',(#18704,#18705,#18706,#18707));
#4217=EDGE_LOOP('',(#18708,#18709,#18710,#18711));
#4218=EDGE_LOOP('',(#18712,#18713,#18714,#18715));
#4219=EDGE_LOOP('',(#18716,#18717,#18718,#18719));
#4220=EDGE_LOOP('',(#18720,#18721,#18722,#18723));
#4221=EDGE_LOOP('',(#18724,#18725,#18726,#18727));
#4222=EDGE_LOOP('',(#18728,#18729,#18730,#18731));
#4223=EDGE_LOOP('',(#18732,#18733,#18734,#18735));
#4224=EDGE_LOOP('',(#18736,#18737,#18738,#18739));
#4225=EDGE_LOOP('',(#18740,#18741,#18742,#18743));
#4226=EDGE_LOOP('',(#18744,#18745,#18746,#18747));
#4227=EDGE_LOOP('',(#18748,#18749,#18750,#18751));
#4228=EDGE_LOOP('',(#18752));
#4229=EDGE_LOOP('',(#18753,#18754,#18755,#18756));
#4230=EDGE_LOOP('',(#18757,#18758,#18759,#18760));
#4231=EDGE_LOOP('',(#18761,#18762,#18763,#18764));
#4232=EDGE_LOOP('',(#18765,#18766,#18767,#18768));
#4233=EDGE_LOOP('',(#18769,#18770,#18771,#18772));
#4234=EDGE_LOOP('',(#18773,#18774,#18775,#18776));
#4235=EDGE_LOOP('',(#18777,#18778,#18779,#18780));
#4236=EDGE_LOOP('',(#18781,#18782,#18783,#18784,#18785,#18786));
#4237=EDGE_LOOP('',(#18787,#18788,#18789,#18790));
#4238=EDGE_LOOP('',(#18791,#18792,#18793,#18794));
#4239=EDGE_LOOP('',(#18795,#18796,#18797,#18798,#18799,#18800));
#4240=EDGE_LOOP('',(#18801,#18802,#18803,#18804));
#4241=EDGE_LOOP('',(#18805,#18806,#18807,#18808,#18809,#18810,#18811,#18812,
#18813,#18814,#18815,#18816,#18817,#18818,#18819,#18820,#18821,#18822,#18823,
#18824,#18825,#18826,#18827,#18828,#18829,#18830,#18831,#18832,#18833,#18834,
#18835,#18836,#18837,#18838,#18839,#18840,#18841,#18842,#18843,#18844,#18845,
#18846,#18847,#18848));
#4242=EDGE_LOOP('',(#18849,#18850,#18851,#18852,#18853,#18854,#18855,#18856,
#18857,#18858,#18859,#18860,#18861,#18862,#18863,#18864,#18865,#18866,#18867,
#18868,#18869,#18870,#18871,#18872,#18873,#18874,#18875,#18876,#18877,#18878,
#18879,#18880,#18881,#18882,#18883,#18884,#18885,#18886,#18887,#18888,#18889,
#18890,#18891,#18892));
#4243=EDGE_LOOP('',(#18893,#18894,#18895,#18896));
#4244=EDGE_LOOP('',(#18897,#18898,#18899,#18900));
#4245=EDGE_LOOP('',(#18901,#18902,#18903,#18904,#18905,#18906));
#4246=EDGE_LOOP('',(#18907,#18908,#18909,#18910));
#4247=EDGE_LOOP('',(#18911,#18912,#18913,#18914,#18915,#18916));
#4248=EDGE_LOOP('',(#18917,#18918,#18919,#18920));
#4249=EDGE_LOOP('',(#18921));
#4250=EDGE_LOOP('',(#18922,#18923,#18924,#18925));
#4251=EDGE_LOOP('',(#18926,#18927,#18928,#18929,#18930,#18931,#18932,#18933));
#4252=EDGE_LOOP('',(#18934,#18935,#18936,#18937,#18938,#18939));
#4253=EDGE_LOOP('',(#18940));
#4254=EDGE_LOOP('',(#18941,#18942,#18943,#18944));
#4255=EDGE_LOOP('',(#18945,#18946,#18947,#18948));
#4256=EDGE_LOOP('',(#18949,#18950,#18951,#18952));
#4257=EDGE_LOOP('',(#18953,#18954,#18955,#18956,#18957,#18958));
#4258=EDGE_LOOP('',(#18959));
#4259=EDGE_LOOP('',(#18960,#18961,#18962,#18963));
#4260=EDGE_LOOP('',(#18964,#18965,#18966,#18967,#18968,#18969,#18970,#18971));
#4261=EDGE_LOOP('',(#18972,#18973,#18974,#18975));
#4262=EDGE_LOOP('',(#18976,#18977,#18978,#18979));
#4263=EDGE_LOOP('',(#18980,#18981,#18982,#18983));
#4264=EDGE_LOOP('',(#18984,#18985,#18986,#18987));
#4265=EDGE_LOOP('',(#18988,#18989,#18990,#18991));
#4266=EDGE_LOOP('',(#18992,#18993,#18994,#18995));
#4267=EDGE_LOOP('',(#18996,#18997,#18998,#18999));
#4268=EDGE_LOOP('',(#19000,#19001,#19002,#19003));
#4269=EDGE_LOOP('',(#19004,#19005,#19006,#19007));
#4270=EDGE_LOOP('',(#19008,#19009,#19010,#19011));
#4271=EDGE_LOOP('',(#19012,#19013,#19014,#19015));
#4272=EDGE_LOOP('',(#19016,#19017,#19018,#19019));
#4273=EDGE_LOOP('',(#19020,#19021,#19022,#19023));
#4274=EDGE_LOOP('',(#19024,#19025,#19026,#19027));
#4275=EDGE_LOOP('',(#19028,#19029,#19030,#19031));
#4276=EDGE_LOOP('',(#19032,#19033,#19034,#19035));
#4277=EDGE_LOOP('',(#19036,#19037,#19038,#19039));
#4278=EDGE_LOOP('',(#19040,#19041,#19042,#19043));
#4279=EDGE_LOOP('',(#19044,#19045,#19046,#19047));
#4280=EDGE_LOOP('',(#19048,#19049,#19050,#19051));
#4281=EDGE_LOOP('',(#19052,#19053,#19054,#19055));
#4282=EDGE_LOOP('',(#19056,#19057,#19058,#19059));
#4283=EDGE_LOOP('',(#19060,#19061,#19062,#19063));
#4284=EDGE_LOOP('',(#19064,#19065,#19066,#19067));
#4285=EDGE_LOOP('',(#19068,#19069,#19070,#19071));
#4286=EDGE_LOOP('',(#19072,#19073,#19074,#19075));
#4287=EDGE_LOOP('',(#19076,#19077,#19078,#19079));
#4288=EDGE_LOOP('',(#19080,#19081,#19082,#19083));
#4289=EDGE_LOOP('',(#19084,#19085,#19086,#19087));
#4290=EDGE_LOOP('',(#19088,#19089,#19090,#19091));
#4291=EDGE_LOOP('',(#19092,#19093,#19094,#19095));
#4292=EDGE_LOOP('',(#19096,#19097,#19098,#19099));
#4293=EDGE_LOOP('',(#19100,#19101,#19102,#19103));
#4294=EDGE_LOOP('',(#19104,#19105,#19106,#19107));
#4295=EDGE_LOOP('',(#19108,#19109,#19110,#19111));
#4296=EDGE_LOOP('',(#19112,#19113,#19114,#19115));
#4297=EDGE_LOOP('',(#19116,#19117,#19118,#19119));
#4298=EDGE_LOOP('',(#19120,#19121,#19122,#19123));
#4299=EDGE_LOOP('',(#19124,#19125,#19126,#19127));
#4300=EDGE_LOOP('',(#19128,#19129,#19130,#19131));
#4301=EDGE_LOOP('',(#19132,#19133,#19134,#19135));
#4302=EDGE_LOOP('',(#19136,#19137,#19138,#19139));
#4303=EDGE_LOOP('',(#19140,#19141,#19142,#19143));
#4304=EDGE_LOOP('',(#19144,#19145,#19146,#19147));
#4305=EDGE_LOOP('',(#19148,#19149,#19150,#19151));
#4306=EDGE_LOOP('',(#19152));
#4307=EDGE_LOOP('',(#19153,#19154,#19155,#19156));
#4308=EDGE_LOOP('',(#19157,#19158,#19159,#19160));
#4309=EDGE_LOOP('',(#19161,#19162,#19163,#19164));
#4310=EDGE_LOOP('',(#19165,#19166,#19167,#19168));
#4311=EDGE_LOOP('',(#19169));
#4312=EDGE_LOOP('',(#19170,#19171,#19172,#19173));
#4313=EDGE_LOOP('',(#19174));
#4314=EDGE_LOOP('',(#19175,#19176,#19177,#19178));
#4315=EDGE_LOOP('',(#19179,#19180,#19181,#19182));
#4316=EDGE_LOOP('',(#19183,#19184,#19185,#19186));
#4317=EDGE_LOOP('',(#19187,#19188,#19189,#19190,#19191,#19192));
#4318=EDGE_LOOP('',(#19193,#19194,#19195,#19196));
#4319=EDGE_LOOP('',(#19197,#19198,#19199,#19200));
#4320=EDGE_LOOP('',(#19201));
#4321=EDGE_LOOP('',(#19202));
#4322=EDGE_LOOP('',(#19203,#19204,#19205,#19206));
#4323=EDGE_LOOP('',(#19207,#19208,#19209,#19210));
#4324=EDGE_LOOP('',(#19211,#19212,#19213,#19214));
#4325=EDGE_LOOP('',(#19215,#19216,#19217,#19218));
#4326=EDGE_LOOP('',(#19219,#19220,#19221,#19222));
#4327=EDGE_LOOP('',(#19223,#19224,#19225,#19226));
#4328=EDGE_LOOP('',(#19227,#19228,#19229,#19230));
#4329=EDGE_LOOP('',(#19231,#19232,#19233,#19234));
#4330=EDGE_LOOP('',(#19235));
#4331=EDGE_LOOP('',(#19236));
#4332=EDGE_LOOP('',(#19237,#19238,#19239,#19240));
#4333=EDGE_LOOP('',(#19241,#19242,#19243,#19244));
#4334=EDGE_LOOP('',(#19245,#19246,#19247,#19248));
#4335=EDGE_LOOP('',(#19249,#19250,#19251,#19252,#19253,#19254));
#4336=EDGE_LOOP('',(#19255,#19256,#19257,#19258,#19259,#19260));
#4337=EDGE_LOOP('',(#19261));
#4338=EDGE_LOOP('',(#19262,#19263,#19264,#19265));
#4339=EDGE_LOOP('',(#19266,#19267,#19268,#19269));
#4340=EDGE_LOOP('',(#19270,#19271,#19272,#19273));
#4341=EDGE_LOOP('',(#19274,#19275,#19276,#19277));
#4342=EDGE_LOOP('',(#19278,#19279,#19280,#19281,#19282,#19283));
#4343=EDGE_LOOP('',(#19284));
#4344=EDGE_LOOP('',(#19285,#19286,#19287,#19288));
#4345=EDGE_LOOP('',(#19289,#19290,#19291,#19292));
#4346=EDGE_LOOP('',(#19293,#19294,#19295,#19296));
#4347=EDGE_LOOP('',(#19297,#19298,#19299,#19300,#19301,#19302,#19303,#19304,
#19305,#19306,#19307,#19308,#19309,#19310,#19311,#19312,#19313,#19314,#19315,
#19316,#19317,#19318,#19319,#19320,#19321,#19322,#19323,#19324,#19325,#19326,
#19327,#19328,#19329,#19330,#19331,#19332));
#4348=EDGE_LOOP('',(#19333,#19334,#19335,#19336));
#4349=EDGE_LOOP('',(#19337,#19338,#19339,#19340,#19341,#19342,#19343,#19344,
#19345,#19346,#19347,#19348,#19349,#19350,#19351,#19352,#19353,#19354,#19355,
#19356,#19357,#19358,#19359,#19360,#19361,#19362,#19363,#19364,#19365,#19366,
#19367,#19368,#19369,#19370,#19371,#19372,#19373,#19374,#19375,#19376,#19377,
#19378,#19379,#19380,#19381,#19382,#19383,#19384));
#4350=EDGE_LOOP('',(#19385,#19386,#19387,#19388,#19389,#19390,#19391,#19392,
#19393,#19394,#19395,#19396,#19397,#19398,#19399,#19400,#19401,#19402,#19403,
#19404,#19405,#19406,#19407,#19408,#19409,#19410,#19411,#19412,#19413,#19414,
#19415,#19416,#19417,#19418,#19419,#19420,#19421,#19422,#19423,#19424,#19425,
#19426,#19427,#19428));
#4351=EDGE_LOOP('',(#19429,#19430,#19431,#19432,#19433,#19434,#19435,#19436,
#19437,#19438,#19439,#19440,#19441,#19442,#19443,#19444,#19445,#19446,#19447,
#19448,#19449,#19450,#19451,#19452,#19453,#19454,#19455,#19456,#19457,#19458,
#19459,#19460,#19461,#19462,#19463,#19464));
#4352=EDGE_LOOP('',(#19465,#19466,#19467,#19468));
#4353=EDGE_LOOP('',(#19469,#19470,#19471,#19472));
#4354=EDGE_LOOP('',(#19473,#19474,#19475,#19476));
#4355=EDGE_LOOP('',(#19477));
#4356=EDGE_LOOP('',(#19478,#19479,#19480,#19481));
#4357=EDGE_LOOP('',(#19482,#19483,#19484,#19485));
#4358=EDGE_LOOP('',(#19486,#19487,#19488,#19489));
#4359=EDGE_LOOP('',(#19490,#19491,#19492,#19493));
#4360=EDGE_LOOP('',(#19494,#19495,#19496,#19497));
#4361=EDGE_LOOP('',(#19498,#19499,#19500,#19501));
#4362=EDGE_LOOP('',(#19502,#19503,#19504,#19505,#19506,#19507,#19508,#19509,
#19510,#19511));
#4363=EDGE_LOOP('',(#19512,#19513,#19514,#19515));
#4364=EDGE_LOOP('',(#19516,#19517,#19518,#19519));
#4365=EDGE_LOOP('',(#19520,#19521,#19522,#19523));
#4366=EDGE_LOOP('',(#19524,#19525,#19526,#19527));
#4367=EDGE_LOOP('',(#19528,#19529,#19530,#19531));
#4368=EDGE_LOOP('',(#19532,#19533,#19534,#19535));
#4369=EDGE_LOOP('',(#19536,#19537,#19538,#19539));
#4370=EDGE_LOOP('',(#19540,#19541,#19542,#19543));
#4371=EDGE_LOOP('',(#19544,#19545,#19546,#19547));
#4372=EDGE_LOOP('',(#19548,#19549,#19550,#19551));
#4373=EDGE_LOOP('',(#19552,#19553,#19554,#19555));
#4374=EDGE_LOOP('',(#19556,#19557,#19558,#19559));
#4375=EDGE_LOOP('',(#19560,#19561,#19562,#19563));
#4376=EDGE_LOOP('',(#19564,#19565,#19566,#19567));
#4377=EDGE_LOOP('',(#19568,#19569,#19570,#19571));
#4378=EDGE_LOOP('',(#19572,#19573,#19574,#19575));
#4379=EDGE_LOOP('',(#19576,#19577,#19578,#19579));
#4380=EDGE_LOOP('',(#19580,#19581,#19582,#19583));
#4381=EDGE_LOOP('',(#19584,#19585,#19586,#19587));
#4382=EDGE_LOOP('',(#19588,#19589,#19590,#19591));
#4383=EDGE_LOOP('',(#19592,#19593,#19594,#19595));
#4384=EDGE_LOOP('',(#19596,#19597,#19598,#19599));
#4385=EDGE_LOOP('',(#19600,#19601,#19602,#19603));
#4386=EDGE_LOOP('',(#19604,#19605,#19606,#19607));
#4387=EDGE_LOOP('',(#19608,#19609,#19610,#19611));
#4388=EDGE_LOOP('',(#19612,#19613,#19614,#19615));
#4389=EDGE_LOOP('',(#19616,#19617,#19618,#19619));
#4390=EDGE_LOOP('',(#19620));
#4391=EDGE_LOOP('',(#19621,#19622,#19623,#19624));
#4392=EDGE_LOOP('',(#19625,#19626,#19627,#19628));
#4393=EDGE_LOOP('',(#19629,#19630,#19631,#19632,#19633,#19634,#19635,#19636,
#19637,#19638));
#4394=EDGE_LOOP('',(#19639,#19640,#19641,#19642));
#4395=EDGE_LOOP('',(#19643,#19644,#19645,#19646));
#4396=EDGE_LOOP('',(#19647,#19648,#19649,#19650));
#4397=EDGE_LOOP('',(#19651,#19652,#19653,#19654));
#4398=EDGE_LOOP('',(#19655,#19656,#19657,#19658));
#4399=EDGE_LOOP('',(#19659,#19660,#19661,#19662));
#4400=EDGE_LOOP('',(#19663,#19664,#19665,#19666));
#4401=EDGE_LOOP('',(#19667,#19668,#19669,#19670));
#4402=EDGE_LOOP('',(#19671));
#4403=EDGE_LOOP('',(#19672,#19673,#19674,#19675,#19676,#19677,#19678,#19679,
#19680,#19681,#19682,#19683,#19684,#19685,#19686,#19687,#19688,#19689,#19690,
#19691,#19692,#19693,#19694,#19695,#19696,#19697,#19698,#19699,#19700,#19701,
#19702,#19703,#19704,#19705,#19706,#19707,#19708,#19709,#19710,#19711,#19712,
#19713,#19714,#19715,#19716,#19717,#19718,#19719));
#4404=EDGE_LOOP('',(#19720,#19721,#19722,#19723,#19724,#19725,#19726,#19727,
#19728,#19729,#19730,#19731,#19732,#19733,#19734,#19735,#19736,#19737,#19738,
#19739,#19740,#19741,#19742,#19743,#19744,#19745,#19746,#19747,#19748,#19749,
#19750,#19751,#19752,#19753,#19754,#19755,#19756,#19757,#19758,#19759,#19760,
#19761,#19762,#19763));
#4405=EDGE_LOOP('',(#19764,#19765,#19766,#19767));
#4406=EDGE_LOOP('',(#19768,#19769,#19770,#19771));
#4407=EDGE_LOOP('',(#19772,#19773,#19774,#19775));
#4408=EDGE_LOOP('',(#19776,#19777,#19778,#19779));
#4409=EDGE_LOOP('',(#19780,#19781,#19782,#19783,#19784,#19785,#19786));
#4410=EDGE_LOOP('',(#19787,#19788,#19789,#19790,#19791,#19792,#19793));
#4411=EDGE_LOOP('',(#19794,#19795,#19796,#19797,#19798,#19799,#19800));
#4412=EDGE_LOOP('',(#19801,#19802,#19803,#19804,#19805,#19806,#19807));
#4413=EDGE_LOOP('',(#19808,#19809,#19810,#19811));
#4414=EDGE_LOOP('',(#19812,#19813,#19814,#19815));
#4415=EDGE_LOOP('',(#19816,#19817,#19818,#19819));
#4416=EDGE_LOOP('',(#19820));
#4417=EDGE_LOOP('',(#19821,#19822,#19823));
#4418=EDGE_LOOP('',(#19824,#19825,#19826));
#4419=EDGE_LOOP('',(#19827,#19828,#19829,#19830,#19831,#19832));
#4420=EDGE_LOOP('',(#19833,#19834,#19835,#19836,#19837,#19838,#19839,#19840,
#19841,#19842,#19843,#19844,#19845));
#4421=EDGE_LOOP('',(#19846,#19847,#19848,#19849,#19850,#19851));
#4422=EDGE_LOOP('',(#19852,#19853,#19854,#19855,#19856,#19857));
#4423=EDGE_LOOP('',(#19858));
#4424=EDGE_LOOP('',(#19859,#19860,#19861,#19862,#19863,#19864));
#4425=EDGE_LOOP('',(#19865));
#4426=EDGE_LOOP('',(#19866,#19867,#19868));
#4427=EDGE_LOOP('',(#19869,#19870,#19871));
#4428=EDGE_LOOP('',(#19872,#19873,#19874));
#4429=EDGE_LOOP('',(#19875,#19876,#19877));
#4430=EDGE_LOOP('',(#19878,#19879,#19880));
#4431=EDGE_LOOP('',(#19881,#19882,#19883));
#4432=EDGE_LOOP('',(#19884,#19885,#19886,#19887,#19888));
#4433=EDGE_LOOP('',(#19889,#19890,#19891,#19892,#19893));
#4434=EDGE_LOOP('',(#19894,#19895,#19896,#19897,#19898));
#4435=EDGE_LOOP('',(#19899,#19900,#19901,#19902,#19903));
#4436=EDGE_LOOP('',(#19904,#19905,#19906,#19907,#19908));
#4437=EDGE_LOOP('',(#19909,#19910,#19911,#19912,#19913));
#4438=EDGE_LOOP('',(#19914,#19915,#19916,#19917,#19918,#19919));
#4439=EDGE_LOOP('',(#19920,#19921,#19922));
#4440=EDGE_LOOP('',(#19923,#19924,#19925));
#4441=EDGE_LOOP('',(#19926,#19927,#19928));
#4442=EDGE_LOOP('',(#19929,#19930,#19931));
#4443=EDGE_LOOP('',(#19932,#19933,#19934));
#4444=EDGE_LOOP('',(#19935,#19936,#19937));
#4445=EDGE_LOOP('',(#19938,#19939,#19940));
#4446=EDGE_LOOP('',(#19941,#19942,#19943));
#4447=EDGE_LOOP('',(#19944,#19945,#19946));
#4448=EDGE_LOOP('',(#19947,#19948,#19949));
#4449=EDGE_LOOP('',(#19950,#19951,#19952,#19953,#19954,#19955));
#4450=EDGE_LOOP('',(#19956,#19957,#19958,#19959,#19960,#19961));
#4451=EDGE_LOOP('',(#19962,#19963,#19964,#19965,#19966,#19967));
#4452=EDGE_LOOP('',(#19968,#19969,#19970,#19971,#19972,#19973));
#4453=EDGE_LOOP('',(#19974,#19975,#19976,#19977,#19978,#19979));
#4454=EDGE_LOOP('',(#19980,#19981,#19982,#19983,#19984,#19985));
#4455=EDGE_LOOP('',(#19986));
#4456=EDGE_LOOP('',(#19987));
#4457=EDGE_LOOP('',(#19988,#19989,#19990,#19991,#19992,#19993,#19994,#19995));
#4458=EDGE_LOOP('',(#19996,#19997,#19998,#19999));
#4459=EDGE_LOOP('',(#20000,#20001,#20002,#20003));
#4460=EDGE_LOOP('',(#20004,#20005,#20006,#20007));
#4461=EDGE_LOOP('',(#20008,#20009,#20010,#20011));
#4462=EDGE_LOOP('',(#20012,#20013,#20014,#20015));
#4463=EDGE_LOOP('',(#20016,#20017,#20018,#20019,#20020));
#4464=EDGE_LOOP('',(#20021,#20022,#20023,#20024,#20025));
#4465=EDGE_LOOP('',(#20026,#20027,#20028,#20029));
#4466=EDGE_LOOP('',(#20030,#20031,#20032,#20033));
#4467=EDGE_LOOP('',(#20034,#20035,#20036,#20037));
#4468=EDGE_LOOP('',(#20038,#20039,#20040,#20041,#20042));
#4469=EDGE_LOOP('',(#20043,#20044,#20045,#20046,#20047));
#4470=EDGE_LOOP('',(#20048));
#4471=EDGE_LOOP('',(#20049));
#4472=EDGE_LOOP('',(#20050));
#4473=EDGE_LOOP('',(#20051));
#4474=EDGE_LOOP('',(#20052));
#4475=EDGE_LOOP('',(#20053));
#4476=EDGE_LOOP('',(#20054));
#4477=EDGE_LOOP('',(#20055));
#4478=EDGE_LOOP('',(#20056));
#4479=EDGE_LOOP('',(#20057));
#4480=EDGE_LOOP('',(#20058,#20059,#20060,#20061,#20062));
#4481=EDGE_LOOP('',(#20063,#20064,#20065,#20066));
#4482=EDGE_LOOP('',(#20067));
#4483=EDGE_LOOP('',(#20068,#20069,#20070,#20071,#20072));
#4484=EDGE_LOOP('',(#20073,#20074,#20075,#20076,#20077));
#4485=EDGE_LOOP('',(#20078,#20079,#20080,#20081));
#4486=EDGE_LOOP('',(#20082,#20083,#20084,#20085));
#4487=EDGE_LOOP('',(#20086,#20087,#20088,#20089));
#4488=EDGE_LOOP('',(#20090,#20091,#20092,#20093));
#4489=EDGE_LOOP('',(#20094,#20095,#20096,#20097));
#4490=EDGE_LOOP('',(#20098,#20099,#20100,#20101));
#4491=EDGE_LOOP('',(#20102,#20103,#20104,#20105));
#4492=EDGE_LOOP('',(#20106,#20107,#20108,#20109));
#4493=EDGE_LOOP('',(#20110,#20111,#20112,#20113));
#4494=EDGE_LOOP('',(#20114,#20115,#20116,#20117));
#4495=EDGE_LOOP('',(#20118,#20119,#20120,#20121));
#4496=EDGE_LOOP('',(#20122,#20123,#20124,#20125));
#4497=EDGE_LOOP('',(#20126,#20127,#20128,#20129));
#4498=EDGE_LOOP('',(#20130));
#4499=EDGE_LOOP('',(#20131,#20132,#20133,#20134));
#4500=EDGE_LOOP('',(#20135,#20136,#20137,#20138));
#4501=EDGE_LOOP('',(#20139,#20140,#20141,#20142));
#4502=EDGE_LOOP('',(#20143,#20144,#20145,#20146));
#4503=EDGE_LOOP('',(#20147));
#4504=EDGE_LOOP('',(#20148));
#4505=EDGE_LOOP('',(#20149));
#4506=EDGE_LOOP('',(#20150));
#4507=EDGE_LOOP('',(#20151));
#4508=EDGE_LOOP('',(#20152));
#4509=EDGE_LOOP('',(#20153));
#4510=EDGE_LOOP('',(#20154,#20155,#20156,#20157));
#4511=EDGE_LOOP('',(#20158,#20159,#20160,#20161));
#4512=EDGE_LOOP('',(#20162,#20163,#20164,#20165));
#4513=EDGE_LOOP('',(#20166));
#4514=EDGE_LOOP('',(#20167,#20168,#20169,#20170));
#4515=EDGE_LOOP('',(#20171,#20172,#20173,#20174));
#4516=EDGE_LOOP('',(#20175,#20176,#20177,#20178));
#4517=EDGE_LOOP('',(#20179,#20180,#20181,#20182));
#4518=EDGE_LOOP('',(#20183));
#4519=EDGE_LOOP('',(#20184));
#4520=EDGE_LOOP('',(#20185));
#4521=EDGE_LOOP('',(#20186));
#4522=EDGE_LOOP('',(#20187));
#4523=EDGE_LOOP('',(#20188));
#4524=EDGE_LOOP('',(#20189));
#4525=EDGE_LOOP('',(#20190));
#4526=EDGE_LOOP('',(#20191));
#4527=EDGE_LOOP('',(#20192));
#4528=EDGE_LOOP('',(#20193));
#4529=EDGE_LOOP('',(#20194));
#4530=EDGE_LOOP('',(#20195));
#4531=EDGE_LOOP('',(#20196));
#4532=EDGE_LOOP('',(#20197));
#4533=EDGE_LOOP('',(#20198));
#4534=EDGE_LOOP('',(#20199));
#4535=EDGE_LOOP('',(#20200,#20201,#20202,#20203,#20204,#20205,#20206,#20207));
#4536=EDGE_LOOP('',(#20208,#20209,#20210,#20211,#20212,#20213,#20214,#20215));
#4537=EDGE_LOOP('',(#20216,#20217,#20218,#20219));
#4538=EDGE_LOOP('',(#20220,#20221,#20222,#20223));
#4539=EDGE_LOOP('',(#20224,#20225,#20226,#20227));
#4540=EDGE_LOOP('',(#20228,#20229,#20230,#20231));
#4541=EDGE_LOOP('',(#20232,#20233,#20234,#20235));
#4542=EDGE_LOOP('',(#20236,#20237,#20238,#20239));
#4543=EDGE_LOOP('',(#20240,#20241,#20242,#20243));
#4544=EDGE_LOOP('',(#20244,#20245,#20246,#20247));
#4545=EDGE_LOOP('',(#20248));
#4546=EDGE_LOOP('',(#20249,#20250,#20251,#20252));
#4547=EDGE_LOOP('',(#20253,#20254,#20255,#20256));
#4548=EDGE_LOOP('',(#20257,#20258,#20259,#20260));
#4549=EDGE_LOOP('',(#20261));
#4550=EDGE_LOOP('',(#20262));
#4551=EDGE_LOOP('',(#20263,#20264,#20265,#20266));
#4552=EDGE_LOOP('',(#20267,#20268,#20269,#20270));
#4553=EDGE_LOOP('',(#20271,#20272,#20273,#20274));
#4554=EDGE_LOOP('',(#20275));
#4555=EDGE_LOOP('',(#20276,#20277,#20278,#20279));
#4556=EDGE_LOOP('',(#20280,#20281,#20282,#20283));
#4557=EDGE_LOOP('',(#20284,#20285,#20286,#20287));
#4558=EDGE_LOOP('',(#20288,#20289,#20290,#20291));
#4559=EDGE_LOOP('',(#20292,#20293,#20294,#20295));
#4560=EDGE_LOOP('',(#20296,#20297,#20298,#20299,#20300,#20301,#20302,#20303,
#20304,#20305,#20306,#20307));
#4561=EDGE_LOOP('',(#20308));
#4562=EDGE_LOOP('',(#20309,#20310,#20311,#20312,#20313,#20314,#20315,#20316,
#20317,#20318,#20319,#20320));
#4563=EDGE_LOOP('',(#20321));
#4564=EDGE_LOOP('',(#20322));
#4565=EDGE_LOOP('',(#20323));
#4566=EDGE_LOOP('',(#20324));
#4567=EDGE_LOOP('',(#20325));
#4568=EDGE_LOOP('',(#20326));
#4569=EDGE_LOOP('',(#20327));
#4570=EDGE_LOOP('',(#20328));
#4571=EDGE_LOOP('',(#20329));
#4572=EDGE_LOOP('',(#20330,#20331,#20332,#20333));
#4573=EDGE_LOOP('',(#20334,#20335,#20336,#20337));
#4574=EDGE_LOOP('',(#20338,#20339,#20340,#20341));
#4575=EDGE_LOOP('',(#20342,#20343,#20344,#20345));
#4576=EDGE_LOOP('',(#20346,#20347,#20348,#20349,#20350,#20351,#20352,#20353,
#20354,#20355,#20356,#20357));
#4577=EDGE_LOOP('',(#20358));
#4578=EDGE_LOOP('',(#20359));
#4579=EDGE_LOOP('',(#20360,#20361,#20362,#20363,#20364,#20365,#20366,#20367,
#20368,#20369,#20370,#20371));
#4580=EDGE_LOOP('',(#20372));
#4581=EDGE_LOOP('',(#20373));
#4582=EDGE_LOOP('',(#20374,#20375,#20376,#20377));
#4583=EDGE_LOOP('',(#20378,#20379,#20380,#20381));
#4584=EDGE_LOOP('',(#20382,#20383,#20384,#20385));
#4585=EDGE_LOOP('',(#20386,#20387,#20388,#20389));
#4586=EDGE_LOOP('',(#20390,#20391,#20392,#20393));
#4587=EDGE_LOOP('',(#20394,#20395,#20396,#20397));
#4588=EDGE_LOOP('',(#20398,#20399,#20400,#20401));
#4589=EDGE_LOOP('',(#20402,#20403,#20404,#20405));
#4590=EDGE_LOOP('',(#20406,#20407,#20408,#20409));
#4591=EDGE_LOOP('',(#20410,#20411,#20412,#20413));
#4592=EDGE_LOOP('',(#20414,#20415,#20416,#20417));
#4593=EDGE_LOOP('',(#20418,#20419,#20420,#20421));
#4594=EDGE_LOOP('',(#20422,#20423,#20424,#20425));
#4595=EDGE_LOOP('',(#20426,#20427,#20428,#20429));
#4596=EDGE_LOOP('',(#20430,#20431,#20432,#20433));
#4597=EDGE_LOOP('',(#20434,#20435,#20436,#20437));
#4598=EDGE_LOOP('',(#20438,#20439,#20440,#20441));
#4599=EDGE_LOOP('',(#20442,#20443,#20444,#20445));
#4600=EDGE_LOOP('',(#20446,#20447,#20448,#20449));
#4601=EDGE_LOOP('',(#20450,#20451,#20452,#20453));
#4602=EDGE_LOOP('',(#20454,#20455,#20456,#20457));
#4603=EDGE_LOOP('',(#20458,#20459,#20460,#20461));
#4604=EDGE_LOOP('',(#20462,#20463,#20464,#20465));
#4605=EDGE_LOOP('',(#20466,#20467,#20468,#20469));
#4606=EDGE_LOOP('',(#20470,#20471,#20472,#20473));
#4607=EDGE_LOOP('',(#20474,#20475,#20476,#20477));
#4608=EDGE_LOOP('',(#20478,#20479,#20480,#20481));
#4609=EDGE_LOOP('',(#20482,#20483,#20484,#20485));
#4610=EDGE_LOOP('',(#20486,#20487,#20488,#20489));
#4611=EDGE_LOOP('',(#20490,#20491,#20492,#20493));
#4612=EDGE_LOOP('',(#20494,#20495,#20496,#20497));
#4613=EDGE_LOOP('',(#20498));
#4614=EDGE_LOOP('',(#20499));
#4615=EDGE_LOOP('',(#20500));
#4616=EDGE_LOOP('',(#20501));
#4617=EDGE_LOOP('',(#20502));
#4618=EDGE_LOOP('',(#20503));
#4619=EDGE_LOOP('',(#20504));
#4620=EDGE_LOOP('',(#20505));
#4621=EDGE_LOOP('',(#20506,#20507,#20508,#20509,#20510,#20511,#20512,#20513,
#20514,#20515,#20516,#20517));
#4622=EDGE_LOOP('',(#20518,#20519,#20520,#20521,#20522,#20523,#20524,#20525));
#4623=EDGE_LOOP('',(#20526,#20527,#20528,#20529));
#4624=EDGE_LOOP('',(#20530));
#4625=EDGE_LOOP('',(#20531));
#4626=EDGE_LOOP('',(#20532,#20533,#20534,#20535));
#4627=EDGE_LOOP('',(#20536,#20537,#20538,#20539));
#4628=EDGE_LOOP('',(#20540,#20541,#20542,#20543));
#4629=EDGE_LOOP('',(#20544));
#4630=EDGE_LOOP('',(#20545));
#4631=EDGE_LOOP('',(#20546));
#4632=EDGE_LOOP('',(#20547));
#4633=EDGE_LOOP('',(#20548,#20549,#20550,#20551));
#4634=EDGE_LOOP('',(#20552,#20553,#20554,#20555));
#4635=EDGE_LOOP('',(#20556,#20557,#20558,#20559));
#4636=EDGE_LOOP('',(#20560));
#4637=EDGE_LOOP('',(#20561));
#4638=EDGE_LOOP('',(#20562,#20563,#20564,#20565));
#4639=EDGE_LOOP('',(#20566,#20567,#20568,#20569));
#4640=EDGE_LOOP('',(#20570,#20571,#20572,#20573));
#4641=EDGE_LOOP('',(#20574,#20575,#20576,#20577));
#4642=EDGE_LOOP('',(#20578,#20579,#20580,#20581));
#4643=EDGE_LOOP('',(#20582,#20583,#20584,#20585,#20586,#20587,#20588,#20589,
#20590,#20591,#20592,#20593));
#4644=EDGE_LOOP('',(#20594));
#4645=EDGE_LOOP('',(#20595));
#4646=EDGE_LOOP('',(#20596));
#4647=EDGE_LOOP('',(#20597));
#4648=EDGE_LOOP('',(#20598));
#4649=EDGE_LOOP('',(#20599));
#4650=EDGE_LOOP('',(#20600));
#4651=EDGE_LOOP('',(#20601));
#4652=EDGE_LOOP('',(#20602));
#4653=EDGE_LOOP('',(#20603,#20604,#20605,#20606,#20607,#20608,#20609,#20610));
#4654=EDGE_LOOP('',(#20611));
#4655=EDGE_LOOP('',(#20612));
#4656=EDGE_LOOP('',(#20613));
#4657=EDGE_LOOP('',(#20614));
#4658=EDGE_LOOP('',(#20615));
#4659=EDGE_LOOP('',(#20616,#20617,#20618,#20619));
#4660=EDGE_LOOP('',(#20620,#20621,#20622,#20623));
#4661=EDGE_LOOP('',(#20624,#20625,#20626,#20627));
#4662=EDGE_LOOP('',(#20628,#20629,#20630,#20631));
#4663=EDGE_LOOP('',(#20632,#20633,#20634,#20635));
#4664=EDGE_LOOP('',(#20636,#20637,#20638,#20639));
#4665=EDGE_LOOP('',(#20640,#20641,#20642,#20643));
#4666=EDGE_LOOP('',(#20644,#20645,#20646,#20647));
#4667=EDGE_LOOP('',(#20648));
#4668=EDGE_LOOP('',(#20649,#20650,#20651,#20652,#20653,#20654));
#4669=EDGE_LOOP('',(#20655));
#4670=EDGE_LOOP('',(#20656,#20657,#20658,#20659,#20660,#20661));
#4671=EDGE_LOOP('',(#20662));
#4672=EDGE_LOOP('',(#20663,#20664,#20665,#20666,#20667,#20668));
#4673=EDGE_LOOP('',(#20669));
#4674=EDGE_LOOP('',(#20670,#20671,#20672,#20673,#20674,#20675));
#4675=EDGE_LOOP('',(#20676,#20677,#20678,#20679));
#4676=EDGE_LOOP('',(#20680,#20681,#20682,#20683));
#4677=EDGE_LOOP('',(#20684,#20685,#20686,#20687));
#4678=EDGE_LOOP('',(#20688,#20689,#20690,#20691));
#4679=EDGE_LOOP('',(#20692,#20693,#20694,#20695));
#4680=EDGE_LOOP('',(#20696,#20697,#20698,#20699));
#4681=EDGE_LOOP('',(#20700,#20701,#20702,#20703,#20704,#20705));
#4682=EDGE_LOOP('',(#20706,#20707,#20708,#20709));
#4683=EDGE_LOOP('',(#20710,#20711,#20712,#20713));
#4684=EDGE_LOOP('',(#20714,#20715,#20716,#20717));
#4685=EDGE_LOOP('',(#20718,#20719,#20720,#20721));
#4686=EDGE_LOOP('',(#20722,#20723,#20724,#20725));
#4687=EDGE_LOOP('',(#20726,#20727,#20728,#20729));
#4688=EDGE_LOOP('',(#20730,#20731,#20732,#20733,#20734,#20735));
#4689=EDGE_LOOP('',(#20736,#20737,#20738,#20739));
#4690=EDGE_LOOP('',(#20740,#20741,#20742,#20743));
#4691=EDGE_LOOP('',(#20744,#20745,#20746,#20747));
#4692=EDGE_LOOP('',(#20748,#20749,#20750,#20751));
#4693=EDGE_LOOP('',(#20752,#20753,#20754,#20755));
#4694=EDGE_LOOP('',(#20756,#20757,#20758,#20759));
#4695=EDGE_LOOP('',(#20760,#20761,#20762,#20763,#20764,#20765));
#4696=EDGE_LOOP('',(#20766,#20767,#20768,#20769));
#4697=EDGE_LOOP('',(#20770,#20771,#20772,#20773));
#4698=EDGE_LOOP('',(#20774,#20775,#20776,#20777));
#4699=EDGE_LOOP('',(#20778,#20779,#20780,#20781));
#4700=EDGE_LOOP('',(#20782,#20783,#20784,#20785));
#4701=EDGE_LOOP('',(#20786,#20787,#20788,#20789));
#4702=EDGE_LOOP('',(#20790,#20791,#20792,#20793,#20794,#20795));
#4703=EDGE_LOOP('',(#20796));
#4704=EDGE_LOOP('',(#20797));
#4705=EDGE_LOOP('',(#20798));
#4706=EDGE_LOOP('',(#20799));
#4707=EDGE_LOOP('',(#20800));
#4708=EDGE_LOOP('',(#20801));
#4709=EDGE_LOOP('',(#20802));
#4710=EDGE_LOOP('',(#20803));
#4711=EDGE_LOOP('',(#20804,#20805,#20806,#20807,#20808,#20809,#20810,#20811));
#4712=EDGE_LOOP('',(#20812,#20813,#20814,#20815,#20816));
#4713=EDGE_LOOP('',(#20817,#20818,#20819,#20820,#20821));
#4714=EDGE_LOOP('',(#20822,#20823,#20824,#20825,#20826));
#4715=EDGE_LOOP('',(#20827,#20828,#20829,#20830,#20831,#20832));
#4716=EDGE_LOOP('',(#20833,#20834,#20835,#20836,#20837));
#4717=EDGE_LOOP('',(#20838,#20839,#20840,#20841));
#4718=EDGE_LOOP('',(#20842,#20843,#20844,#20845));
#4719=EDGE_LOOP('',(#20846,#20847,#20848,#20849));
#4720=EDGE_LOOP('',(#20850,#20851,#20852,#20853,#20854));
#4721=EDGE_LOOP('',(#20855,#20856));
#4722=EDGE_LOOP('',(#20857,#20858));
#4723=EDGE_LOOP('',(#20859,#20860,#20861,#20862,#20863,#20864));
#4724=EDGE_LOOP('',(#20865,#20866,#20867,#20868));
#4725=EDGE_LOOP('',(#20869,#20870));
#4726=EDGE_LOOP('',(#20871,#20872,#20873,#20874));
#4727=EDGE_LOOP('',(#20875,#20876,#20877,#20878));
#4728=EDGE_LOOP('',(#20879));
#4729=EDGE_LOOP('',(#20880));
#4730=EDGE_LOOP('',(#20881,#20882,#20883,#20884,#20885,#20886,#20887,#20888));
#4731=EDGE_LOOP('',(#20889));
#4732=EDGE_LOOP('',(#20890,#20891,#20892,#20893,#20894,#20895,#20896,#20897));
#4733=EDGE_LOOP('',(#20898));
#4734=EDGE_LOOP('',(#20899,#20900,#20901,#20902));
#4735=EDGE_LOOP('',(#20903,#20904,#20905,#20906));
#4736=EDGE_LOOP('',(#20907,#20908,#20909,#20910));
#4737=EDGE_LOOP('',(#20911,#20912,#20913,#20914));
#4738=EDGE_LOOP('',(#20915));
#4739=EDGE_LOOP('',(#20916,#20917,#20918,#20919,#20920));
#4740=EDGE_LOOP('',(#20921,#20922,#20923,#20924,#20925));
#4741=EDGE_LOOP('',(#20926,#20927,#20928,#20929,#20930));
#4742=EDGE_LOOP('',(#20931,#20932,#20933,#20934,#20935));
#4743=EDGE_LOOP('',(#20936,#20937,#20938,#20939,#20940));
#4744=EDGE_LOOP('',(#20941,#20942,#20943,#20944,#20945));
#4745=EDGE_LOOP('',(#20946,#20947,#20948));
#4746=EDGE_LOOP('',(#20949,#20950,#20951));
#4747=EDGE_LOOP('',(#20952,#20953,#20954));
#4748=EDGE_LOOP('',(#20955,#20956,#20957));
#4749=EDGE_LOOP('',(#20958,#20959,#20960));
#4750=EDGE_LOOP('',(#20961,#20962,#20963));
#4751=EDGE_LOOP('',(#20964,#20965,#20966,#20967));
#4752=EDGE_LOOP('',(#20968,#20969,#20970,#20971));
#4753=EDGE_LOOP('',(#20972));
#4754=EDGE_LOOP('',(#20973));
#4755=EDGE_LOOP('',(#20974));
#4756=EDGE_LOOP('',(#20975));
#4757=EDGE_LOOP('',(#20976,#20977,#20978,#20979));
#4758=EDGE_LOOP('',(#20980,#20981,#20982,#20983));
#4759=EDGE_LOOP('',(#20984,#20985,#20986,#20987));
#4760=EDGE_LOOP('',(#20988,#20989,#20990,#20991));
#4761=EDGE_LOOP('',(#20992,#20993,#20994,#20995));
#4762=EDGE_LOOP('',(#20996,#20997,#20998,#20999));
#4763=EDGE_LOOP('',(#21000,#21001,#21002,#21003));
#4764=EDGE_LOOP('',(#21004,#21005,#21006,#21007,#21008,#21009));
#4765=EDGE_LOOP('',(#21010,#21011,#21012,#21013,#21014,#21015));
#4766=EDGE_LOOP('',(#21016,#21017,#21018,#21019,#21020,#21021));
#4767=EDGE_LOOP('',(#21022,#21023,#21024,#21025,#21026,#21027));
#4768=EDGE_LOOP('',(#21028,#21029,#21030,#21031));
#4769=EDGE_LOOP('',(#21032,#21033,#21034,#21035));
#4770=EDGE_LOOP('',(#21036));
#4771=EDGE_LOOP('',(#21037));
#4772=EDGE_LOOP('',(#21038));
#4773=EDGE_LOOP('',(#21039));
#4774=EDGE_LOOP('',(#21040));
#4775=EDGE_LOOP('',(#21041));
#4776=EDGE_LOOP('',(#21042,#21043,#21044,#21045));
#4777=EDGE_LOOP('',(#21046,#21047,#21048,#21049));
#4778=EDGE_LOOP('',(#21050,#21051,#21052,#21053));
#4779=EDGE_LOOP('',(#21054,#21055,#21056,#21057));
#4780=EDGE_LOOP('',(#21058,#21059,#21060,#21061,#21062,#21063,#21064,#21065));
#4781=EDGE_LOOP('',(#21066));
#4782=EDGE_LOOP('',(#21067));
#4783=EDGE_LOOP('',(#21068));
#4784=EDGE_LOOP('',(#21069));
#4785=EDGE_LOOP('',(#21070));
#4786=EDGE_LOOP('',(#21071));
#4787=EDGE_LOOP('',(#21072));
#4788=EDGE_LOOP('',(#21073,#21074,#21075,#21076));
#4789=EDGE_LOOP('',(#21077));
#4790=EDGE_LOOP('',(#21078,#21079,#21080,#21081));
#4791=EDGE_LOOP('',(#21082,#21083,#21084,#21085));
#4792=EDGE_LOOP('',(#21086,#21087,#21088,#21089));
#4793=EDGE_LOOP('',(#21090,#21091,#21092,#21093));
#4794=EDGE_LOOP('',(#21094,#21095,#21096));
#4795=EDGE_LOOP('',(#21097,#21098,#21099,#21100));
#4796=EDGE_LOOP('',(#21101,#21102,#21103,#21104));
#4797=EDGE_LOOP('',(#21105,#21106,#21107,#21108));
#4798=EDGE_LOOP('',(#21109,#21110,#21111,#21112));
#4799=EDGE_LOOP('',(#21113,#21114,#21115,#21116));
#4800=EDGE_LOOP('',(#21117,#21118,#21119));
#4801=EDGE_LOOP('',(#21120,#21121,#21122,#21123));
#4802=EDGE_LOOP('',(#21124,#21125,#21126,#21127));
#4803=EDGE_LOOP('',(#21128,#21129,#21130));
#4804=EDGE_LOOP('',(#21131,#21132,#21133,#21134));
#4805=EDGE_LOOP('',(#21135,#21136,#21137,#21138));
#4806=EDGE_LOOP('',(#21139,#21140,#21141,#21142));
#4807=EDGE_LOOP('',(#21143,#21144,#21145));
#4808=EDGE_LOOP('',(#21146,#21147,#21148,#21149));
#4809=EDGE_LOOP('',(#21150,#21151,#21152,#21153));
#4810=EDGE_LOOP('',(#21154,#21155,#21156,#21157));
#4811=EDGE_LOOP('',(#21158,#21159,#21160,#21161));
#4812=EDGE_LOOP('',(#21162,#21163,#21164,#21165));
#4813=EDGE_LOOP('',(#21166,#21167,#21168,#21169));
#4814=EDGE_LOOP('',(#21170,#21171,#21172,#21173));
#4815=EDGE_LOOP('',(#21174,#21175,#21176));
#4816=EDGE_LOOP('',(#21177,#21178,#21179,#21180));
#4817=EDGE_LOOP('',(#21181,#21182,#21183,#21184));
#4818=EDGE_LOOP('',(#21185,#21186,#21187,#21188));
#4819=EDGE_LOOP('',(#21189,#21190,#21191,#21192));
#4820=EDGE_LOOP('',(#21193,#21194,#21195,#21196));
#4821=EDGE_LOOP('',(#21197,#21198,#21199));
#4822=EDGE_LOOP('',(#21200,#21201,#21202,#21203));
#4823=EDGE_LOOP('',(#21204,#21205,#21206,#21207));
#4824=EDGE_LOOP('',(#21208,#21209,#21210));
#4825=EDGE_LOOP('',(#21211,#21212,#21213,#21214));
#4826=EDGE_LOOP('',(#21215,#21216,#21217,#21218));
#4827=EDGE_LOOP('',(#21219,#21220,#21221,#21222));
#4828=EDGE_LOOP('',(#21223,#21224,#21225));
#4829=EDGE_LOOP('',(#21226,#21227,#21228,#21229));
#4830=EDGE_LOOP('',(#21230,#21231,#21232,#21233));
#4831=EDGE_LOOP('',(#21234,#21235,#21236,#21237));
#4832=EDGE_LOOP('',(#21238,#21239,#21240,#21241));
#4833=EDGE_LOOP('',(#21242,#21243,#21244,#21245));
#4834=EDGE_LOOP('',(#21246,#21247,#21248,#21249));
#4835=EDGE_LOOP('',(#21250,#21251,#21252,#21253));
#4836=EDGE_LOOP('',(#21254,#21255,#21256));
#4837=EDGE_LOOP('',(#21257,#21258,#21259,#21260));
#4838=EDGE_LOOP('',(#21261,#21262,#21263,#21264));
#4839=EDGE_LOOP('',(#21265,#21266,#21267,#21268));
#4840=EDGE_LOOP('',(#21269,#21270,#21271,#21272));
#4841=EDGE_LOOP('',(#21273,#21274,#21275,#21276));
#4842=EDGE_LOOP('',(#21277,#21278,#21279));
#4843=EDGE_LOOP('',(#21280,#21281,#21282,#21283));
#4844=EDGE_LOOP('',(#21284,#21285,#21286,#21287));
#4845=EDGE_LOOP('',(#21288,#21289,#21290));
#4846=EDGE_LOOP('',(#21291,#21292,#21293,#21294));
#4847=EDGE_LOOP('',(#21295,#21296,#21297,#21298));
#4848=EDGE_LOOP('',(#21299,#21300,#21301,#21302));
#4849=EDGE_LOOP('',(#21303,#21304,#21305));
#4850=EDGE_LOOP('',(#21306,#21307,#21308,#21309));
#4851=EDGE_LOOP('',(#21310,#21311,#21312,#21313));
#4852=EDGE_LOOP('',(#21314,#21315,#21316,#21317));
#4853=EDGE_LOOP('',(#21318,#21319,#21320,#21321));
#4854=EDGE_LOOP('',(#21322,#21323,#21324,#21325));
#4855=EDGE_LOOP('',(#21326,#21327,#21328,#21329));
#4856=EDGE_LOOP('',(#21330,#21331,#21332,#21333));
#4857=EDGE_LOOP('',(#21334,#21335,#21336));
#4858=EDGE_LOOP('',(#21337,#21338,#21339,#21340));
#4859=EDGE_LOOP('',(#21341,#21342,#21343,#21344));
#4860=EDGE_LOOP('',(#21345,#21346,#21347,#21348));
#4861=EDGE_LOOP('',(#21349,#21350,#21351,#21352));
#4862=EDGE_LOOP('',(#21353,#21354,#21355,#21356));
#4863=EDGE_LOOP('',(#21357,#21358,#21359));
#4864=EDGE_LOOP('',(#21360,#21361,#21362,#21363));
#4865=EDGE_LOOP('',(#21364,#21365,#21366,#21367));
#4866=EDGE_LOOP('',(#21368,#21369,#21370));
#4867=EDGE_LOOP('',(#21371,#21372,#21373,#21374));
#4868=EDGE_LOOP('',(#21375,#21376,#21377,#21378));
#4869=EDGE_LOOP('',(#21379,#21380,#21381,#21382));
#4870=EDGE_LOOP('',(#21383,#21384,#21385));
#4871=EDGE_LOOP('',(#21386,#21387,#21388,#21389));
#4872=EDGE_LOOP('',(#21390,#21391,#21392,#21393));
#4873=EDGE_LOOP('',(#21394,#21395,#21396,#21397));
#4874=EDGE_LOOP('',(#21398,#21399,#21400,#21401));
#4875=EDGE_LOOP('',(#21402,#21403,#21404,#21405));
#4876=EDGE_LOOP('',(#21406,#21407,#21408,#21409));
#4877=EDGE_LOOP('',(#21410,#21411,#21412,#21413));
#4878=EDGE_LOOP('',(#21414,#21415,#21416));
#4879=EDGE_LOOP('',(#21417,#21418,#21419,#21420));
#4880=EDGE_LOOP('',(#21421,#21422,#21423,#21424));
#4881=EDGE_LOOP('',(#21425,#21426,#21427,#21428));
#4882=EDGE_LOOP('',(#21429,#21430,#21431,#21432));
#4883=EDGE_LOOP('',(#21433,#21434,#21435,#21436));
#4884=EDGE_LOOP('',(#21437,#21438,#21439));
#4885=EDGE_LOOP('',(#21440,#21441,#21442,#21443));
#4886=EDGE_LOOP('',(#21444,#21445,#21446,#21447));
#4887=EDGE_LOOP('',(#21448,#21449,#21450));
#4888=EDGE_LOOP('',(#21451,#21452,#21453,#21454));
#4889=EDGE_LOOP('',(#21455,#21456,#21457,#21458));
#4890=EDGE_LOOP('',(#21459,#21460,#21461,#21462));
#4891=EDGE_LOOP('',(#21463,#21464,#21465));
#4892=EDGE_LOOP('',(#21466,#21467,#21468,#21469));
#4893=EDGE_LOOP('',(#21470,#21471,#21472,#21473));
#4894=EDGE_LOOP('',(#21474,#21475,#21476,#21477));
#4895=EDGE_LOOP('',(#21478,#21479,#21480,#21481));
#4896=EDGE_LOOP('',(#21482,#21483,#21484,#21485));
#4897=EDGE_LOOP('',(#21486,#21487,#21488,#21489));
#4898=EDGE_LOOP('',(#21490,#21491,#21492,#21493));
#4899=EDGE_LOOP('',(#21494,#21495,#21496));
#4900=EDGE_LOOP('',(#21497,#21498,#21499,#21500));
#4901=EDGE_LOOP('',(#21501,#21502,#21503,#21504));
#4902=EDGE_LOOP('',(#21505,#21506,#21507,#21508));
#4903=EDGE_LOOP('',(#21509,#21510,#21511,#21512));
#4904=EDGE_LOOP('',(#21513,#21514,#21515,#21516));
#4905=EDGE_LOOP('',(#21517,#21518,#21519));
#4906=EDGE_LOOP('',(#21520,#21521,#21522,#21523));
#4907=EDGE_LOOP('',(#21524,#21525,#21526,#21527));
#4908=EDGE_LOOP('',(#21528,#21529,#21530));
#4909=EDGE_LOOP('',(#21531,#21532,#21533,#21534));
#4910=EDGE_LOOP('',(#21535,#21536,#21537,#21538));
#4911=EDGE_LOOP('',(#21539,#21540,#21541,#21542));
#4912=EDGE_LOOP('',(#21543,#21544,#21545));
#4913=EDGE_LOOP('',(#21546,#21547,#21548,#21549));
#4914=EDGE_LOOP('',(#21550,#21551,#21552,#21553));
#4915=EDGE_LOOP('',(#21554,#21555,#21556,#21557));
#4916=EDGE_LOOP('',(#21558,#21559,#21560,#21561));
#4917=EDGE_LOOP('',(#21562,#21563,#21564,#21565));
#4918=EDGE_LOOP('',(#21566,#21567,#21568,#21569));
#4919=EDGE_LOOP('',(#21570,#21571,#21572,#21573));
#4920=EDGE_LOOP('',(#21574,#21575,#21576,#21577));
#4921=EDGE_LOOP('',(#21578,#21579,#21580,#21581));
#4922=EDGE_LOOP('',(#21582,#21583,#21584));
#4923=EDGE_LOOP('',(#21585,#21586,#21587,#21588));
#4924=EDGE_LOOP('',(#21589,#21590,#21591,#21592));
#4925=EDGE_LOOP('',(#21593,#21594,#21595,#21596));
#4926=EDGE_LOOP('',(#21597,#21598,#21599));
#4927=EDGE_LOOP('',(#21600,#21601,#21602,#21603));
#4928=EDGE_LOOP('',(#21604,#21605,#21606,#21607));
#4929=EDGE_LOOP('',(#21608,#21609,#21610,#21611));
#4930=EDGE_LOOP('',(#21612,#21613,#21614,#21615));
#4931=EDGE_LOOP('',(#21616,#21617,#21618,#21619));
#4932=EDGE_LOOP('',(#21620,#21621,#21622,#21623));
#4933=EDGE_LOOP('',(#21624,#21625,#21626));
#4934=EDGE_LOOP('',(#21627,#21628,#21629,#21630));
#4935=EDGE_LOOP('',(#21631,#21632,#21633));
#4936=EDGE_LOOP('',(#21634,#21635,#21636,#21637));
#4937=EDGE_LOOP('',(#21638,#21639,#21640,#21641));
#4938=EDGE_LOOP('',(#21642,#21643,#21644,#21645));
#4939=EDGE_LOOP('',(#21646,#21647,#21648,#21649));
#4940=EDGE_LOOP('',(#21650,#21651,#21652,#21653));
#4941=EDGE_LOOP('',(#21654,#21655,#21656));
#4942=EDGE_LOOP('',(#21657,#21658,#21659,#21660));
#4943=EDGE_LOOP('',(#21661,#21662,#21663,#21664));
#4944=EDGE_LOOP('',(#21665,#21666,#21667,#21668));
#4945=EDGE_LOOP('',(#21669,#21670,#21671,#21672));
#4946=EDGE_LOOP('',(#21673,#21674,#21675,#21676));
#4947=EDGE_LOOP('',(#21677,#21678,#21679));
#4948=EDGE_LOOP('',(#21680,#21681,#21682,#21683));
#4949=EDGE_LOOP('',(#21684,#21685,#21686,#21687));
#4950=EDGE_LOOP('',(#21688,#21689,#21690));
#4951=EDGE_LOOP('',(#21691,#21692,#21693,#21694));
#4952=EDGE_LOOP('',(#21695,#21696,#21697,#21698));
#4953=EDGE_LOOP('',(#21699,#21700,#21701,#21702));
#4954=EDGE_LOOP('',(#21703,#21704,#21705));
#4955=EDGE_LOOP('',(#21706,#21707,#21708,#21709));
#4956=EDGE_LOOP('',(#21710,#21711,#21712,#21713));
#4957=EDGE_LOOP('',(#21714,#21715,#21716,#21717));
#4958=EDGE_LOOP('',(#21718,#21719,#21720,#21721));
#4959=EDGE_LOOP('',(#21722,#21723,#21724,#21725,#21726,#21727,#21728,#21729));
#4960=EDGE_LOOP('',(#21730,#21731,#21732,#21733,#21734,#21735,#21736,#21737));
#4961=EDGE_LOOP('',(#21738,#21739,#21740,#21741,#21742,#21743,#21744,#21745));
#4962=EDGE_LOOP('',(#21746,#21747,#21748,#21749,#21750,#21751,#21752,#21753));
#4963=EDGE_LOOP('',(#21754,#21755,#21756,#21757,#21758,#21759,#21760,#21761));
#4964=EDGE_LOOP('',(#21762,#21763,#21764,#21765,#21766,#21767,#21768,#21769));
#4965=EDGE_LOOP('',(#21770,#21771,#21772,#21773,#21774,#21775,#21776,#21777));
#4966=EDGE_LOOP('',(#21778,#21779,#21780,#21781,#21782,#21783,#21784,#21785));
#4967=EDGE_LOOP('',(#21786));
#4968=EDGE_LOOP('',(#21787,#21788,#21789,#21790));
#4969=EDGE_LOOP('',(#21791));
#4970=EDGE_LOOP('',(#21792,#21793,#21794,#21795));
#4971=EDGE_LOOP('',(#21796));
#4972=EDGE_LOOP('',(#21797,#21798,#21799,#21800));
#4973=EDGE_LOOP('',(#21801,#21802,#21803,#21804,#21805,#21806,#21807,#21808,
#21809,#21810,#21811,#21812,#21813,#21814,#21815,#21816,#21817,#21818,#21819,
#21820,#21821,#21822,#21823,#21824,#21825,#21826,#21827,#21828,#21829,#21830,
#21831,#21832,#21833,#21834,#21835,#21836,#21837,#21838,#21839,#21840,#21841,
#21842,#21843,#21844,#21845,#21846,#21847,#21848));
#4974=EDGE_LOOP('',(#21849));
#4975=EDGE_LOOP('',(#21850));
#4976=EDGE_LOOP('',(#21851));
#4977=EDGE_LOOP('',(#21852));
#4978=EDGE_LOOP('',(#21853));
#4979=EDGE_LOOP('',(#21854,#21855,#21856,#21857));
#4980=EDGE_LOOP('',(#21858));
#4981=EDGE_LOOP('',(#21859,#21860,#21861,#21862));
#4982=EDGE_LOOP('',(#21863));
#4983=EDGE_LOOP('',(#21864,#21865,#21866,#21867));
#4984=EDGE_LOOP('',(#21868));
#4985=EDGE_LOOP('',(#21869,#21870,#21871,#21872));
#4986=EDGE_LOOP('',(#21873,#21874,#21875,#21876,#21877,#21878,#21879,#21880,
#21881,#21882,#21883,#21884,#21885,#21886,#21887,#21888,#21889,#21890,#21891,
#21892,#21893,#21894,#21895,#21896,#21897,#21898,#21899,#21900,#21901,#21902,
#21903,#21904,#21905,#21906,#21907,#21908,#21909,#21910,#21911,#21912,#21913,
#21914,#21915,#21916,#21917,#21918,#21919,#21920));
#4987=EDGE_LOOP('',(#21921));
#4988=EDGE_LOOP('',(#21922));
#4989=EDGE_LOOP('',(#21923));
#4990=EDGE_LOOP('',(#21924));
#4991=EDGE_LOOP('',(#21925));
#4992=EDGE_LOOP('',(#21926));
#4993=EDGE_LOOP('',(#21927,#21928,#21929,#21930,#21931,#21932));
#4994=EDGE_LOOP('',(#21933));
#4995=EDGE_LOOP('',(#21934,#21935,#21936,#21937));
#4996=EDGE_LOOP('',(#21938,#21939,#21940,#21941,#21942,#21943));
#4997=EDGE_LOOP('',(#21944,#21945,#21946,#21947));
#4998=EDGE_LOOP('',(#21948,#21949,#21950,#21951));
#4999=EDGE_LOOP('',(#21952,#21953,#21954,#21955));
#5000=EDGE_LOOP('',(#21956,#21957,#21958,#21959));
#5001=EDGE_LOOP('',(#21960,#21961,#21962,#21963));
#5002=EDGE_LOOP('',(#21964,#21965,#21966,#21967));
#5003=EDGE_LOOP('',(#21968));
#5004=EDGE_LOOP('',(#21969));
#5005=EDGE_LOOP('',(#21970,#21971,#21972,#21973));
#5006=EDGE_LOOP('',(#21974,#21975,#21976,#21977));
#5007=EDGE_LOOP('',(#21978));
#5008=EDGE_LOOP('',(#21979,#21980,#21981,#21982,#21983,#21984));
#5009=EDGE_LOOP('',(#21985,#21986,#21987,#21988,#21989,#21990));
#5010=EDGE_LOOP('',(#21991,#21992,#21993,#21994));
#5011=EDGE_LOOP('',(#21995,#21996,#21997,#21998));
#5012=EDGE_LOOP('',(#21999,#22000,#22001,#22002));
#5013=EDGE_LOOP('',(#22003,#22004,#22005,#22006));
#5014=EDGE_LOOP('',(#22007,#22008,#22009,#22010));
#5015=EDGE_LOOP('',(#22011,#22012,#22013,#22014));
#5016=EDGE_LOOP('',(#22015));
#5017=EDGE_LOOP('',(#22016,#22017,#22018,#22019));
#5018=EDGE_LOOP('',(#22020,#22021,#22022,#22023));
#5019=EDGE_LOOP('',(#22024));
#5020=EDGE_LOOP('',(#22025));
#5021=EDGE_LOOP('',(#22026,#22027,#22028,#22029));
#5022=EDGE_LOOP('',(#22030,#22031,#22032,#22033));
#5023=EDGE_LOOP('',(#22034));
#5024=EDGE_LOOP('',(#22035,#22036,#22037,#22038,#22039,#22040));
#5025=EDGE_LOOP('',(#22041,#22042,#22043,#22044,#22045,#22046));
#5026=EDGE_LOOP('',(#22047,#22048,#22049,#22050));
#5027=EDGE_LOOP('',(#22051,#22052,#22053,#22054));
#5028=EDGE_LOOP('',(#22055,#22056,#22057,#22058));
#5029=EDGE_LOOP('',(#22059,#22060,#22061,#22062));
#5030=EDGE_LOOP('',(#22063,#22064,#22065,#22066));
#5031=EDGE_LOOP('',(#22067,#22068,#22069,#22070));
#5032=EDGE_LOOP('',(#22071));
#5033=EDGE_LOOP('',(#22072,#22073,#22074,#22075));
#5034=EDGE_LOOP('',(#22076,#22077,#22078,#22079));
#5035=EDGE_LOOP('',(#22080,#22081,#22082,#22083));
#5036=EDGE_LOOP('',(#22084,#22085,#22086,#22087));
#5037=EDGE_LOOP('',(#22088,#22089,#22090,#22091));
#5038=EDGE_LOOP('',(#22092,#22093,#22094,#22095));
#5039=EDGE_LOOP('',(#22096,#22097,#22098,#22099));
#5040=EDGE_LOOP('',(#22100,#22101,#22102,#22103));
#5041=EDGE_LOOP('',(#22104,#22105,#22106,#22107));
#5042=EDGE_LOOP('',(#22108,#22109,#22110,#22111));
#5043=EDGE_LOOP('',(#22112,#22113,#22114,#22115));
#5044=EDGE_LOOP('',(#22116,#22117,#22118,#22119));
#5045=EDGE_LOOP('',(#22120,#22121,#22122,#22123,#22124,#22125,#22126,#22127,
#22128,#22129,#22130,#22131));
#5046=EDGE_LOOP('',(#22132,#22133));
#5047=EDGE_LOOP('',(#22134,#22135));
#5048=EDGE_LOOP('',(#22136,#22137,#22138,#22139));
#5049=EDGE_LOOP('',(#22140,#22141,#22142,#22143,#22144,#22145,#22146,#22147,
#22148,#22149,#22150,#22151));
#5050=EDGE_LOOP('',(#22152,#22153,#22154,#22155,#22156));
#5051=EDGE_LOOP('',(#22157,#22158));
#5052=EDGE_LOOP('',(#22159));
#5053=EDGE_LOOP('',(#22160,#22161,#22162,#22163));
#5054=EDGE_LOOP('',(#22164));
#5055=EDGE_LOOP('',(#22165));
#5056=EDGE_LOOP('',(#22166,#22167,#22168,#22169));
#5057=EDGE_LOOP('',(#22170,#22171,#22172,#22173,#22174));
#5058=EDGE_LOOP('',(#22175));
#5059=EDGE_LOOP('',(#22176,#22177,#22178,#22179,#22180));
#5060=EDGE_LOOP('',(#22181));
#5061=EDGE_LOOP('',(#22182,#22183));
#5062=EDGE_LOOP('',(#22184,#22185));
#5063=EDGE_LOOP('',(#22186,#22187,#22188,#22189,#22190));
#5064=EDGE_LOOP('',(#22191));
#5065=EDGE_LOOP('',(#22192,#22193,#22194,#22195,#22196));
#5066=EDGE_LOOP('',(#22197,#22198,#22199,#22200));
#5067=EDGE_LOOP('',(#22201));
#5068=EDGE_LOOP('',(#22202));
#5069=EDGE_LOOP('',(#22203,#22204,#22205,#22206));
#5070=EDGE_LOOP('',(#22207,#22208));
#5071=EDGE_LOOP('',(#22209));
#5072=EDGE_LOOP('',(#22210,#22211,#22212,#22213,#22214));
#5073=EDGE_LOOP('',(#22215));
#5074=EDGE_LOOP('',(#22216,#22217,#22218,#22219,#22220,#22221,#22222,#22223));
#5075=EDGE_LOOP('',(#22224,#22225,#22226,#22227));
#5076=EDGE_LOOP('',(#22228,#22229,#22230,#22231,#22232,#22233,#22234,#22235,
#22236,#22237,#22238,#22239,#22240,#22241,#22242,#22243));
#5077=EDGE_LOOP('',(#22244,#22245,#22246,#22247,#22248,#22249));
#5078=EDGE_LOOP('',(#22250,#22251,#22252,#22253,#22254,#22255));
#5079=EDGE_LOOP('',(#22256,#22257,#22258,#22259));
#5080=EDGE_LOOP('',(#22260,#22261,#22262,#22263,#22264,#22265,#22266,#22267,
#22268,#22269,#22270,#22271,#22272,#22273));
#5081=EDGE_LOOP('',(#22274,#22275,#22276,#22277));
#5082=EDGE_LOOP('',(#22278,#22279,#22280,#22281));
#5083=EDGE_LOOP('',(#22282,#22283,#22284,#22285,#22286));
#5084=EDGE_LOOP('',(#22287,#22288,#22289,#22290));
#5085=EDGE_LOOP('',(#22291,#22292,#22293,#22294));
#5086=EDGE_LOOP('',(#22295,#22296,#22297,#22298));
#5087=EDGE_LOOP('',(#22299,#22300,#22301,#22302));
#5088=EDGE_LOOP('',(#22303,#22304,#22305,#22306));
#5089=EDGE_LOOP('',(#22307,#22308,#22309,#22310));
#5090=EDGE_LOOP('',(#22311,#22312,#22313,#22314));
#5091=EDGE_LOOP('',(#22315,#22316,#22317,#22318));
#5092=EDGE_LOOP('',(#22319,#22320,#22321,#22322));
#5093=EDGE_LOOP('',(#22323,#22324,#22325,#22326));
#5094=EDGE_LOOP('',(#22327,#22328,#22329,#22330));
#5095=EDGE_LOOP('',(#22331,#22332,#22333,#22334,#22335,#22336,#22337,#22338,
#22339,#22340,#22341,#22342));
#5096=EDGE_LOOP('',(#22343,#22344));
#5097=EDGE_LOOP('',(#22345,#22346,#22347,#22348,#22349,#22350,#22351,#22352,
#22353));
#5098=EDGE_LOOP('',(#22354,#22355,#22356,#22357,#22358,#22359,#22360,#22361));
#5099=EDGE_LOOP('',(#22362,#22363,#22364));
#5100=EDGE_LOOP('',(#22365,#22366));
#5101=EDGE_LOOP('',(#22367,#22368,#22369,#22370,#22371,#22372));
#5102=EDGE_LOOP('',(#22373,#22374,#22375,#22376,#22377,#22378,#22379,#22380,
#22381,#22382,#22383));
#5103=EDGE_LOOP('',(#22384,#22385,#22386,#22387,#22388,#22389));
#5104=EDGE_LOOP('',(#22390,#22391,#22392,#22393,#22394,#22395,#22396,#22397));
#5105=EDGE_LOOP('',(#22398,#22399,#22400,#22401));
#5106=EDGE_LOOP('',(#22402,#22403,#22404,#22405));
#5107=EDGE_LOOP('',(#22406,#22407,#22408,#22409));
#5108=EDGE_LOOP('',(#22410,#22411,#22412,#22413));
#5109=EDGE_LOOP('',(#22414,#22415,#22416,#22417));
#5110=EDGE_LOOP('',(#22418,#22419,#22420,#22421));
#5111=EDGE_LOOP('',(#22422,#22423,#22424,#22425));
#5112=EDGE_LOOP('',(#22426,#22427,#22428,#22429));
#5113=EDGE_LOOP('',(#22430,#22431,#22432,#22433));
#5114=EDGE_LOOP('',(#22434,#22435,#22436,#22437));
#5115=EDGE_LOOP('',(#22438,#22439,#22440,#22441));
#5116=EDGE_LOOP('',(#22442,#22443,#22444,#22445));
#5117=EDGE_LOOP('',(#22446,#22447,#22448,#22449));
#5118=EDGE_LOOP('',(#22450,#22451,#22452,#22453));
#5119=EDGE_LOOP('',(#22454,#22455,#22456,#22457));
#5120=EDGE_LOOP('',(#22458,#22459,#22460,#22461));
#5121=EDGE_LOOP('',(#22462,#22463,#22464,#22465));
#5122=EDGE_LOOP('',(#22466,#22467,#22468,#22469));
#5123=EDGE_LOOP('',(#22470,#22471,#22472,#22473));
#5124=EDGE_LOOP('',(#22474,#22475,#22476,#22477,#22478,#22479,#22480,#22481,
#22482,#22483,#22484));
#5125=EDGE_LOOP('',(#22485,#22486,#22487,#22488,#22489,#22490));
#5126=EDGE_LOOP('',(#22491,#22492,#22493,#22494));
#5127=EDGE_LOOP('',(#22495,#22496,#22497,#22498));
#5128=EDGE_LOOP('',(#22499,#22500,#22501,#22502));
#5129=EDGE_LOOP('',(#22503,#22504,#22505,#22506));
#5130=EDGE_LOOP('',(#22507,#22508,#22509,#22510));
#5131=EDGE_LOOP('',(#22511,#22512,#22513,#22514));
#5132=EDGE_LOOP('',(#22515,#22516,#22517,#22518));
#5133=EDGE_LOOP('',(#22519,#22520,#22521,#22522));
#5134=EDGE_LOOP('',(#22523,#22524,#22525,#22526));
#5135=EDGE_LOOP('',(#22527,#22528,#22529,#22530));
#5136=EDGE_LOOP('',(#22531,#22532,#22533,#22534));
#5137=EDGE_LOOP('',(#22535,#22536,#22537,#22538));
#5138=EDGE_LOOP('',(#22539,#22540,#22541,#22542,#22543,#22544));
#5139=EDGE_LOOP('',(#22545,#22546,#22547,#22548));
#5140=EDGE_LOOP('',(#22549,#22550,#22551,#22552));
#5141=EDGE_LOOP('',(#22553,#22554,#22555,#22556));
#5142=EDGE_LOOP('',(#22557,#22558,#22559,#22560));
#5143=EDGE_LOOP('',(#22561,#22562,#22563,#22564));
#5144=EDGE_LOOP('',(#22565,#22566,#22567,#22568));
#5145=EDGE_LOOP('',(#22569,#22570,#22571,#22572));
#5146=EDGE_LOOP('',(#22573,#22574,#22575,#22576));
#5147=EDGE_LOOP('',(#22577,#22578,#22579,#22580));
#5148=EDGE_LOOP('',(#22581,#22582,#22583,#22584));
#5149=EDGE_LOOP('',(#22585,#22586,#22587,#22588));
#5150=EDGE_LOOP('',(#22589,#22590,#22591,#22592));
#5151=EDGE_LOOP('',(#22593,#22594,#22595,#22596));
#5152=EDGE_LOOP('',(#22597,#22598,#22599,#22600,#22601,#22602,#22603,#22604,
#22605));
#5153=EDGE_LOOP('',(#22606,#22607,#22608,#22609));
#5154=EDGE_LOOP('',(#22610));
#5155=EDGE_LOOP('',(#22611,#22612,#22613,#22614,#22615,#22616));
#5156=EDGE_LOOP('',(#22617));
#5157=EDGE_LOOP('',(#22618,#22619,#22620,#22621));
#5158=EDGE_LOOP('',(#22622,#22623,#22624,#22625,#22626,#22627));
#5159=EDGE_LOOP('',(#22628,#22629,#22630,#22631));
#5160=EDGE_LOOP('',(#22632,#22633,#22634,#22635));
#5161=EDGE_LOOP('',(#22636,#22637,#22638,#22639));
#5162=EDGE_LOOP('',(#22640,#22641,#22642,#22643));
#5163=EDGE_LOOP('',(#22644,#22645,#22646,#22647));
#5164=EDGE_LOOP('',(#22648,#22649,#22650,#22651));
#5165=EDGE_LOOP('',(#22652));
#5166=EDGE_LOOP('',(#22653));
#5167=EDGE_LOOP('',(#22654,#22655,#22656,#22657));
#5168=EDGE_LOOP('',(#22658,#22659,#22660,#22661));
#5169=EDGE_LOOP('',(#22662));
#5170=EDGE_LOOP('',(#22663,#22664,#22665,#22666,#22667,#22668));
#5171=EDGE_LOOP('',(#22669,#22670,#22671,#22672,#22673,#22674));
#5172=EDGE_LOOP('',(#22675,#22676,#22677,#22678));
#5173=EDGE_LOOP('',(#22679,#22680,#22681,#22682));
#5174=EDGE_LOOP('',(#22683,#22684,#22685,#22686));
#5175=EDGE_LOOP('',(#22687,#22688,#22689,#22690));
#5176=EDGE_LOOP('',(#22691,#22692,#22693,#22694));
#5177=EDGE_LOOP('',(#22695,#22696,#22697,#22698));
#5178=EDGE_LOOP('',(#22699));
#5179=EDGE_LOOP('',(#22700,#22701,#22702,#22703));
#5180=EDGE_LOOP('',(#22704,#22705,#22706,#22707));
#5181=EDGE_LOOP('',(#22708));
#5182=EDGE_LOOP('',(#22709));
#5183=EDGE_LOOP('',(#22710,#22711,#22712,#22713));
#5184=EDGE_LOOP('',(#22714,#22715,#22716,#22717));
#5185=EDGE_LOOP('',(#22718));
#5186=EDGE_LOOP('',(#22719,#22720,#22721,#22722,#22723,#22724));
#5187=EDGE_LOOP('',(#22725,#22726,#22727,#22728,#22729,#22730));
#5188=EDGE_LOOP('',(#22731,#22732,#22733,#22734));
#5189=EDGE_LOOP('',(#22735,#22736,#22737,#22738));
#5190=EDGE_LOOP('',(#22739,#22740,#22741,#22742));
#5191=EDGE_LOOP('',(#22743,#22744,#22745,#22746));
#5192=EDGE_LOOP('',(#22747,#22748,#22749,#22750));
#5193=EDGE_LOOP('',(#22751,#22752,#22753,#22754));
#5194=EDGE_LOOP('',(#22755));
#5195=EDGE_LOOP('',(#22756,#22757,#22758,#22759));
#5196=EDGE_LOOP('',(#22760,#22761,#22762,#22763));
#5197=EDGE_LOOP('',(#22764,#22765,#22766,#22767));
#5198=EDGE_LOOP('',(#22768,#22769,#22770,#22771));
#5199=EDGE_LOOP('',(#22772,#22773,#22774,#22775));
#5200=EDGE_LOOP('',(#22776,#22777,#22778,#22779));
#5201=EDGE_LOOP('',(#22780,#22781,#22782,#22783));
#5202=EDGE_LOOP('',(#22784,#22785,#22786,#22787));
#5203=EDGE_LOOP('',(#22788,#22789,#22790,#22791));
#5204=EDGE_LOOP('',(#22792,#22793,#22794,#22795));
#5205=EDGE_LOOP('',(#22796,#22797,#22798,#22799));
#5206=EDGE_LOOP('',(#22800,#22801,#22802,#22803));
#5207=EDGE_LOOP('',(#22804,#22805,#22806,#22807,#22808,#22809,#22810,#22811,
#22812,#22813,#22814,#22815));
#5208=EDGE_LOOP('',(#22816,#22817));
#5209=EDGE_LOOP('',(#22818,#22819));
#5210=EDGE_LOOP('',(#22820,#22821,#22822,#22823));
#5211=EDGE_LOOP('',(#22824,#22825,#22826,#22827,#22828,#22829,#22830,#22831,
#22832,#22833,#22834,#22835));
#5212=EDGE_LOOP('',(#22836,#22837,#22838,#22839,#22840));
#5213=EDGE_LOOP('',(#22841,#22842));
#5214=EDGE_LOOP('',(#22843));
#5215=EDGE_LOOP('',(#22844,#22845,#22846,#22847));
#5216=EDGE_LOOP('',(#22848));
#5217=EDGE_LOOP('',(#22849));
#5218=EDGE_LOOP('',(#22850,#22851,#22852,#22853));
#5219=EDGE_LOOP('',(#22854,#22855,#22856,#22857,#22858));
#5220=EDGE_LOOP('',(#22859));
#5221=EDGE_LOOP('',(#22860,#22861,#22862,#22863,#22864));
#5222=EDGE_LOOP('',(#22865));
#5223=EDGE_LOOP('',(#22866,#22867));
#5224=EDGE_LOOP('',(#22868,#22869));
#5225=EDGE_LOOP('',(#22870,#22871,#22872,#22873,#22874));
#5226=EDGE_LOOP('',(#22875));
#5227=EDGE_LOOP('',(#22876,#22877,#22878,#22879,#22880));
#5228=EDGE_LOOP('',(#22881,#22882,#22883,#22884));
#5229=EDGE_LOOP('',(#22885));
#5230=EDGE_LOOP('',(#22886));
#5231=EDGE_LOOP('',(#22887,#22888,#22889,#22890));
#5232=EDGE_LOOP('',(#22891,#22892));
#5233=EDGE_LOOP('',(#22893));
#5234=EDGE_LOOP('',(#22894,#22895,#22896,#22897,#22898));
#5235=EDGE_LOOP('',(#22899));
#5236=EDGE_LOOP('',(#22900,#22901,#22902,#22903,#22904,#22905,#22906,#22907));
#5237=EDGE_LOOP('',(#22908,#22909,#22910,#22911));
#5238=EDGE_LOOP('',(#22912,#22913,#22914,#22915,#22916,#22917,#22918,#22919,
#22920,#22921,#22922,#22923,#22924,#22925,#22926,#22927));
#5239=EDGE_LOOP('',(#22928,#22929,#22930,#22931));
#5240=EDGE_LOOP('',(#22932,#22933,#22934,#22935));
#5241=EDGE_LOOP('',(#22936,#22937,#22938,#22939));
#5242=EDGE_LOOP('',(#22940,#22941,#22942,#22943,#22944,#22945));
#5243=EDGE_LOOP('',(#22946,#22947,#22948,#22949));
#5244=EDGE_LOOP('',(#22950,#22951,#22952,#22953));
#5245=EDGE_LOOP('',(#22954,#22955,#22956,#22957));
#5246=EDGE_LOOP('',(#22958));
#5247=EDGE_LOOP('',(#22959,#22960,#22961,#22962));
#5248=EDGE_LOOP('',(#22963,#22964,#22965,#22966));
#5249=EDGE_LOOP('',(#22967,#22968,#22969,#22970));
#5250=EDGE_LOOP('',(#22971,#22972,#22973,#22974));
#5251=EDGE_LOOP('',(#22975,#22976,#22977,#22978));
#5252=EDGE_LOOP('',(#22979,#22980,#22981,#22982));
#5253=EDGE_LOOP('',(#22983,#22984,#22985,#22986));
#5254=EDGE_LOOP('',(#22987,#22988,#22989,#22990));
#5255=EDGE_LOOP('',(#22991,#22992,#22993,#22994,#22995,#22996,#22997,#22998,
#22999,#23000,#23001,#23002));
#5256=EDGE_LOOP('',(#23003,#23004));
#5257=EDGE_LOOP('',(#23005,#23006,#23007,#23008,#23009,#23010,#23011,#23012,
#23013));
#5258=EDGE_LOOP('',(#23014,#23015,#23016,#23017,#23018,#23019,#23020,#23021));
#5259=EDGE_LOOP('',(#23022,#23023,#23024));
#5260=EDGE_LOOP('',(#23025,#23026));
#5261=EDGE_LOOP('',(#23027,#23028,#23029,#23030,#23031,#23032));
#5262=EDGE_LOOP('',(#23033,#23034,#23035,#23036,#23037,#23038,#23039,#23040,
#23041,#23042,#23043));
#5263=EDGE_LOOP('',(#23044,#23045,#23046,#23047,#23048,#23049));
#5264=EDGE_LOOP('',(#23050,#23051,#23052,#23053,#23054,#23055,#23056,#23057));
#5265=EDGE_LOOP('',(#23058,#23059,#23060,#23061));
#5266=EDGE_LOOP('',(#23062,#23063,#23064,#23065));
#5267=EDGE_LOOP('',(#23066,#23067,#23068,#23069));
#5268=EDGE_LOOP('',(#23070,#23071,#23072,#23073));
#5269=EDGE_LOOP('',(#23074,#23075,#23076,#23077));
#5270=EDGE_LOOP('',(#23078,#23079,#23080,#23081));
#5271=EDGE_LOOP('',(#23082,#23083,#23084,#23085));
#5272=EDGE_LOOP('',(#23086,#23087,#23088,#23089));
#5273=EDGE_LOOP('',(#23090,#23091,#23092,#23093));
#5274=EDGE_LOOP('',(#23094,#23095,#23096,#23097));
#5275=EDGE_LOOP('',(#23098,#23099,#23100,#23101));
#5276=EDGE_LOOP('',(#23102,#23103,#23104,#23105));
#5277=EDGE_LOOP('',(#23106,#23107,#23108,#23109));
#5278=EDGE_LOOP('',(#23110,#23111,#23112,#23113));
#5279=EDGE_LOOP('',(#23114,#23115,#23116,#23117));
#5280=EDGE_LOOP('',(#23118,#23119,#23120,#23121));
#5281=EDGE_LOOP('',(#23122,#23123,#23124,#23125));
#5282=EDGE_LOOP('',(#23126,#23127,#23128,#23129));
#5283=EDGE_LOOP('',(#23130,#23131,#23132,#23133));
#5284=EDGE_LOOP('',(#23134,#23135,#23136,#23137,#23138,#23139,#23140,#23141,
#23142,#23143,#23144));
#5285=EDGE_LOOP('',(#23145,#23146,#23147,#23148,#23149,#23150));
#5286=EDGE_LOOP('',(#23151,#23152,#23153,#23154));
#5287=EDGE_LOOP('',(#23155,#23156,#23157,#23158));
#5288=EDGE_LOOP('',(#23159,#23160,#23161,#23162));
#5289=EDGE_LOOP('',(#23163,#23164,#23165,#23166));
#5290=EDGE_LOOP('',(#23167,#23168,#23169,#23170));
#5291=EDGE_LOOP('',(#23171,#23172,#23173,#23174));
#5292=EDGE_LOOP('',(#23175,#23176,#23177,#23178));
#5293=EDGE_LOOP('',(#23179,#23180,#23181,#23182));
#5294=EDGE_LOOP('',(#23183,#23184,#23185,#23186));
#5295=EDGE_LOOP('',(#23187,#23188,#23189,#23190));
#5296=EDGE_LOOP('',(#23191,#23192,#23193,#23194));
#5297=EDGE_LOOP('',(#23195,#23196,#23197,#23198));
#5298=EDGE_LOOP('',(#23199,#23200,#23201,#23202,#23203,#23204));
#5299=EDGE_LOOP('',(#23205,#23206,#23207,#23208));
#5300=EDGE_LOOP('',(#23209,#23210,#23211,#23212));
#5301=EDGE_LOOP('',(#23213,#23214,#23215,#23216));
#5302=EDGE_LOOP('',(#23217,#23218,#23219,#23220));
#5303=EDGE_LOOP('',(#23221,#23222,#23223,#23224));
#5304=EDGE_LOOP('',(#23225,#23226,#23227,#23228));
#5305=EDGE_LOOP('',(#23229,#23230,#23231,#23232));
#5306=EDGE_LOOP('',(#23233,#23234,#23235,#23236));
#5307=EDGE_LOOP('',(#23237,#23238,#23239,#23240));
#5308=EDGE_LOOP('',(#23241,#23242,#23243,#23244));
#5309=EDGE_LOOP('',(#23245,#23246,#23247,#23248));
#5310=EDGE_LOOP('',(#23249,#23250,#23251,#23252));
#5311=EDGE_LOOP('',(#23253,#23254,#23255,#23256));
#5312=EDGE_LOOP('',(#23257,#23258,#23259,#23260,#23261,#23262,#23263,#23264,
#23265));
#5313=EDGE_LOOP('',(#23266,#23267,#23268,#23269));
#5314=EDGE_LOOP('',(#23270,#23271,#23272,#23273));
#5315=EDGE_LOOP('',(#23274,#23275,#23276));
#5316=EDGE_LOOP('',(#23277,#23278,#23279,#23280));
#5317=EDGE_LOOP('',(#23281,#23282,#23283));
#5318=EDGE_LOOP('',(#23284,#23285,#23286,#23287));
#5319=EDGE_LOOP('',(#23288,#23289,#23290));
#5320=EDGE_LOOP('',(#23291,#23292,#23293,#23294));
#5321=EDGE_LOOP('',(#23295,#23296,#23297));
#5322=EDGE_LOOP('',(#23298,#23299,#23300,#23301));
#5323=EDGE_LOOP('',(#23302,#23303,#23304));
#5324=EDGE_LOOP('',(#23305,#23306,#23307,#23308));
#5325=EDGE_LOOP('',(#23309,#23310,#23311));
#5326=EDGE_LOOP('',(#23312,#23313,#23314,#23315));
#5327=EDGE_LOOP('',(#23316,#23317,#23318));
#5328=EDGE_LOOP('',(#23319,#23320,#23321,#23322));
#5329=EDGE_LOOP('',(#23323,#23324,#23325));
#5330=EDGE_LOOP('',(#23326,#23327,#23328,#23329));
#5331=EDGE_LOOP('',(#23330,#23331,#23332));
#5332=EDGE_LOOP('',(#23333,#23334,#23335,#23336));
#5333=EDGE_LOOP('',(#23337,#23338,#23339));
#5334=EDGE_LOOP('',(#23340,#23341,#23342,#23343));
#5335=EDGE_LOOP('',(#23344,#23345,#23346));
#5336=EDGE_LOOP('',(#23347,#23348,#23349,#23350));
#5337=EDGE_LOOP('',(#23351,#23352,#23353));
#5338=EDGE_LOOP('',(#23354,#23355,#23356,#23357));
#5339=EDGE_LOOP('',(#23358,#23359,#23360));
#5340=EDGE_LOOP('',(#23361,#23362,#23363,#23364));
#5341=EDGE_LOOP('',(#23365,#23366,#23367));
#5342=EDGE_LOOP('',(#23368,#23369,#23370,#23371));
#5343=EDGE_LOOP('',(#23372,#23373,#23374));
#5344=EDGE_LOOP('',(#23375,#23376,#23377,#23378));
#5345=EDGE_LOOP('',(#23379,#23380,#23381));
#5346=EDGE_LOOP('',(#23382,#23383,#23384,#23385));
#5347=EDGE_LOOP('',(#23386,#23387,#23388));
#5348=EDGE_LOOP('',(#23389,#23390,#23391,#23392));
#5349=EDGE_LOOP('',(#23393,#23394,#23395,#23396,#23397,#23398,#23399,#23400,
#23401,#23402));
#5350=EDGE_LOOP('',(#23403,#23404,#23405,#23406));
#5351=EDGE_LOOP('',(#23407,#23408,#23409,#23410,#23411,#23412,#23413,#23414,
#23415,#23416));
#5352=EDGE_LOOP('',(#23417,#23418,#23419,#23420));
#5353=EDGE_LOOP('',(#23421,#23422,#23423,#23424));
#5354=EDGE_LOOP('',(#23425,#23426,#23427,#23428));
#5355=EDGE_LOOP('',(#23429,#23430,#23431,#23432));
#5356=EDGE_LOOP('',(#23433,#23434,#23435,#23436));
#5357=EDGE_LOOP('',(#23437));
#5358=EDGE_LOOP('',(#23438));
#5359=EDGE_LOOP('',(#23439));
#5360=EDGE_LOOP('',(#23440));
#5361=EDGE_LOOP('',(#23441));
#5362=EDGE_LOOP('',(#23442));
#5363=EDGE_LOOP('',(#23443));
#5364=EDGE_LOOP('',(#23444));
#5365=EDGE_LOOP('',(#23445));
#5366=EDGE_LOOP('',(#23446));
#5367=EDGE_LOOP('',(#23447));
#5368=EDGE_LOOP('',(#23448));
#5369=EDGE_LOOP('',(#23449));
#5370=EDGE_LOOP('',(#23450));
#5371=EDGE_LOOP('',(#23451));
#5372=EDGE_LOOP('',(#23452));
#5373=EDGE_LOOP('',(#23453));
#5374=EDGE_LOOP('',(#23454,#23455,#23456,#23457));
#5375=EDGE_LOOP('',(#23458,#23459,#23460,#23461));
#5376=EDGE_LOOP('',(#23462,#23463,#23464,#23465));
#5377=EDGE_LOOP('',(#23466,#23467,#23468,#23469));
#5378=EDGE_LOOP('',(#23470,#23471,#23472,#23473));
#5379=EDGE_LOOP('',(#23474,#23475,#23476,#23477,#23478));
#5380=EDGE_LOOP('',(#23479,#23480,#23481,#23482,#23483));
#5381=EDGE_LOOP('',(#23484));
#5382=EDGE_LOOP('',(#23485));
#5383=EDGE_LOOP('',(#23486,#23487,#23488,#23489,#23490,#23491));
#5384=EDGE_LOOP('',(#23492));
#5385=EDGE_LOOP('',(#23493));
#5386=EDGE_LOOP('',(#23494,#23495,#23496,#23497));
#5387=EDGE_LOOP('',(#23498,#23499,#23500,#23501));
#5388=EDGE_LOOP('',(#23502,#23503,#23504,#23505));
#5389=EDGE_LOOP('',(#23506,#23507,#23508,#23509));
#5390=EDGE_LOOP('',(#23510,#23511,#23512,#23513));
#5391=EDGE_LOOP('',(#23514,#23515,#23516,#23517));
#5392=EDGE_LOOP('',(#23518,#23519,#23520,#23521,#23522,#23523));
#5393=EDGE_LOOP('',(#23524,#23525,#23526,#23527,#23528));
#5394=EDGE_LOOP('',(#23529,#23530,#23531,#23532,#23533,#23534,#23535,#23536,
#23537));
#5395=EDGE_LOOP('',(#23538,#23539,#23540,#23541,#23542));
#5396=EDGE_LOOP('',(#23543,#23544,#23545,#23546));
#5397=EDGE_LOOP('',(#23547,#23548,#23549,#23550));
#5398=EDGE_LOOP('',(#23551));
#5399=EDGE_LOOP('',(#23552,#23553,#23554,#23555,#23556,#23557));
#5400=EDGE_LOOP('',(#23558));
#5401=EDGE_LOOP('',(#23559));
#5402=EDGE_LOOP('',(#23560));
#5403=EDGE_LOOP('',(#23561));
#5404=EDGE_LOOP('',(#23562));
#5405=EDGE_LOOP('',(#23563,#23564,#23565,#23566,#23567));
#5406=EDGE_LOOP('',(#23568,#23569,#23570,#23571,#23572));
#5407=EDGE_LOOP('',(#23573,#23574,#23575,#23576,#23577));
#5408=EDGE_LOOP('',(#23578,#23579,#23580,#23581,#23582));
#5409=EDGE_LOOP('',(#23583,#23584,#23585,#23586,#23587));
#5410=EDGE_LOOP('',(#23588,#23589,#23590,#23591,#23592));
#5411=EDGE_LOOP('',(#23593,#23594,#23595));
#5412=EDGE_LOOP('',(#23596,#23597,#23598,#23599));
#5413=EDGE_LOOP('',(#23600,#23601,#23602));
#5414=EDGE_LOOP('',(#23603,#23604,#23605));
#5415=EDGE_LOOP('',(#23606,#23607,#23608));
#5416=EDGE_LOOP('',(#23609,#23610,#23611));
#5417=EDGE_LOOP('',(#23612,#23613,#23614,#23615));
#5418=EDGE_LOOP('',(#23616,#23617,#23618,#23619));
#5419=EDGE_LOOP('',(#23620));
#5420=EDGE_LOOP('',(#23621));
#5421=EDGE_LOOP('',(#23622));
#5422=EDGE_LOOP('',(#23623));
#5423=EDGE_LOOP('',(#23624,#23625,#23626,#23627));
#5424=EDGE_LOOP('',(#23628,#23629,#23630,#23631));
#5425=EDGE_LOOP('',(#23632,#23633,#23634,#23635));
#5426=EDGE_LOOP('',(#23636,#23637,#23638,#23639));
#5427=EDGE_LOOP('',(#23640,#23641,#23642,#23643));
#5428=EDGE_LOOP('',(#23644,#23645,#23646,#23647));
#5429=EDGE_LOOP('',(#23648,#23649,#23650,#23651));
#5430=EDGE_LOOP('',(#23652,#23653,#23654,#23655));
#5431=EDGE_LOOP('',(#23656,#23657,#23658,#23659));
#5432=EDGE_LOOP('',(#23660,#23661,#23662,#23663));
#5433=EDGE_LOOP('',(#23664,#23665,#23666,#23667));
#5434=EDGE_LOOP('',(#23668,#23669,#23670,#23671));
#5435=EDGE_LOOP('',(#23672,#23673,#23674,#23675));
#5436=EDGE_LOOP('',(#23676,#23677,#23678,#23679));
#5437=EDGE_LOOP('',(#23680,#23681,#23682,#23683));
#5438=EDGE_LOOP('',(#23684,#23685,#23686,#23687));
#5439=EDGE_LOOP('',(#23688,#23689,#23690,#23691));
#5440=EDGE_LOOP('',(#23692));
#5441=EDGE_LOOP('',(#23693));
#5442=EDGE_LOOP('',(#23694));
#5443=EDGE_LOOP('',(#23695));
#5444=EDGE_LOOP('',(#23696));
#5445=EDGE_LOOP('',(#23697));
#5446=EDGE_LOOP('',(#23698));
#5447=EDGE_LOOP('',(#23699));
#5448=EDGE_LOOP('',(#23700));
#5449=EDGE_LOOP('',(#23701));
#5450=EDGE_LOOP('',(#23702,#23703,#23704,#23705));
#5451=EDGE_LOOP('',(#23706,#23707,#23708,#23709,#23710,#23711));
#5452=EDGE_LOOP('',(#23712,#23713,#23714,#23715));
#5453=EDGE_LOOP('',(#23716,#23717,#23718,#23719,#23720,#23721));
#5454=EDGE_LOOP('',(#23722,#23723,#23724,#23725));
#5455=EDGE_LOOP('',(#23726));
#5456=EDGE_LOOP('',(#23727));
#5457=EDGE_LOOP('',(#23728));
#5458=EDGE_LOOP('',(#23729));
#5459=EDGE_LOOP('',(#23730));
#5460=EDGE_LOOP('',(#23731));
#5461=EDGE_LOOP('',(#23732));
#5462=EDGE_LOOP('',(#23733));
#5463=EDGE_LOOP('',(#23734));
#5464=EDGE_LOOP('',(#23735));
#5465=EDGE_LOOP('',(#23736,#23737,#23738,#23739));
#5466=EDGE_LOOP('',(#23740,#23741,#23742,#23743));
#5467=EDGE_LOOP('',(#23744,#23745,#23746,#23747));
#5468=EDGE_LOOP('',(#23748,#23749,#23750,#23751));
#5469=EDGE_LOOP('',(#23752,#23753,#23754,#23755,#23756));
#5470=EDGE_LOOP('',(#23757,#23758,#23759,#23760,#23761));
#5471=EDGE_LOOP('',(#23762));
#5472=EDGE_LOOP('',(#23763));
#5473=EDGE_LOOP('',(#23764,#23765,#23766,#23767,#23768,#23769));
#5474=EDGE_LOOP('',(#23770));
#5475=EDGE_LOOP('',(#23771));
#5476=EDGE_LOOP('',(#23772,#23773,#23774,#23775));
#5477=EDGE_LOOP('',(#23776,#23777,#23778,#23779));
#5478=EDGE_LOOP('',(#23780,#23781,#23782,#23783));
#5479=EDGE_LOOP('',(#23784,#23785,#23786,#23787));
#5480=EDGE_LOOP('',(#23788,#23789,#23790,#23791));
#5481=EDGE_LOOP('',(#23792,#23793,#23794,#23795));
#5482=EDGE_LOOP('',(#23796,#23797,#23798,#23799,#23800,#23801));
#5483=LINE('',#36181,#7472);
#5484=LINE('',#36187,#7473);
#5485=LINE('',#36193,#7474);
#5486=LINE('',#36199,#7475);
#5487=LINE('',#36204,#7476);
#5488=LINE('',#36206,#7477);
#5489=LINE('',#36208,#7478);
#5490=LINE('',#36209,#7479);
#5491=LINE('',#36212,#7480);
#5492=LINE('',#36214,#7481);
#5493=LINE('',#36215,#7482);
#5494=LINE('',#36218,#7483);
#5495=LINE('',#36220,#7484);
#5496=LINE('',#36221,#7485);
#5497=LINE('',#36223,#7486);
#5498=LINE('',#36224,#7487);
#5499=LINE('',#36228,#7488);
#5500=LINE('',#36230,#7489);
#5501=LINE('',#36232,#7490);
#5502=LINE('',#36233,#7491);
#5503=LINE('',#36236,#7492);
#5504=LINE('',#36238,#7493);
#5505=LINE('',#36240,#7494);
#5506=LINE('',#36241,#7495);
#5507=LINE('',#36245,#7496);
#5508=LINE('',#36247,#7497);
#5509=LINE('',#36249,#7498);
#5510=LINE('',#36250,#7499);
#5511=LINE('',#36253,#7500);
#5512=LINE('',#36255,#7501);
#5513=LINE('',#36257,#7502);
#5514=LINE('',#36258,#7503);
#5515=LINE('',#36260,#7504);
#5516=LINE('',#36261,#7505);
#5517=LINE('',#36263,#7506);
#5518=LINE('',#36265,#7507);
#5519=LINE('',#36268,#7508);
#5520=LINE('',#36269,#7509);
#5521=LINE('',#36271,#7510);
#5522=LINE('',#36273,#7511);
#5523=LINE('',#36281,#7512);
#5524=LINE('',#36287,#7513);
#5525=LINE('',#36293,#7514);
#5526=LINE('',#36299,#7515);
#5527=LINE('',#36304,#7516);
#5528=LINE('',#36306,#7517);
#5529=LINE('',#36308,#7518);
#5530=LINE('',#36309,#7519);
#5531=LINE('',#36312,#7520);
#5532=LINE('',#36314,#7521);
#5533=LINE('',#36316,#7522);
#5534=LINE('',#36318,#7523);
#5535=LINE('',#36319,#7524);
#5536=LINE('',#36323,#7525);
#5537=LINE('',#36324,#7526);
#5538=LINE('',#36326,#7527);
#5539=LINE('',#36327,#7528);
#5540=LINE('',#36331,#7529);
#5541=LINE('',#36333,#7530);
#5542=LINE('',#36334,#7531);
#5543=LINE('',#36336,#7532);
#5544=LINE('',#36337,#7533);
#5545=LINE('',#36340,#7534);
#5546=LINE('',#36342,#7535);
#5547=LINE('',#36343,#7536);
#5548=LINE('',#36344,#7537);
#5549=LINE('',#36347,#7538);
#5550=LINE('',#36348,#7539);
#5551=LINE('',#36352,#7540);
#5552=LINE('',#36353,#7541);
#5553=LINE('',#36355,#7542);
#5554=LINE('',#36358,#7543);
#5555=LINE('',#36359,#7544);
#5556=LINE('',#36361,#7545);
#5557=LINE('',#36368,#7546);
#5558=LINE('',#36374,#7547);
#5559=LINE('',#36380,#7548);
#5560=LINE('',#36386,#7549);
#5561=LINE('',#36392,#7550);
#5562=LINE('',#36398,#7551);
#5563=LINE('',#36404,#7552);
#5564=LINE('',#36410,#7553);
#5565=LINE('',#36416,#7554);
#5566=LINE('',#36422,#7555);
#5567=LINE('',#36428,#7556);
#5568=LINE('',#36434,#7557);
#5569=LINE('',#36439,#7558);
#5570=LINE('',#36441,#7559);
#5571=LINE('',#36443,#7560);
#5572=LINE('',#36444,#7561);
#5573=LINE('',#36447,#7562);
#5574=LINE('',#36449,#7563);
#5575=LINE('',#36450,#7564);
#5576=LINE('',#36453,#7565);
#5577=LINE('',#36454,#7566);
#5578=LINE('',#36457,#7567);
#5579=LINE('',#36458,#7568);
#5580=LINE('',#36460,#7569);
#5581=LINE('',#36471,#7570);
#5582=LINE('',#36477,#7571);
#5583=LINE('',#36483,#7572);
#5584=LINE('',#36489,#7573);
#5585=LINE('',#36495,#7574);
#5586=LINE('',#36501,#7575);
#5587=LINE('',#36507,#7576);
#5588=LINE('',#36512,#7577);
#5589=LINE('',#36516,#7578);
#5590=LINE('',#36518,#7579);
#5591=LINE('',#36520,#7580);
#5592=LINE('',#36525,#7581);
#5593=LINE('',#36526,#7582);
#5594=LINE('',#36527,#7583);
#5595=LINE('',#36531,#7584);
#5596=LINE('',#36536,#7585);
#5597=LINE('',#36537,#7586);
#5598=LINE('',#36539,#7587);
#5599=LINE('',#36540,#7588);
#5600=LINE('',#36542,#7589);
#5601=LINE('',#36544,#7590);
#5602=LINE('',#36552,#7591);
#5603=LINE('',#36558,#7592);
#5604=LINE('',#36564,#7593);
#5605=LINE('',#36570,#7594);
#5606=LINE('',#36576,#7595);
#5607=LINE('',#36582,#7596);
#5608=LINE('',#36587,#7597);
#5609=LINE('',#36589,#7598);
#5610=LINE('',#36591,#7599);
#5611=LINE('',#36592,#7600);
#5612=LINE('',#36595,#7601);
#5613=LINE('',#36597,#7602);
#5614=LINE('',#36598,#7603);
#5615=LINE('',#36601,#7604);
#5616=LINE('',#36603,#7605);
#5617=LINE('',#36604,#7606);
#5618=LINE('',#36606,#7607);
#5619=LINE('',#36607,#7608);
#5620=LINE('',#36617,#7609);
#5621=LINE('',#36623,#7610);
#5622=LINE('',#36629,#7611);
#5623=LINE('',#36635,#7612);
#5624=LINE('',#36641,#7613);
#5625=LINE('',#36647,#7614);
#5626=LINE('',#36652,#7615);
#5627=LINE('',#36654,#7616);
#5628=LINE('',#36656,#7617);
#5629=LINE('',#36657,#7618);
#5630=LINE('',#36660,#7619);
#5631=LINE('',#36662,#7620);
#5632=LINE('',#36663,#7621);
#5633=LINE('',#36666,#7622);
#5634=LINE('',#36668,#7623);
#5635=LINE('',#36669,#7624);
#5636=LINE('',#36671,#7625);
#5637=LINE('',#36672,#7626);
#5638=LINE('',#36681,#7627);
#5639=LINE('',#36696,#7628);
#5640=LINE('',#36709,#7629);
#5641=LINE('',#36724,#7630);
#5642=LINE('',#36737,#7631);
#5643=LINE('',#36752,#7632);
#5644=LINE('',#36765,#7633);
#5645=LINE('',#36780,#7634);
#5646=LINE('',#36793,#7635);
#5647=LINE('',#36808,#7636);
#5648=LINE('',#36821,#7637);
#5649=LINE('',#36836,#7638);
#5650=LINE('',#36849,#7639);
#5651=LINE('',#36864,#7640);
#5652=LINE('',#36877,#7641);
#5653=LINE('',#36892,#7642);
#5654=LINE('',#36905,#7643);
#5655=LINE('',#36920,#7644);
#5656=LINE('',#36933,#7645);
#5657=LINE('',#36948,#7646);
#5658=LINE('',#36961,#7647);
#5659=LINE('',#36976,#7648);
#5660=LINE('',#36989,#7649);
#5661=LINE('',#37004,#7650);
#5662=LINE('',#37017,#7651);
#5663=LINE('',#37032,#7652);
#5664=LINE('',#37045,#7653);
#5665=LINE('',#37060,#7654);
#5666=LINE('',#37073,#7655);
#5667=LINE('',#37088,#7656);
#5668=LINE('',#37099,#7657);
#5669=LINE('',#37101,#7658);
#5670=LINE('',#37102,#7659);
#5671=LINE('',#37104,#7660);
#5672=LINE('',#37105,#7661);
#5673=LINE('',#37107,#7662);
#5674=LINE('',#37108,#7663);
#5675=LINE('',#37109,#7664);
#5676=LINE('',#37110,#7665);
#5677=LINE('',#37111,#7666);
#5678=LINE('',#37112,#7667);
#5679=LINE('',#37113,#7668);
#5680=LINE('',#37114,#7669);
#5681=LINE('',#37115,#7670);
#5682=LINE('',#37116,#7671);
#5683=LINE('',#37117,#7672);
#5684=LINE('',#37118,#7673);
#5685=LINE('',#37119,#7674);
#5686=LINE('',#37120,#7675);
#5687=LINE('',#37122,#7676);
#5688=LINE('',#37124,#7677);
#5689=LINE('',#37126,#7678);
#5690=LINE('',#37127,#7679);
#5691=LINE('',#37129,#7680);
#5692=LINE('',#37132,#7681);
#5693=LINE('',#37134,#7682);
#5694=LINE('',#37136,#7683);
#5695=LINE('',#37138,#7684);
#5696=LINE('',#37139,#7685);
#5697=LINE('',#37140,#7686);
#5698=LINE('',#37141,#7687);
#5699=LINE('',#37142,#7688);
#5700=LINE('',#37143,#7689);
#5701=LINE('',#37144,#7690);
#5702=LINE('',#37145,#7691);
#5703=LINE('',#37146,#7692);
#5704=LINE('',#37147,#7693);
#5705=LINE('',#37148,#7694);
#5706=LINE('',#37149,#7695);
#5707=LINE('',#37150,#7696);
#5708=LINE('',#37151,#7697);
#5709=LINE('',#37152,#7698);
#5710=LINE('',#37155,#7699);
#5711=LINE('',#37156,#7700);
#5712=LINE('',#37160,#7701);
#5713=LINE('',#37161,#7702);
#5714=LINE('',#37165,#7703);
#5715=LINE('',#37166,#7704);
#5716=LINE('',#37170,#7705);
#5717=LINE('',#37171,#7706);
#5718=LINE('',#37175,#7707);
#5719=LINE('',#37176,#7708);
#5720=LINE('',#37180,#7709);
#5721=LINE('',#37181,#7710);
#5722=LINE('',#37185,#7711);
#5723=LINE('',#37186,#7712);
#5724=LINE('',#37190,#7713);
#5725=LINE('',#37191,#7714);
#5726=LINE('',#37195,#7715);
#5727=LINE('',#37196,#7716);
#5728=LINE('',#37199,#7717);
#5729=LINE('',#37200,#7718);
#5730=LINE('',#37205,#7719);
#5731=LINE('',#37206,#7720);
#5732=LINE('',#37210,#7721);
#5733=LINE('',#37211,#7722);
#5734=LINE('',#37214,#7723);
#5735=LINE('',#37215,#7724);
#5736=LINE('',#37220,#7725);
#5737=LINE('',#37222,#7726);
#5738=LINE('',#37223,#7727);
#5739=LINE('',#37226,#7728);
#5740=LINE('',#37229,#7729);
#5741=LINE('',#37231,#7730);
#5742=LINE('',#37235,#7731);
#5743=LINE('',#37239,#7732);
#5744=LINE('',#37243,#7733);
#5745=LINE('',#37251,#7734);
#5746=LINE('',#37255,#7735);
#5747=LINE('',#37259,#7736);
#5748=LINE('',#37267,#7737);
#5749=LINE('',#37269,#7738);
#5750=LINE('',#37271,#7739);
#5751=LINE('',#37279,#7740);
#5752=LINE('',#37283,#7741);
#5753=LINE('',#37287,#7742);
#5754=LINE('',#37295,#7743);
#5755=LINE('',#37299,#7744);
#5756=LINE('',#37303,#7745);
#5757=LINE('',#37307,#7746);
#5758=LINE('',#37308,#7747);
#5759=LINE('',#37310,#7748);
#5760=LINE('',#37311,#7749);
#5761=LINE('',#37313,#7750);
#5762=LINE('',#37315,#7751);
#5763=LINE('',#37317,#7752);
#5764=LINE('',#37321,#7753);
#5765=LINE('',#37325,#7754);
#5766=LINE('',#37329,#7755);
#5767=LINE('',#37337,#7756);
#5768=LINE('',#37341,#7757);
#5769=LINE('',#37345,#7758);
#5770=LINE('',#37353,#7759);
#5771=LINE('',#37355,#7760);
#5772=LINE('',#37357,#7761);
#5773=LINE('',#37365,#7762);
#5774=LINE('',#37369,#7763);
#5775=LINE('',#37373,#7764);
#5776=LINE('',#37381,#7765);
#5777=LINE('',#37385,#7766);
#5778=LINE('',#37389,#7767);
#5779=LINE('',#37393,#7768);
#5780=LINE('',#37394,#7769);
#5781=LINE('',#37396,#7770);
#5782=LINE('',#37397,#7771);
#5783=LINE('',#37399,#7772);
#5784=LINE('',#37400,#7773);
#5785=LINE('',#37402,#7774);
#5786=LINE('',#37403,#7775);
#5787=LINE('',#37405,#7776);
#5788=LINE('',#37406,#7777);
#5789=LINE('',#37408,#7778);
#5790=LINE('',#37409,#7779);
#5791=LINE('',#37411,#7780);
#5792=LINE('',#37412,#7781);
#5793=LINE('',#37414,#7782);
#5794=LINE('',#37416,#7783);
#5795=LINE('',#37418,#7784);
#5796=LINE('',#37420,#7785);
#5797=LINE('',#37421,#7786);
#5798=LINE('',#37423,#7787);
#5799=LINE('',#37424,#7788);
#5800=LINE('',#37426,#7789);
#5801=LINE('',#37427,#7790);
#5802=LINE('',#37429,#7791);
#5803=LINE('',#37430,#7792);
#5804=LINE('',#37432,#7793);
#5805=LINE('',#37434,#7794);
#5806=LINE('',#37435,#7795);
#5807=LINE('',#37437,#7796);
#5808=LINE('',#37438,#7797);
#5809=LINE('',#37449,#7798);
#5810=LINE('',#37450,#7799);
#5811=LINE('',#37452,#7800);
#5812=LINE('',#37453,#7801);
#5813=LINE('',#37455,#7802);
#5814=LINE('',#37456,#7803);
#5815=LINE('',#37458,#7804);
#5816=LINE('',#37459,#7805);
#5817=LINE('',#37462,#7806);
#5818=LINE('',#37463,#7807);
#5819=LINE('',#37465,#7808);
#5820=LINE('',#37466,#7809);
#5821=LINE('',#37478,#7810);
#5822=LINE('',#37500,#7811);
#5823=LINE('',#37506,#7812);
#5824=LINE('',#37512,#7813);
#5825=LINE('',#37516,#7814);
#5826=LINE('',#37519,#7815);
#5827=LINE('',#37524,#7816);
#5828=LINE('',#37530,#7817);
#5829=LINE('',#37536,#7818);
#5830=LINE('',#37542,#7819);
#5831=LINE('',#37548,#7820);
#5832=LINE('',#37554,#7821);
#5833=LINE('',#37560,#7822);
#5834=LINE('',#37566,#7823);
#5835=LINE('',#37570,#7824);
#5836=LINE('',#37573,#7825);
#5837=LINE('',#37576,#7826);
#5838=LINE('',#37579,#7827);
#5839=LINE('',#37584,#7828);
#5840=LINE('',#37586,#7829);
#5841=LINE('',#37590,#7830);
#5842=LINE('',#37695,#7831);
#5843=LINE('',#37700,#7832);
#5844=LINE('',#37707,#7833);
#5845=LINE('',#37709,#7834);
#5846=LINE('',#37710,#7835);
#5847=LINE('',#37715,#7836);
#5848=LINE('',#37718,#7837);
#5849=LINE('',#37724,#7838);
#5850=LINE('',#37727,#7839);
#5851=LINE('',#37732,#7840);
#5852=LINE('',#37734,#7841);
#5853=LINE('',#37735,#7842);
#5854=LINE('',#37739,#7843);
#5855=LINE('',#37741,#7844);
#5856=LINE('',#37743,#7845);
#5857=LINE('',#37744,#7846);
#5858=LINE('',#37748,#7847);
#5859=LINE('',#37750,#7848);
#5860=LINE('',#37752,#7849);
#5861=LINE('',#37753,#7850);
#5862=LINE('',#37757,#7851);
#5863=LINE('',#37759,#7852);
#5864=LINE('',#37761,#7853);
#5865=LINE('',#37762,#7854);
#5866=LINE('',#37766,#7855);
#5867=LINE('',#37768,#7856);
#5868=LINE('',#37770,#7857);
#5869=LINE('',#37771,#7858);
#5870=LINE('',#37775,#7859);
#5871=LINE('',#37777,#7860);
#5872=LINE('',#37779,#7861);
#5873=LINE('',#37780,#7862);
#5874=LINE('',#37784,#7863);
#5875=LINE('',#37786,#7864);
#5876=LINE('',#37788,#7865);
#5877=LINE('',#37789,#7866);
#5878=LINE('',#37793,#7867);
#5879=LINE('',#37795,#7868);
#5880=LINE('',#37797,#7869);
#5881=LINE('',#37798,#7870);
#5882=LINE('',#37802,#7871);
#5883=LINE('',#37804,#7872);
#5884=LINE('',#37806,#7873);
#5885=LINE('',#37807,#7874);
#5886=LINE('',#37811,#7875);
#5887=LINE('',#37813,#7876);
#5888=LINE('',#37815,#7877);
#5889=LINE('',#37816,#7878);
#5890=LINE('',#37819,#7879);
#5891=LINE('',#37821,#7880);
#5892=LINE('',#37822,#7881);
#5893=LINE('',#37826,#7882);
#5894=LINE('',#37828,#7883);
#5895=LINE('',#37830,#7884);
#5896=LINE('',#37831,#7885);
#5897=LINE('',#37834,#7886);
#5898=LINE('',#37836,#7887);
#5899=LINE('',#37837,#7888);
#5900=LINE('',#37841,#7889);
#5901=LINE('',#37843,#7890);
#5902=LINE('',#37845,#7891);
#5903=LINE('',#37846,#7892);
#5904=LINE('',#37850,#7893);
#5905=LINE('',#37852,#7894);
#5906=LINE('',#37854,#7895);
#5907=LINE('',#37855,#7896);
#5908=LINE('',#37859,#7897);
#5909=LINE('',#37861,#7898);
#5910=LINE('',#37863,#7899);
#5911=LINE('',#37864,#7900);
#5912=LINE('',#37868,#7901);
#5913=LINE('',#37870,#7902);
#5914=LINE('',#37872,#7903);
#5915=LINE('',#37873,#7904);
#5916=LINE('',#37875,#7905);
#5917=LINE('',#37876,#7906);
#5918=LINE('',#37882,#7907);
#5919=LINE('',#37885,#7908);
#5920=LINE('',#37891,#7909);
#5921=LINE('',#37894,#7910);
#5922=LINE('',#37900,#7911);
#5923=LINE('',#37903,#7912);
#5924=LINE('',#37909,#7913);
#5925=LINE('',#37912,#7914);
#5926=LINE('',#37965,#7915);
#5927=LINE('',#37967,#7916);
#5928=LINE('',#37969,#7917);
#5929=LINE('',#37970,#7918);
#5930=LINE('',#37973,#7919);
#5931=LINE('',#37975,#7920);
#5932=LINE('',#37976,#7921);
#5933=LINE('',#37978,#7922);
#5934=LINE('',#37980,#7923);
#5935=LINE('',#37981,#7924);
#5936=LINE('',#37984,#7925);
#5937=LINE('',#37985,#7926);
#5938=LINE('',#37988,#7927);
#5939=LINE('',#37989,#7928);
#5940=LINE('',#37991,#7929);
#5941=LINE('',#37994,#7930);
#5942=LINE('',#37995,#7931);
#5943=LINE('',#37998,#7932);
#5944=LINE('',#37999,#7933);
#5945=LINE('',#38001,#7934);
#5946=LINE('',#38004,#7935);
#5947=LINE('',#38006,#7936);
#5948=LINE('',#38007,#7937);
#5949=LINE('',#38010,#7938);
#5950=LINE('',#38011,#7939);
#5951=LINE('',#38014,#7940);
#5952=LINE('',#38015,#7941);
#5953=LINE('',#38018,#7942);
#5954=LINE('',#38019,#7943);
#5955=LINE('',#38022,#7944);
#5956=LINE('',#38023,#7945);
#5957=LINE('',#38025,#7946);
#5958=LINE('',#38030,#7947);
#5959=LINE('',#38034,#7948);
#5960=LINE('',#38038,#7949);
#5961=LINE('',#38046,#7950);
#5962=LINE('',#38050,#7951);
#5963=LINE('',#38054,#7952);
#5964=LINE('',#38062,#7953);
#5965=LINE('',#38064,#7954);
#5966=LINE('',#38066,#7955);
#5967=LINE('',#38074,#7956);
#5968=LINE('',#38078,#7957);
#5969=LINE('',#38082,#7958);
#5970=LINE('',#38090,#7959);
#5971=LINE('',#38094,#7960);
#5972=LINE('',#38098,#7961);
#5973=LINE('',#38100,#7962);
#5974=LINE('',#38102,#7963);
#5975=LINE('',#38104,#7964);
#5976=LINE('',#38106,#7965);
#5977=LINE('',#38108,#7966);
#5978=LINE('',#38110,#7967);
#5979=LINE('',#38112,#7968);
#5980=LINE('',#38114,#7969);
#5981=LINE('',#38115,#7970);
#5982=LINE('',#38119,#7971);
#5983=LINE('',#38120,#7972);
#5984=LINE('',#38121,#7973);
#5985=LINE('',#38125,#7974);
#5986=LINE('',#38128,#7975);
#5987=LINE('',#38129,#7976);
#5988=LINE('',#38133,#7977);
#5989=LINE('',#38136,#7978);
#5990=LINE('',#38137,#7979);
#5991=LINE('',#38141,#7980);
#5992=LINE('',#38145,#7981);
#5993=LINE('',#38149,#7982);
#5994=LINE('',#38152,#7983);
#5995=LINE('',#38153,#7984);
#5996=LINE('',#38157,#7985);
#5997=LINE('',#38160,#7986);
#5998=LINE('',#38161,#7987);
#5999=LINE('',#38165,#7988);
#6000=LINE('',#38168,#7989);
#6001=LINE('',#38169,#7990);
#6002=LINE('',#38173,#7991);
#6003=LINE('',#38177,#7992);
#6004=LINE('',#38181,#7993);
#6005=LINE('',#38184,#7994);
#6006=LINE('',#38185,#7995);
#6007=LINE('',#38188,#7996);
#6008=LINE('',#38189,#7997);
#6009=LINE('',#38192,#7998);
#6010=LINE('',#38193,#7999);
#6011=LINE('',#38197,#8000);
#6012=LINE('',#38201,#8001);
#6013=LINE('',#38205,#8002);
#6014=LINE('',#38208,#8003);
#6015=LINE('',#38209,#8004);
#6016=LINE('',#38213,#8005);
#6017=LINE('',#38216,#8006);
#6018=LINE('',#38217,#8007);
#6019=LINE('',#38221,#8008);
#6020=LINE('',#38224,#8009);
#6021=LINE('',#38225,#8010);
#6022=LINE('',#38229,#8011);
#6023=LINE('',#38233,#8012);
#6024=LINE('',#38237,#8013);
#6025=LINE('',#38240,#8014);
#6026=LINE('',#38241,#8015);
#6027=LINE('',#38245,#8016);
#6028=LINE('',#38248,#8017);
#6029=LINE('',#38249,#8018);
#6030=LINE('',#38253,#8019);
#6031=LINE('',#38256,#8020);
#6032=LINE('',#38257,#8021);
#6033=LINE('',#38260,#8022);
#6034=LINE('',#38261,#8023);
#6035=LINE('',#38264,#8024);
#6036=LINE('',#38265,#8025);
#6037=LINE('',#38268,#8026);
#6038=LINE('',#38269,#8027);
#6039=LINE('',#38272,#8028);
#6040=LINE('',#38273,#8029);
#6041=LINE('',#38276,#8030);
#6042=LINE('',#38277,#8031);
#6043=LINE('',#38280,#8032);
#6044=LINE('',#38281,#8033);
#6045=LINE('',#38284,#8034);
#6046=LINE('',#38285,#8035);
#6047=LINE('',#38288,#8036);
#6048=LINE('',#38289,#8037);
#6049=LINE('',#38291,#8038);
#6050=LINE('',#38295,#8039);
#6051=LINE('',#38298,#8040);
#6052=LINE('',#38302,#8041);
#6053=LINE('',#38304,#8042);
#6054=LINE('',#38308,#8043);
#6055=LINE('',#38310,#8044);
#6056=LINE('',#38312,#8045);
#6057=LINE('',#38314,#8046);
#6058=LINE('',#38316,#8047);
#6059=LINE('',#38318,#8048);
#6060=LINE('',#38320,#8049);
#6061=LINE('',#38324,#8050);
#6062=LINE('',#38328,#8051);
#6063=LINE('',#38336,#8052);
#6064=LINE('',#38340,#8053);
#6065=LINE('',#38344,#8054);
#6066=LINE('',#38352,#8055);
#6067=LINE('',#38354,#8056);
#6068=LINE('',#38356,#8057);
#6069=LINE('',#38364,#8058);
#6070=LINE('',#38368,#8059);
#6071=LINE('',#38372,#8060);
#6072=LINE('',#38380,#8061);
#6073=LINE('',#38384,#8062);
#6074=LINE('',#38388,#8063);
#6075=LINE('',#38390,#8064);
#6076=LINE('',#38392,#8065);
#6077=LINE('',#38394,#8066);
#6078=LINE('',#38395,#8067);
#6079=LINE('',#38398,#8068);
#6080=LINE('',#38399,#8069);
#6081=LINE('',#38402,#8070);
#6082=LINE('',#38403,#8071);
#6083=LINE('',#38409,#8072);
#6084=LINE('',#38412,#8073);
#6085=LINE('',#38416,#8074);
#6086=LINE('',#38417,#8075);
#6087=LINE('',#38418,#8076);
#6088=LINE('',#38421,#8077);
#6089=LINE('',#38422,#8078);
#6090=LINE('',#38425,#8079);
#6091=LINE('',#38426,#8080);
#6092=LINE('',#38429,#8081);
#6093=LINE('',#38430,#8082);
#6094=LINE('',#38434,#8083);
#6095=LINE('',#38435,#8084);
#6096=LINE('',#38437,#8085);
#6097=LINE('',#38438,#8086);
#6098=LINE('',#38439,#8087);
#6099=LINE('',#38442,#8088);
#6100=LINE('',#38443,#8089);
#6101=LINE('',#38446,#8090);
#6102=LINE('',#38447,#8091);
#6103=LINE('',#38450,#8092);
#6104=LINE('',#38451,#8093);
#6105=LINE('',#38454,#8094);
#6106=LINE('',#38455,#8095);
#6107=LINE('',#38458,#8096);
#6108=LINE('',#38459,#8097);
#6109=LINE('',#38463,#8098);
#6110=LINE('',#38466,#8099);
#6111=LINE('',#38467,#8100);
#6112=LINE('',#38471,#8101);
#6113=LINE('',#38474,#8102);
#6114=LINE('',#38475,#8103);
#6115=LINE('',#38479,#8104);
#6116=LINE('',#38483,#8105);
#6117=LINE('',#38487,#8106);
#6118=LINE('',#38490,#8107);
#6119=LINE('',#38491,#8108);
#6120=LINE('',#38495,#8109);
#6121=LINE('',#38498,#8110);
#6122=LINE('',#38499,#8111);
#6123=LINE('',#38503,#8112);
#6124=LINE('',#38506,#8113);
#6125=LINE('',#38507,#8114);
#6126=LINE('',#38511,#8115);
#6127=LINE('',#38515,#8116);
#6128=LINE('',#38519,#8117);
#6129=LINE('',#38522,#8118);
#6130=LINE('',#38523,#8119);
#6131=LINE('',#38526,#8120);
#6132=LINE('',#38527,#8121);
#6133=LINE('',#38530,#8122);
#6134=LINE('',#38531,#8123);
#6135=LINE('',#38535,#8124);
#6136=LINE('',#38539,#8125);
#6137=LINE('',#38543,#8126);
#6138=LINE('',#38546,#8127);
#6139=LINE('',#38547,#8128);
#6140=LINE('',#38551,#8129);
#6141=LINE('',#38554,#8130);
#6142=LINE('',#38555,#8131);
#6143=LINE('',#38559,#8132);
#6144=LINE('',#38562,#8133);
#6145=LINE('',#38563,#8134);
#6146=LINE('',#38567,#8135);
#6147=LINE('',#38571,#8136);
#6148=LINE('',#38575,#8137);
#6149=LINE('',#38578,#8138);
#6150=LINE('',#38579,#8139);
#6151=LINE('',#38583,#8140);
#6152=LINE('',#38586,#8141);
#6153=LINE('',#38587,#8142);
#6154=LINE('',#38591,#8143);
#6155=LINE('',#38593,#8144);
#6156=LINE('',#38598,#8145);
#6157=LINE('',#38600,#8146);
#6158=LINE('',#38602,#8147);
#6159=LINE('',#38603,#8148);
#6160=LINE('',#38607,#8149);
#6161=LINE('',#38609,#8150);
#6162=LINE('',#38611,#8151);
#6163=LINE('',#38612,#8152);
#6164=LINE('',#38615,#8153);
#6165=LINE('',#38616,#8154);
#6166=LINE('',#38619,#8155);
#6167=LINE('',#38620,#8156);
#6168=LINE('',#38628,#8157);
#6169=LINE('',#38631,#8158);
#6170=LINE('',#38633,#8159);
#6171=LINE('',#38635,#8160);
#6172=LINE('',#38636,#8161);
#6173=LINE('',#38639,#8162);
#6174=LINE('',#38641,#8163);
#6175=LINE('',#38642,#8164);
#6176=LINE('',#38646,#8165);
#6177=LINE('',#38648,#8166);
#6178=LINE('',#38650,#8167);
#6179=LINE('',#38651,#8168);
#6180=LINE('',#38654,#8169);
#6181=LINE('',#38657,#8170);
#6182=LINE('',#38658,#8171);
#6183=LINE('',#38661,#8172);
#6184=LINE('',#38666,#8173);
#6185=LINE('',#38668,#8174);
#6186=LINE('',#38670,#8175);
#6187=LINE('',#38672,#8176);
#6188=LINE('',#38674,#8177);
#6189=LINE('',#38676,#8178);
#6190=LINE('',#38678,#8179);
#6191=LINE('',#38680,#8180);
#6192=LINE('',#38682,#8181);
#6193=LINE('',#38684,#8182);
#6194=LINE('',#38688,#8183);
#6195=LINE('',#38692,#8184);
#6196=LINE('',#38700,#8185);
#6197=LINE('',#38704,#8186);
#6198=LINE('',#38708,#8187);
#6199=LINE('',#38716,#8188);
#6200=LINE('',#38718,#8189);
#6201=LINE('',#38720,#8190);
#6202=LINE('',#38728,#8191);
#6203=LINE('',#38732,#8192);
#6204=LINE('',#38736,#8193);
#6205=LINE('',#38744,#8194);
#6206=LINE('',#38748,#8195);
#6207=LINE('',#38751,#8196);
#6208=LINE('',#38754,#8197);
#6209=LINE('',#38755,#8198);
#6210=LINE('',#38758,#8199);
#6211=LINE('',#38759,#8200);
#6212=LINE('',#38763,#8201);
#6213=LINE('',#38764,#8202);
#6214=LINE('',#38765,#8203);
#6215=LINE('',#38768,#8204);
#6216=LINE('',#38770,#8205);
#6217=LINE('',#38771,#8206);
#6218=LINE('',#38774,#8207);
#6219=LINE('',#38776,#8208);
#6220=LINE('',#38777,#8209);
#6221=LINE('',#38780,#8210);
#6222=LINE('',#38782,#8211);
#6223=LINE('',#38783,#8212);
#6224=LINE('',#38792,#8213);
#6225=LINE('',#38794,#8214);
#6226=LINE('',#38795,#8215);
#6227=LINE('',#38799,#8216);
#6228=LINE('',#38800,#8217);
#6229=LINE('',#38801,#8218);
#6230=LINE('',#38806,#8219);
#6231=LINE('',#38807,#8220);
#6232=LINE('',#38811,#8221);
#6233=LINE('',#38812,#8222);
#6234=LINE('',#38813,#8223);
#6235=LINE('',#38816,#8224);
#6236=LINE('',#38817,#8225);
#6237=LINE('',#38823,#8226);
#6238=LINE('',#38824,#8227);
#6239=LINE('',#38831,#8228);
#6240=LINE('',#38832,#8229);
#6241=LINE('',#38833,#8230);
#6242=LINE('',#38836,#8231);
#6243=LINE('',#38837,#8232);
#6244=LINE('',#38840,#8233);
#6245=LINE('',#38841,#8234);
#6246=LINE('',#38844,#8235);
#6247=LINE('',#38845,#8236);
#6248=LINE('',#38848,#8237);
#6249=LINE('',#38849,#8238);
#6250=LINE('',#38852,#8239);
#6251=LINE('',#38853,#8240);
#6252=LINE('',#38856,#8241);
#6253=LINE('',#38857,#8242);
#6254=LINE('',#38860,#8243);
#6255=LINE('',#38861,#8244);
#6256=LINE('',#38864,#8245);
#6257=LINE('',#38865,#8246);
#6258=LINE('',#38868,#8247);
#6259=LINE('',#38869,#8248);
#6260=LINE('',#38873,#8249);
#6261=LINE('',#38876,#8250);
#6262=LINE('',#38877,#8251);
#6263=LINE('',#38881,#8252);
#6264=LINE('',#38884,#8253);
#6265=LINE('',#38885,#8254);
#6266=LINE('',#38889,#8255);
#6267=LINE('',#38893,#8256);
#6268=LINE('',#38897,#8257);
#6269=LINE('',#38900,#8258);
#6270=LINE('',#38901,#8259);
#6271=LINE('',#38905,#8260);
#6272=LINE('',#38908,#8261);
#6273=LINE('',#38909,#8262);
#6274=LINE('',#38913,#8263);
#6275=LINE('',#38916,#8264);
#6276=LINE('',#38917,#8265);
#6277=LINE('',#38921,#8266);
#6278=LINE('',#38925,#8267);
#6279=LINE('',#38929,#8268);
#6280=LINE('',#38932,#8269);
#6281=LINE('',#38933,#8270);
#6282=LINE('',#38936,#8271);
#6283=LINE('',#38937,#8272);
#6284=LINE('',#38940,#8273);
#6285=LINE('',#38941,#8274);
#6286=LINE('',#38945,#8275);
#6287=LINE('',#38949,#8276);
#6288=LINE('',#38953,#8277);
#6289=LINE('',#38956,#8278);
#6290=LINE('',#38957,#8279);
#6291=LINE('',#38961,#8280);
#6292=LINE('',#38964,#8281);
#6293=LINE('',#38965,#8282);
#6294=LINE('',#38969,#8283);
#6295=LINE('',#38972,#8284);
#6296=LINE('',#38973,#8285);
#6297=LINE('',#38977,#8286);
#6298=LINE('',#38981,#8287);
#6299=LINE('',#38985,#8288);
#6300=LINE('',#38988,#8289);
#6301=LINE('',#38989,#8290);
#6302=LINE('',#38993,#8291);
#6303=LINE('',#38996,#8292);
#6304=LINE('',#38997,#8293);
#6305=LINE('',#39001,#8294);
#6306=LINE('',#39003,#8295);
#6307=LINE('',#39007,#8296);
#6308=LINE('',#39009,#8297);
#6309=LINE('',#39011,#8298);
#6310=LINE('',#39012,#8299);
#6311=LINE('',#39015,#8300);
#6312=LINE('',#39017,#8301);
#6313=LINE('',#39018,#8302);
#6314=LINE('',#39021,#8303);
#6315=LINE('',#39023,#8304);
#6316=LINE('',#39024,#8305);
#6317=LINE('',#39027,#8306);
#6318=LINE('',#39029,#8307);
#6319=LINE('',#39030,#8308);
#6320=LINE('',#39033,#8309);
#6321=LINE('',#39035,#8310);
#6322=LINE('',#39036,#8311);
#6323=LINE('',#39040,#8312);
#6324=LINE('',#39042,#8313);
#6325=LINE('',#39044,#8314);
#6326=LINE('',#39045,#8315);
#6327=LINE('',#39048,#8316);
#6328=LINE('',#39050,#8317);
#6329=LINE('',#39051,#8318);
#6330=LINE('',#39054,#8319);
#6331=LINE('',#39056,#8320);
#6332=LINE('',#39057,#8321);
#6333=LINE('',#39059,#8322);
#6334=LINE('',#39060,#8323);
#6335=LINE('',#39063,#8324);
#6336=LINE('',#39065,#8325);
#6337=LINE('',#39067,#8326);
#6338=LINE('',#39068,#8327);
#6339=LINE('',#39071,#8328);
#6340=LINE('',#39073,#8329);
#6341=LINE('',#39074,#8330);
#6342=LINE('',#39078,#8331);
#6343=LINE('',#39079,#8332);
#6344=LINE('',#39080,#8333);
#6345=LINE('',#39084,#8334);
#6346=LINE('',#39085,#8335);
#6347=LINE('',#39086,#8336);
#6348=LINE('',#39090,#8337);
#6349=LINE('',#39091,#8338);
#6350=LINE('',#39092,#8339);
#6351=LINE('',#39096,#8340);
#6352=LINE('',#39097,#8341);
#6353=LINE('',#39098,#8342);
#6354=LINE('',#39101,#8343);
#6355=LINE('',#39103,#8344);
#6356=LINE('',#39104,#8345);
#6357=LINE('',#39108,#8346);
#6358=LINE('',#39109,#8347);
#6359=LINE('',#39110,#8348);
#6360=LINE('',#39114,#8349);
#6361=LINE('',#39115,#8350);
#6362=LINE('',#39116,#8351);
#6363=LINE('',#39120,#8352);
#6364=LINE('',#39121,#8353);
#6365=LINE('',#39122,#8354);
#6366=LINE('',#39125,#8355);
#6367=LINE('',#39127,#8356);
#6368=LINE('',#39128,#8357);
#6369=LINE('',#39131,#8358);
#6370=LINE('',#39133,#8359);
#6371=LINE('',#39134,#8360);
#6372=LINE('',#39137,#8361);
#6373=LINE('',#39139,#8362);
#6374=LINE('',#39140,#8363);
#6375=LINE('',#39143,#8364);
#6376=LINE('',#39145,#8365);
#6377=LINE('',#39146,#8366);
#6378=LINE('',#39149,#8367);
#6379=LINE('',#39150,#8368);
#6380=LINE('',#39151,#8369);
#6381=LINE('',#39156,#8370);
#6382=LINE('',#39157,#8371);
#6383=LINE('',#39161,#8372);
#6384=LINE('',#39162,#8373);
#6385=LINE('',#39163,#8374);
#6386=LINE('',#39168,#8375);
#6387=LINE('',#39169,#8376);
#6388=LINE('',#39174,#8377);
#6389=LINE('',#39175,#8378);
#6390=LINE('',#39179,#8379);
#6391=LINE('',#39180,#8380);
#6392=LINE('',#39181,#8381);
#6393=LINE('',#39183,#8382);
#6394=LINE('',#39188,#8383);
#6395=LINE('',#39189,#8384);
#6396=LINE('',#39192,#8385);
#6397=LINE('',#39194,#8386);
#6398=LINE('',#39195,#8387);
#6399=LINE('',#39198,#8388);
#6400=LINE('',#39200,#8389);
#6401=LINE('',#39201,#8390);
#6402=LINE('',#39203,#8391);
#6403=LINE('',#39205,#8392);
#6404=LINE('',#39206,#8393);
#6405=LINE('',#39209,#8394);
#6406=LINE('',#39212,#8395);
#6407=LINE('',#39214,#8396);
#6408=LINE('',#39218,#8397);
#6409=LINE('',#39222,#8398);
#6410=LINE('',#39230,#8399);
#6411=LINE('',#39234,#8400);
#6412=LINE('',#39238,#8401);
#6413=LINE('',#39246,#8402);
#6414=LINE('',#39248,#8403);
#6415=LINE('',#39250,#8404);
#6416=LINE('',#39258,#8405);
#6417=LINE('',#39262,#8406);
#6418=LINE('',#39266,#8407);
#6419=LINE('',#39274,#8408);
#6420=LINE('',#39278,#8409);
#6421=LINE('',#39282,#8410);
#6422=LINE('',#39283,#8411);
#6423=LINE('',#39286,#8412);
#6424=LINE('',#39288,#8413);
#6425=LINE('',#39290,#8414);
#6426=LINE('',#39292,#8415);
#6427=LINE('',#39294,#8416);
#6428=LINE('',#39296,#8417);
#6429=LINE('',#39298,#8418);
#6430=LINE('',#39300,#8419);
#6431=LINE('',#39302,#8420);
#6432=LINE('',#39304,#8421);
#6433=LINE('',#39306,#8422);
#6434=LINE('',#39308,#8423);
#6435=LINE('',#39309,#8424);
#6436=LINE('',#39313,#8425);
#6437=LINE('',#39314,#8426);
#6438=LINE('',#39315,#8427);
#6439=LINE('',#39319,#8428);
#6440=LINE('',#39320,#8429);
#6441=LINE('',#39321,#8430);
#6442=LINE('',#39324,#8431);
#6443=LINE('',#39325,#8432);
#6444=LINE('',#39328,#8433);
#6445=LINE('',#39329,#8434);
#6446=LINE('',#39332,#8435);
#6447=LINE('',#39333,#8436);
#6448=LINE('',#39336,#8437);
#6449=LINE('',#39339,#8438);
#6450=LINE('',#39342,#8439);
#6451=LINE('',#39345,#8440);
#6452=LINE('',#39347,#8441);
#6453=LINE('',#39350,#8442);
#6454=LINE('',#39351,#8443);
#6455=LINE('',#39353,#8444);
#6456=LINE('',#39358,#8445);
#6457=LINE('',#39359,#8446);
#6458=LINE('',#39364,#8447);
#6459=LINE('',#39365,#8448);
#6460=LINE('',#39372,#8449);
#6461=LINE('',#39373,#8450);
#6462=LINE('',#39378,#8451);
#6463=LINE('',#39379,#8452);
#6464=LINE('',#39381,#8453);
#6465=LINE('',#39383,#8454);
#6466=LINE('',#39388,#8455);
#6467=LINE('',#39389,#8456);
#6468=LINE('',#39394,#8457);
#6469=LINE('',#39395,#8458);
#6470=LINE('',#39400,#8459);
#6471=LINE('',#39402,#8460);
#6472=LINE('',#39403,#8461);
#6473=LINE('',#39405,#8462);
#6474=LINE('',#39410,#8463);
#6475=LINE('',#39411,#8464);
#6476=LINE('',#39416,#8465);
#6477=LINE('',#39417,#8466);
#6478=LINE('',#39424,#8467);
#6479=LINE('',#39425,#8468);
#6480=LINE('',#39430,#8469);
#6481=LINE('',#39431,#8470);
#6482=LINE('',#39433,#8471);
#6483=LINE('',#39435,#8472);
#6484=LINE('',#39437,#8473);
#6485=LINE('',#39442,#8474);
#6486=LINE('',#39443,#8475);
#6487=LINE('',#39448,#8476);
#6488=LINE('',#39449,#8477);
#6489=LINE('',#39454,#8478);
#6490=LINE('',#39457,#8479);
#6491=LINE('',#39460,#8480);
#6492=LINE('',#39463,#8481);
#6493=LINE('',#39467,#8482);
#6494=LINE('',#39468,#8483);
#6495=LINE('',#39469,#8484);
#6496=LINE('',#39472,#8485);
#6497=LINE('',#39473,#8486);
#6498=LINE('',#39476,#8487);
#6499=LINE('',#39477,#8488);
#6500=LINE('',#39479,#8489);
#6501=LINE('',#39482,#8490);
#6502=LINE('',#39483,#8491);
#6503=LINE('',#39485,#8492);
#6504=LINE('',#39487,#8493);
#6505=LINE('',#39489,#8494);
#6506=LINE('',#39491,#8495);
#6507=LINE('',#39493,#8496);
#6508=LINE('',#39495,#8497);
#6509=LINE('',#39498,#8498);
#6510=LINE('',#39499,#8499);
#6511=LINE('',#39501,#8500);
#6512=LINE('',#39505,#8501);
#6513=LINE('',#39506,#8502);
#6514=LINE('',#39510,#8503);
#6515=LINE('',#39512,#8504);
#6516=LINE('',#39557,#8505);
#6517=LINE('',#39600,#8506);
#6518=LINE('',#39619,#8507);
#6519=LINE('',#39656,#8508);
#6520=LINE('',#39657,#8509);
#6521=LINE('',#39660,#8510);
#6522=LINE('',#39661,#8511);
#6523=LINE('',#39664,#8512);
#6524=LINE('',#39665,#8513);
#6525=LINE('',#39668,#8514);
#6526=LINE('',#39669,#8515);
#6527=LINE('',#39672,#8516);
#6528=LINE('',#39673,#8517);
#6529=LINE('',#39676,#8518);
#6530=LINE('',#39677,#8519);
#6531=LINE('',#39681,#8520);
#6532=LINE('',#39682,#8521);
#6533=LINE('',#39683,#8522);
#6534=LINE('',#39686,#8523);
#6535=LINE('',#39687,#8524);
#6536=LINE('',#39690,#8525);
#6537=LINE('',#39691,#8526);
#6538=LINE('',#39694,#8527);
#6539=LINE('',#39695,#8528);
#6540=LINE('',#39698,#8529);
#6541=LINE('',#39699,#8530);
#6542=LINE('',#39701,#8531);
#6543=LINE('',#39784,#8532);
#6544=LINE('',#39785,#8533);
#6545=LINE('',#39787,#8534);
#6546=LINE('',#39789,#8535);
#6547=LINE('',#39791,#8536);
#6548=LINE('',#39793,#8537);
#6549=LINE('',#39812,#8538);
#6550=LINE('',#39816,#8539);
#6551=LINE('',#39837,#8540);
#6552=LINE('',#39847,#8541);
#6553=LINE('',#39852,#8542);
#6554=LINE('',#39861,#8543);
#6555=LINE('',#39868,#8544);
#6556=LINE('',#39871,#8545);
#6557=LINE('',#39882,#8546);
#6558=LINE('',#39887,#8547);
#6559=LINE('',#39895,#8548);
#6560=LINE('',#39899,#8549);
#6561=LINE('',#39918,#8550);
#6562=LINE('',#39920,#8551);
#6563=LINE('',#39921,#8552);
#6564=LINE('',#39925,#8553);
#6565=LINE('',#39926,#8554);
#6566=LINE('',#39929,#8555);
#6567=LINE('',#39930,#8556);
#6568=LINE('',#39972,#8557);
#6569=LINE('',#40011,#8558);
#6570=LINE('',#40017,#8559);
#6571=LINE('',#40023,#8560);
#6572=LINE('',#40029,#8561);
#6573=LINE('',#40035,#8562);
#6574=LINE('',#40041,#8563);
#6575=LINE('',#40047,#8564);
#6576=LINE('',#40053,#8565);
#6577=LINE('',#40059,#8566);
#6578=LINE('',#40065,#8567);
#6579=LINE('',#40071,#8568);
#6580=LINE('',#40077,#8569);
#6581=LINE('',#40086,#8570);
#6582=LINE('',#40090,#8571);
#6583=LINE('',#40142,#8572);
#6584=LINE('',#40145,#8573);
#6585=LINE('',#40148,#8574);
#6586=LINE('',#40150,#8575);
#6587=LINE('',#40201,#8576);
#6588=LINE('',#40202,#8577);
#6589=LINE('',#40218,#8578);
#6590=LINE('',#40224,#8579);
#6591=LINE('',#40230,#8580);
#6592=LINE('',#40236,#8581);
#6593=LINE('',#40242,#8582);
#6594=LINE('',#40248,#8583);
#6595=LINE('',#40254,#8584);
#6596=LINE('',#40259,#8585);
#6597=LINE('',#40261,#8586);
#6598=LINE('',#40263,#8587);
#6599=LINE('',#40264,#8588);
#6600=LINE('',#40267,#8589);
#6601=LINE('',#40269,#8590);
#6602=LINE('',#40270,#8591);
#6603=LINE('',#40273,#8592);
#6604=LINE('',#40275,#8593);
#6605=LINE('',#40276,#8594);
#6606=LINE('',#40279,#8595);
#6607=LINE('',#40281,#8596);
#6608=LINE('',#40282,#8597);
#6609=LINE('',#40285,#8598);
#6610=LINE('',#40287,#8599);
#6611=LINE('',#40288,#8600);
#6612=LINE('',#40291,#8601);
#6613=LINE('',#40293,#8602);
#6614=LINE('',#40294,#8603);
#6615=LINE('',#40297,#8604);
#6616=LINE('',#40299,#8605);
#6617=LINE('',#40300,#8606);
#6618=LINE('',#40303,#8607);
#6619=LINE('',#40305,#8608);
#6620=LINE('',#40306,#8609);
#6621=LINE('',#40309,#8610);
#6622=LINE('',#40311,#8611);
#6623=LINE('',#40312,#8612);
#6624=LINE('',#40315,#8613);
#6625=LINE('',#40317,#8614);
#6626=LINE('',#40318,#8615);
#6627=LINE('',#40321,#8616);
#6628=LINE('',#40323,#8617);
#6629=LINE('',#40324,#8618);
#6630=LINE('',#40326,#8619);
#6631=LINE('',#40327,#8620);
#6632=LINE('',#40339,#8621);
#6633=LINE('',#40345,#8622);
#6634=LINE('',#40352,#8623);
#6635=LINE('',#40355,#8624);
#6636=LINE('',#40361,#8625);
#6637=LINE('',#40364,#8626);
#6638=LINE('',#40368,#8627);
#6639=LINE('',#40372,#8628);
#6640=LINE('',#40377,#8629);
#6641=LINE('',#40381,#8630);
#6642=LINE('',#40382,#8631);
#6643=LINE('',#40383,#8632);
#6644=LINE('',#40387,#8633);
#6645=LINE('',#40388,#8634);
#6646=LINE('',#40390,#8635);
#6647=LINE('',#40392,#8636);
#6648=LINE('',#40396,#8637);
#6649=LINE('',#40401,#8638);
#6650=LINE('',#40404,#8639);
#6651=LINE('',#40405,#8640);
#6652=LINE('',#40407,#8641);
#6653=LINE('',#40409,#8642);
#6654=LINE('',#40412,#8643);
#6655=LINE('',#40414,#8644);
#6656=LINE('',#40416,#8645);
#6657=LINE('',#40418,#8646);
#6658=LINE('',#40429,#8647);
#6659=LINE('',#40435,#8648);
#6660=LINE('',#40441,#8649);
#6661=LINE('',#40447,#8650);
#6662=LINE('',#40453,#8651);
#6663=LINE('',#40459,#8652);
#6664=LINE('',#40465,#8653);
#6665=LINE('',#40471,#8654);
#6666=LINE('',#40477,#8655);
#6667=LINE('',#40483,#8656);
#6668=LINE('',#40489,#8657);
#6669=LINE('',#40495,#8658);
#6670=LINE('',#40501,#8659);
#6671=LINE('',#40507,#8660);
#6672=LINE('',#40513,#8661);
#6673=LINE('',#40519,#8662);
#6674=LINE('',#40525,#8663);
#6675=LINE('',#40531,#8664);
#6676=LINE('',#40537,#8665);
#6677=LINE('',#40543,#8666);
#6678=LINE('',#40549,#8667);
#6679=LINE('',#40558,#8668);
#6680=LINE('',#40560,#8669);
#6681=LINE('',#40562,#8670);
#6682=LINE('',#40564,#8671);
#6683=LINE('',#40566,#8672);
#6684=LINE('',#40568,#8673);
#6685=LINE('',#40570,#8674);
#6686=LINE('',#40572,#8675);
#6687=LINE('',#40574,#8676);
#6688=LINE('',#40576,#8677);
#6689=LINE('',#40578,#8678);
#6690=LINE('',#40579,#8679);
#6691=LINE('',#40582,#8680);
#6692=LINE('',#40584,#8681);
#6693=LINE('',#40586,#8682);
#6694=LINE('',#40588,#8683);
#6695=LINE('',#40590,#8684);
#6696=LINE('',#40592,#8685);
#6697=LINE('',#40594,#8686);
#6698=LINE('',#40595,#8687);
#6699=LINE('',#40599,#8688);
#6700=LINE('',#40600,#8689);
#6701=LINE('',#40601,#8690);
#6702=LINE('',#40604,#8691);
#6703=LINE('',#40605,#8692);
#6704=LINE('',#40608,#8693);
#6705=LINE('',#40609,#8694);
#6706=LINE('',#40612,#8695);
#6707=LINE('',#40613,#8696);
#6708=LINE('',#40616,#8697);
#6709=LINE('',#40617,#8698);
#6710=LINE('',#40620,#8699);
#6711=LINE('',#40621,#8700);
#6712=LINE('',#40624,#8701);
#6713=LINE('',#40625,#8702);
#6714=LINE('',#40628,#8703);
#6715=LINE('',#40629,#8704);
#6716=LINE('',#40632,#8705);
#6717=LINE('',#40633,#8706);
#6718=LINE('',#40636,#8707);
#6719=LINE('',#40637,#8708);
#6720=LINE('',#40640,#8709);
#6721=LINE('',#40641,#8710);
#6722=LINE('',#40643,#8711);
#6723=LINE('',#40652,#8712);
#6724=LINE('',#40654,#8713);
#6725=LINE('',#40656,#8714);
#6726=LINE('',#40658,#8715);
#6727=LINE('',#40660,#8716);
#6728=LINE('',#40662,#8717);
#6729=LINE('',#40664,#8718);
#6730=LINE('',#40665,#8719);
#6731=LINE('',#40667,#8720);
#6732=LINE('',#40668,#8721);
#6733=LINE('',#40670,#8722);
#6734=LINE('',#40672,#8723);
#6735=LINE('',#40674,#8724);
#6736=LINE('',#40676,#8725);
#6737=LINE('',#40678,#8726);
#6738=LINE('',#40680,#8727);
#6739=LINE('',#40685,#8728);
#6740=LINE('',#40687,#8729);
#6741=LINE('',#40689,#8730);
#6742=LINE('',#40691,#8731);
#6743=LINE('',#40693,#8732);
#6744=LINE('',#40694,#8733);
#6745=LINE('',#40698,#8734);
#6746=LINE('',#40700,#8735);
#6747=LINE('',#40702,#8736);
#6748=LINE('',#40704,#8737);
#6749=LINE('',#40706,#8738);
#6750=LINE('',#40707,#8739);
#6751=LINE('',#40711,#8740);
#6752=LINE('',#40713,#8741);
#6753=LINE('',#40715,#8742);
#6754=LINE('',#40717,#8743);
#6755=LINE('',#40719,#8744);
#6756=LINE('',#40720,#8745);
#6757=LINE('',#40724,#8746);
#6758=LINE('',#40726,#8747);
#6759=LINE('',#40728,#8748);
#6760=LINE('',#40730,#8749);
#6761=LINE('',#40732,#8750);
#6762=LINE('',#40733,#8751);
#6763=LINE('',#40736,#8752);
#6764=LINE('',#40738,#8753);
#6765=LINE('',#40739,#8754);
#6766=LINE('',#40742,#8755);
#6767=LINE('',#40743,#8756);
#6768=LINE('',#40746,#8757);
#6769=LINE('',#40747,#8758);
#6770=LINE('',#40750,#8759);
#6771=LINE('',#40751,#8760);
#6772=LINE('',#40754,#8761);
#6773=LINE('',#40755,#8762);
#6774=LINE('',#40757,#8763);
#6775=LINE('',#40761,#8764);
#6776=LINE('',#40763,#8765);
#6777=LINE('',#40764,#8766);
#6778=LINE('',#40767,#8767);
#6779=LINE('',#40768,#8768);
#6780=LINE('',#40771,#8769);
#6781=LINE('',#40772,#8770);
#6782=LINE('',#40775,#8771);
#6783=LINE('',#40776,#8772);
#6784=LINE('',#40779,#8773);
#6785=LINE('',#40780,#8774);
#6786=LINE('',#40782,#8775);
#6787=LINE('',#40786,#8776);
#6788=LINE('',#40788,#8777);
#6789=LINE('',#40789,#8778);
#6790=LINE('',#40792,#8779);
#6791=LINE('',#40793,#8780);
#6792=LINE('',#40796,#8781);
#6793=LINE('',#40797,#8782);
#6794=LINE('',#40800,#8783);
#6795=LINE('',#40801,#8784);
#6796=LINE('',#40804,#8785);
#6797=LINE('',#40805,#8786);
#6798=LINE('',#40807,#8787);
#6799=LINE('',#40811,#8788);
#6800=LINE('',#40813,#8789);
#6801=LINE('',#40814,#8790);
#6802=LINE('',#40817,#8791);
#6803=LINE('',#40818,#8792);
#6804=LINE('',#40821,#8793);
#6805=LINE('',#40822,#8794);
#6806=LINE('',#40825,#8795);
#6807=LINE('',#40826,#8796);
#6808=LINE('',#40829,#8797);
#6809=LINE('',#40830,#8798);
#6810=LINE('',#40832,#8799);
#6811=LINE('',#40842,#8800);
#6812=LINE('',#40876,#8801);
#6813=LINE('',#40899,#8802);
#6814=LINE('',#40943,#8803);
#6815=LINE('',#40948,#8804);
#6816=LINE('',#40992,#8805);
#6817=LINE('',#40999,#8806);
#6818=LINE('',#41006,#8807);
#6819=LINE('',#41009,#8808);
#6820=LINE('',#41014,#8809);
#6821=LINE('',#41017,#8810);
#6822=LINE('',#41036,#8811);
#6823=LINE('',#41039,#8812);
#6824=LINE('',#41045,#8813);
#6825=LINE('',#41048,#8814);
#6826=LINE('',#41054,#8815);
#6827=LINE('',#41057,#8816);
#6828=LINE('',#41060,#8817);
#6829=LINE('',#41061,#8818);
#6830=LINE('',#41062,#8819);
#6831=LINE('',#41063,#8820);
#6832=LINE('',#41065,#8821);
#6833=LINE('',#41066,#8822);
#6834=LINE('',#41067,#8823);
#6835=LINE('',#41068,#8824);
#6836=LINE('',#41076,#8825);
#6837=LINE('',#41077,#8826);
#6838=LINE('',#41079,#8827);
#6839=LINE('',#41080,#8828);
#6840=LINE('',#41082,#8829);
#6841=LINE('',#41084,#8830);
#6842=LINE('',#41085,#8831);
#6843=LINE('',#41087,#8832);
#6844=LINE('',#41089,#8833);
#6845=LINE('',#41090,#8834);
#6846=LINE('',#41092,#8835);
#6847=LINE('',#41094,#8836);
#6848=LINE('',#41095,#8837);
#6849=LINE('',#41097,#8838);
#6850=LINE('',#41099,#8839);
#6851=LINE('',#41100,#8840);
#6852=LINE('',#41102,#8841);
#6853=LINE('',#41103,#8842);
#6854=LINE('',#41115,#8843);
#6855=LINE('',#41121,#8844);
#6856=LINE('',#41134,#8845);
#6857=LINE('',#41140,#8846);
#6858=LINE('',#41146,#8847);
#6859=LINE('',#41152,#8848);
#6860=LINE('',#41158,#8849);
#6861=LINE('',#41164,#8850);
#6862=LINE('',#41169,#8851);
#6863=LINE('',#41171,#8852);
#6864=LINE('',#41173,#8853);
#6865=LINE('',#41174,#8854);
#6866=LINE('',#41177,#8855);
#6867=LINE('',#41179,#8856);
#6868=LINE('',#41181,#8857);
#6869=LINE('',#41183,#8858);
#6870=LINE('',#41184,#8859);
#6871=LINE('',#41188,#8860);
#6872=LINE('',#41189,#8861);
#6873=LINE('',#41191,#8862);
#6874=LINE('',#41192,#8863);
#6875=LINE('',#41196,#8864);
#6876=LINE('',#41198,#8865);
#6877=LINE('',#41199,#8866);
#6878=LINE('',#41201,#8867);
#6879=LINE('',#41202,#8868);
#6880=LINE('',#41205,#8869);
#6881=LINE('',#41207,#8870);
#6882=LINE('',#41208,#8871);
#6883=LINE('',#41209,#8872);
#6884=LINE('',#41212,#8873);
#6885=LINE('',#41213,#8874);
#6886=LINE('',#41217,#8875);
#6887=LINE('',#41218,#8876);
#6888=LINE('',#41220,#8877);
#6889=LINE('',#41223,#8878);
#6890=LINE('',#41224,#8879);
#6891=LINE('',#41226,#8880);
#6892=LINE('',#41236,#8881);
#6893=LINE('',#41244,#8882);
#6894=LINE('',#63971,#8883);
#6895=LINE('',#63978,#8884);
#6896=LINE('',#63985,#8885);
#6897=LINE('',#63992,#8886);
#6898=LINE('',#63998,#8887);
#6899=LINE('',#64005,#8888);
#6900=LINE('',#64012,#8889);
#6901=LINE('',#64021,#8890);
#6902=LINE('',#64023,#8891);
#6903=LINE('',#64025,#8892);
#6904=LINE('',#64027,#8893);
#6905=LINE('',#64029,#8894);
#6906=LINE('',#64030,#8895);
#6907=LINE('',#64035,#8896);
#6908=LINE('',#64039,#8897);
#6909=LINE('',#64041,#8898);
#6910=LINE('',#64043,#8899);
#6911=LINE('',#64045,#8900);
#6912=LINE('',#64047,#8901);
#6913=LINE('',#64048,#8902);
#6914=LINE('',#64050,#8903);
#6915=LINE('',#64051,#8904);
#6916=LINE('',#64053,#8905);
#6917=LINE('',#64055,#8906);
#6918=LINE('',#64057,#8907);
#6919=LINE('',#64059,#8908);
#6920=LINE('',#64069,#8909);
#6921=LINE('',#64078,#8910);
#6922=LINE('',#64080,#8911);
#6923=LINE('',#64082,#8912);
#6924=LINE('',#64084,#8913);
#6925=LINE('',#64086,#8914);
#6926=LINE('',#64087,#8915);
#6927=LINE('',#64091,#8916);
#6928=LINE('',#64093,#8917);
#6929=LINE('',#64095,#8918);
#6930=LINE('',#64097,#8919);
#6931=LINE('',#64099,#8920);
#6932=LINE('',#64100,#8921);
#6933=LINE('',#64102,#8922);
#6934=LINE('',#64103,#8923);
#6935=LINE('',#64105,#8924);
#6936=LINE('',#64107,#8925);
#6937=LINE('',#64109,#8926);
#6938=LINE('',#64111,#8927);
#6939=LINE('',#64119,#8928);
#6940=LINE('',#64121,#8929);
#6941=LINE('',#64130,#8930);
#6942=LINE('',#64139,#8931);
#6943=LINE('',#64141,#8932);
#6944=LINE('',#64143,#8933);
#6945=LINE('',#64145,#8934);
#6946=LINE('',#64147,#8935);
#6947=LINE('',#64148,#8936);
#6948=LINE('',#64152,#8937);
#6949=LINE('',#64154,#8938);
#6950=LINE('',#64156,#8939);
#6951=LINE('',#64158,#8940);
#6952=LINE('',#64160,#8941);
#6953=LINE('',#64161,#8942);
#6954=LINE('',#64163,#8943);
#6955=LINE('',#64164,#8944);
#6956=LINE('',#64166,#8945);
#6957=LINE('',#64168,#8946);
#6958=LINE('',#64170,#8947);
#6959=LINE('',#64172,#8948);
#6960=LINE('',#64180,#8949);
#6961=LINE('',#64182,#8950);
#6962=LINE('',#64187,#8951);
#6963=LINE('',#64191,#8952);
#6964=LINE('',#64197,#8953);
#6965=LINE('',#64198,#8954);
#6966=LINE('',#64221,#8955);
#6967=LINE('',#64222,#8956);
#6968=LINE('',#64225,#8957);
#6969=LINE('',#64227,#8958);
#6970=LINE('',#64231,#8959);
#6971=LINE('',#64235,#8960);
#6972=LINE('',#64240,#8961);
#6973=LINE('',#64244,#8962);
#6974=LINE('',#64249,#8963);
#6975=LINE('',#64251,#8964);
#6976=LINE('',#64300,#8965);
#6977=LINE('',#64333,#8966);
#6978=LINE('',#64336,#8967);
#6979=LINE('',#64338,#8968);
#6980=LINE('',#64339,#8969);
#6981=LINE('',#64342,#8970);
#6982=LINE('',#64351,#8971);
#6983=LINE('',#64358,#8972);
#6984=LINE('',#64399,#8973);
#6985=LINE('',#64401,#8974);
#6986=LINE('',#64403,#8975);
#6987=LINE('',#64405,#8976);
#6988=LINE('',#64406,#8977);
#6989=LINE('',#64452,#8978);
#6990=LINE('',#64457,#8979);
#6991=LINE('',#64464,#8980);
#6992=LINE('',#64467,#8981);
#6993=LINE('',#64471,#8982);
#6994=LINE('',#64473,#8983);
#6995=LINE('',#64475,#8984);
#6996=LINE('',#64477,#8985);
#6997=LINE('',#64478,#8986);
#6998=LINE('',#64483,#8987);
#6999=LINE('',#64485,#8988);
#7000=LINE('',#64487,#8989);
#7001=LINE('',#64513,#8990);
#7002=LINE('',#64515,#8991);
#7003=LINE('',#64517,#8992);
#7004=LINE('',#64521,#8993);
#7005=LINE('',#64529,#8994);
#7006=LINE('',#64532,#8995);
#7007=LINE('',#64541,#8996);
#7008=LINE('',#64545,#8997);
#7009=LINE('',#64566,#8998);
#7010=LINE('',#64573,#8999);
#7011=LINE('',#64667,#9000);
#7012=LINE('',#64669,#9001);
#7013=LINE('',#64672,#9002);
#7014=LINE('',#64673,#9003);
#7015=LINE('',#64675,#9004);
#7016=LINE('',#64677,#9005);
#7017=LINE('',#64679,#9006);
#7018=LINE('',#64681,#9007);
#7019=LINE('',#64688,#9008);
#7020=LINE('',#64689,#9009);
#7021=LINE('',#64694,#9010);
#7022=LINE('',#64695,#9011);
#7023=LINE('',#64698,#9012);
#7024=LINE('',#64701,#9013);
#7025=LINE('',#64705,#9014);
#7026=LINE('',#64710,#9015);
#7027=LINE('',#64738,#9016);
#7028=LINE('',#64742,#9017);
#7029=LINE('',#64746,#9018);
#7030=LINE('',#64749,#9019);
#7031=LINE('',#64754,#9020);
#7032=LINE('',#64758,#9021);
#7033=LINE('',#64762,#9022);
#7034=LINE('',#64765,#9023);
#7035=LINE('',#64768,#9024);
#7036=LINE('',#64774,#9025);
#7037=LINE('',#64782,#9026);
#7038=LINE('',#64788,#9027);
#7039=LINE('',#64792,#9028);
#7040=LINE('',#64798,#9029);
#7041=LINE('',#64804,#9030);
#7042=LINE('',#64810,#9031);
#7043=LINE('',#64817,#9032);
#7044=LINE('',#64821,#9033);
#7045=LINE('',#64825,#9034);
#7046=LINE('',#64828,#9035);
#7047=LINE('',#64830,#9036);
#7048=LINE('',#64831,#9037);
#7049=LINE('',#64833,#9038);
#7050=LINE('',#64835,#9039);
#7051=LINE('',#64837,#9040);
#7052=LINE('',#64839,#9041);
#7053=LINE('',#64841,#9042);
#7054=LINE('',#64843,#9043);
#7055=LINE('',#64847,#9044);
#7056=LINE('',#64850,#9045);
#7057=LINE('',#64853,#9046);
#7058=LINE('',#64854,#9047);
#7059=LINE('',#64857,#9048);
#7060=LINE('',#64861,#9049);
#7061=LINE('',#64863,#9050);
#7062=LINE('',#64864,#9051);
#7063=LINE('',#64867,#9052);
#7064=LINE('',#64871,#9053);
#7065=LINE('',#64875,#9054);
#7066=LINE('',#64876,#9055);
#7067=LINE('',#64879,#9056);
#7068=LINE('',#64883,#9057);
#7069=LINE('',#64884,#9058);
#7070=LINE('',#64895,#9059);
#7071=LINE('',#64901,#9060);
#7072=LINE('',#64904,#9061);
#7073=LINE('',#64905,#9062);
#7074=LINE('',#64907,#9063);
#7075=LINE('',#64909,#9064);
#7076=LINE('',#64911,#9065);
#7077=LINE('',#64913,#9066);
#7078=LINE('',#64917,#9067);
#7079=LINE('',#64919,#9068);
#7080=LINE('',#64920,#9069);
#7081=LINE('',#64923,#9070);
#7082=LINE('',#64927,#9071);
#7083=LINE('',#64931,#9072);
#7084=LINE('',#64932,#9073);
#7085=LINE('',#64936,#9074);
#7086=LINE('',#64942,#9075);
#7087=LINE('',#64945,#9076);
#7088=LINE('',#64948,#9077);
#7089=LINE('',#64949,#9078);
#7090=LINE('',#64952,#9079);
#7091=LINE('',#64956,#9080);
#7092=LINE('',#64975,#9081);
#7093=LINE('',#64976,#9082);
#7094=LINE('',#64979,#9083);
#7095=LINE('',#64982,#9084);
#7096=LINE('',#64985,#9085);
#7097=LINE('',#64986,#9086);
#7098=LINE('',#64989,#9087);
#7099=LINE('',#64993,#9088);
#7100=LINE('',#64994,#9089);
#7101=LINE('',#64997,#9090);
#7102=LINE('',#65000,#9091);
#7103=LINE('',#65003,#9092);
#7104=LINE('',#65023,#9093);
#7105=LINE('',#65031,#9094);
#7106=LINE('',#65033,#9095);
#7107=LINE('',#65035,#9096);
#7108=LINE('',#65037,#9097);
#7109=LINE('',#65039,#9098);
#7110=LINE('',#65040,#9099);
#7111=LINE('',#65045,#9100);
#7112=LINE('',#65049,#9101);
#7113=LINE('',#65051,#9102);
#7114=LINE('',#65053,#9103);
#7115=LINE('',#65055,#9104);
#7116=LINE('',#65057,#9105);
#7117=LINE('',#65058,#9106);
#7118=LINE('',#65060,#9107);
#7119=LINE('',#65061,#9108);
#7120=LINE('',#65063,#9109);
#7121=LINE('',#65065,#9110);
#7122=LINE('',#65067,#9111);
#7123=LINE('',#65069,#9112);
#7124=LINE('',#65079,#9113);
#7125=LINE('',#65088,#9114);
#7126=LINE('',#65090,#9115);
#7127=LINE('',#65092,#9116);
#7128=LINE('',#65094,#9117);
#7129=LINE('',#65096,#9118);
#7130=LINE('',#65097,#9119);
#7131=LINE('',#65101,#9120);
#7132=LINE('',#65103,#9121);
#7133=LINE('',#65105,#9122);
#7134=LINE('',#65107,#9123);
#7135=LINE('',#65109,#9124);
#7136=LINE('',#65110,#9125);
#7137=LINE('',#65112,#9126);
#7138=LINE('',#65113,#9127);
#7139=LINE('',#65115,#9128);
#7140=LINE('',#65117,#9129);
#7141=LINE('',#65119,#9130);
#7142=LINE('',#65121,#9131);
#7143=LINE('',#65129,#9132);
#7144=LINE('',#65131,#9133);
#7145=LINE('',#65140,#9134);
#7146=LINE('',#65149,#9135);
#7147=LINE('',#65151,#9136);
#7148=LINE('',#65153,#9137);
#7149=LINE('',#65155,#9138);
#7150=LINE('',#65157,#9139);
#7151=LINE('',#65158,#9140);
#7152=LINE('',#65162,#9141);
#7153=LINE('',#65164,#9142);
#7154=LINE('',#65166,#9143);
#7155=LINE('',#65168,#9144);
#7156=LINE('',#65170,#9145);
#7157=LINE('',#65171,#9146);
#7158=LINE('',#65173,#9147);
#7159=LINE('',#65174,#9148);
#7160=LINE('',#65176,#9149);
#7161=LINE('',#65178,#9150);
#7162=LINE('',#65180,#9151);
#7163=LINE('',#65182,#9152);
#7164=LINE('',#65190,#9153);
#7165=LINE('',#65192,#9154);
#7166=LINE('',#65197,#9155);
#7167=LINE('',#65201,#9156);
#7168=LINE('',#65207,#9157);
#7169=LINE('',#65208,#9158);
#7170=LINE('',#65231,#9159);
#7171=LINE('',#65232,#9160);
#7172=LINE('',#65235,#9161);
#7173=LINE('',#65237,#9162);
#7174=LINE('',#65241,#9163);
#7175=LINE('',#65245,#9164);
#7176=LINE('',#65250,#9165);
#7177=LINE('',#65254,#9166);
#7178=LINE('',#65259,#9167);
#7179=LINE('',#65261,#9168);
#7180=LINE('',#65310,#9169);
#7181=LINE('',#65343,#9170);
#7182=LINE('',#65346,#9171);
#7183=LINE('',#65348,#9172);
#7184=LINE('',#65349,#9173);
#7185=LINE('',#65352,#9174);
#7186=LINE('',#65361,#9175);
#7187=LINE('',#65368,#9176);
#7188=LINE('',#65409,#9177);
#7189=LINE('',#65411,#9178);
#7190=LINE('',#65413,#9179);
#7191=LINE('',#65415,#9180);
#7192=LINE('',#65416,#9181);
#7193=LINE('',#65462,#9182);
#7194=LINE('',#65467,#9183);
#7195=LINE('',#65474,#9184);
#7196=LINE('',#65477,#9185);
#7197=LINE('',#65481,#9186);
#7198=LINE('',#65483,#9187);
#7199=LINE('',#65485,#9188);
#7200=LINE('',#65487,#9189);
#7201=LINE('',#65488,#9190);
#7202=LINE('',#65493,#9191);
#7203=LINE('',#65495,#9192);
#7204=LINE('',#65497,#9193);
#7205=LINE('',#65523,#9194);
#7206=LINE('',#65525,#9195);
#7207=LINE('',#65527,#9196);
#7208=LINE('',#65530,#9197);
#7209=LINE('',#65532,#9198);
#7210=LINE('',#65536,#9199);
#7211=LINE('',#65557,#9200);
#7212=LINE('',#65563,#9201);
#7213=LINE('',#65656,#9202);
#7214=LINE('',#65658,#9203);
#7215=LINE('',#65664,#9204);
#7216=LINE('',#65665,#9205);
#7217=LINE('',#65670,#9206);
#7218=LINE('',#65671,#9207);
#7219=LINE('',#65674,#9208);
#7220=LINE('',#65677,#9209);
#7221=LINE('',#65681,#9210);
#7222=LINE('',#65686,#9211);
#7223=LINE('',#65714,#9212);
#7224=LINE('',#65718,#9213);
#7225=LINE('',#65722,#9214);
#7226=LINE('',#65725,#9215);
#7227=LINE('',#65730,#9216);
#7228=LINE('',#65734,#9217);
#7229=LINE('',#65738,#9218);
#7230=LINE('',#65741,#9219);
#7231=LINE('',#65744,#9220);
#7232=LINE('',#65750,#9221);
#7233=LINE('',#65758,#9222);
#7234=LINE('',#65764,#9223);
#7235=LINE('',#65768,#9224);
#7236=LINE('',#65774,#9225);
#7237=LINE('',#65780,#9226);
#7238=LINE('',#65786,#9227);
#7239=LINE('',#65793,#9228);
#7240=LINE('',#65797,#9229);
#7241=LINE('',#65801,#9230);
#7242=LINE('',#65804,#9231);
#7243=LINE('',#65806,#9232);
#7244=LINE('',#65807,#9233);
#7245=LINE('',#65809,#9234);
#7246=LINE('',#65811,#9235);
#7247=LINE('',#65813,#9236);
#7248=LINE('',#65815,#9237);
#7249=LINE('',#65817,#9238);
#7250=LINE('',#65819,#9239);
#7251=LINE('',#65823,#9240);
#7252=LINE('',#65826,#9241);
#7253=LINE('',#65829,#9242);
#7254=LINE('',#65830,#9243);
#7255=LINE('',#65833,#9244);
#7256=LINE('',#65837,#9245);
#7257=LINE('',#65839,#9246);
#7258=LINE('',#65840,#9247);
#7259=LINE('',#65843,#9248);
#7260=LINE('',#65847,#9249);
#7261=LINE('',#65851,#9250);
#7262=LINE('',#65852,#9251);
#7263=LINE('',#65855,#9252);
#7264=LINE('',#65859,#9253);
#7265=LINE('',#65860,#9254);
#7266=LINE('',#65871,#9255);
#7267=LINE('',#65877,#9256);
#7268=LINE('',#65880,#9257);
#7269=LINE('',#65881,#9258);
#7270=LINE('',#65883,#9259);
#7271=LINE('',#65885,#9260);
#7272=LINE('',#65887,#9261);
#7273=LINE('',#65889,#9262);
#7274=LINE('',#65893,#9263);
#7275=LINE('',#65895,#9264);
#7276=LINE('',#65896,#9265);
#7277=LINE('',#65899,#9266);
#7278=LINE('',#65903,#9267);
#7279=LINE('',#65907,#9268);
#7280=LINE('',#65908,#9269);
#7281=LINE('',#65912,#9270);
#7282=LINE('',#65918,#9271);
#7283=LINE('',#65921,#9272);
#7284=LINE('',#65924,#9273);
#7285=LINE('',#65925,#9274);
#7286=LINE('',#65928,#9275);
#7287=LINE('',#65932,#9276);
#7288=LINE('',#65951,#9277);
#7289=LINE('',#65952,#9278);
#7290=LINE('',#65955,#9279);
#7291=LINE('',#65958,#9280);
#7292=LINE('',#65961,#9281);
#7293=LINE('',#65962,#9282);
#7294=LINE('',#65965,#9283);
#7295=LINE('',#65969,#9284);
#7296=LINE('',#65970,#9285);
#7297=LINE('',#65973,#9286);
#7298=LINE('',#65976,#9287);
#7299=LINE('',#65979,#9288);
#7300=LINE('',#65999,#9289);
#7301=LINE('',#66016,#9290);
#7302=LINE('',#66020,#9291);
#7303=LINE('',#66025,#9292);
#7304=LINE('',#66029,#9293);
#7305=LINE('',#66034,#9294);
#7306=LINE('',#66038,#9295);
#7307=LINE('',#66043,#9296);
#7308=LINE('',#66047,#9297);
#7309=LINE('',#66052,#9298);
#7310=LINE('',#66056,#9299);
#7311=LINE('',#66061,#9300);
#7312=LINE('',#66065,#9301);
#7313=LINE('',#66070,#9302);
#7314=LINE('',#66074,#9303);
#7315=LINE('',#66079,#9304);
#7316=LINE('',#66083,#9305);
#7317=LINE('',#66088,#9306);
#7318=LINE('',#66092,#9307);
#7319=LINE('',#66097,#9308);
#7320=LINE('',#66101,#9309);
#7321=LINE('',#66106,#9310);
#7322=LINE('',#66110,#9311);
#7323=LINE('',#66115,#9312);
#7324=LINE('',#66119,#9313);
#7325=LINE('',#66124,#9314);
#7326=LINE('',#66128,#9315);
#7327=LINE('',#66133,#9316);
#7328=LINE('',#66137,#9317);
#7329=LINE('',#66142,#9318);
#7330=LINE('',#66146,#9319);
#7331=LINE('',#66151,#9320);
#7332=LINE('',#66155,#9321);
#7333=LINE('',#66160,#9322);
#7334=LINE('',#66164,#9323);
#7335=LINE('',#66168,#9324);
#7336=LINE('',#66170,#9325);
#7337=LINE('',#66172,#9326);
#7338=LINE('',#66173,#9327);
#7339=LINE('',#66176,#9328);
#7340=LINE('',#66180,#9329);
#7341=LINE('',#66184,#9330);
#7342=LINE('',#66186,#9331);
#7343=LINE('',#66188,#9332);
#7344=LINE('',#66190,#9333);
#7345=LINE('',#66191,#9334);
#7346=LINE('',#66194,#9335);
#7347=LINE('',#66196,#9336);
#7348=LINE('',#66197,#9337);
#7349=LINE('',#66201,#9338);
#7350=LINE('',#66205,#9339);
#7351=LINE('',#66208,#9340);
#7352=LINE('',#66209,#9341);
#7353=LINE('',#66211,#9342);
#7354=LINE('',#66212,#9343);
#7355=LINE('',#66214,#9344);
#7356=LINE('',#66215,#9345);
#7357=LINE('',#66219,#9346);
#7358=LINE('',#66221,#9347);
#7359=LINE('',#66222,#9348);
#7360=LINE('',#66224,#9349);
#7361=LINE('',#66232,#9350);
#7362=LINE('',#66236,#9351);
#7363=LINE('',#66243,#9352);
#7364=LINE('',#66248,#9353);
#7365=LINE('',#66254,#9354);
#7366=LINE('',#66256,#9355);
#7367=LINE('',#66258,#9356);
#7368=LINE('',#66260,#9357);
#7369=LINE('',#66262,#9358);
#7370=LINE('',#66263,#9359);
#7371=LINE('',#66267,#9360);
#7372=LINE('',#66269,#9361);
#7373=LINE('',#66270,#9362);
#7374=LINE('',#66273,#9363);
#7375=LINE('',#66274,#9364);
#7376=LINE('',#66277,#9365);
#7377=LINE('',#66278,#9366);
#7378=LINE('',#66281,#9367);
#7379=LINE('',#66282,#9368);
#7380=LINE('',#66285,#9369);
#7381=LINE('',#66286,#9370);
#7382=LINE('',#66288,#9371);
#7383=LINE('',#66297,#9372);
#7384=LINE('',#66302,#9373);
#7385=LINE('',#66318,#9374);
#7386=LINE('',#66324,#9375);
#7387=LINE('',#66330,#9376);
#7388=LINE('',#66335,#9377);
#7389=LINE('',#66337,#9378);
#7390=LINE('',#66339,#9379);
#7391=LINE('',#66341,#9380);
#7392=LINE('',#66343,#9381);
#7393=LINE('',#66344,#9382);
#7394=LINE('',#66350,#9383);
#7395=LINE('',#66351,#9384);
#7396=LINE('',#66353,#9385);
#7397=LINE('',#66354,#9386);
#7398=LINE('',#66357,#9387);
#7399=LINE('',#66358,#9388);
#7400=LINE('',#66359,#9389);
#7401=LINE('',#66362,#9390);
#7402=LINE('',#66363,#9391);
#7403=LINE('',#66364,#9392);
#7404=LINE('',#66367,#9393);
#7405=LINE('',#66368,#9394);
#7406=LINE('',#66369,#9395);
#7407=LINE('',#66372,#9396);
#7408=LINE('',#66373,#9397);
#7409=LINE('',#66374,#9398);
#7410=LINE('',#66376,#9399);
#7411=LINE('',#66377,#9400);
#7412=LINE('',#66388,#9401);
#7413=LINE('',#66394,#9402);
#7414=LINE('',#66403,#9403);
#7415=LINE('',#66406,#9404);
#7416=LINE('',#66412,#9405);
#7417=LINE('',#66415,#9406);
#7418=LINE('',#66417,#9407);
#7419=LINE('',#66418,#9408);
#7420=LINE('',#66420,#9409);
#7421=LINE('',#66421,#9410);
#7422=LINE('',#66429,#9411);
#7423=LINE('',#66435,#9412);
#7424=LINE('',#66441,#9413);
#7425=LINE('',#66447,#9414);
#7426=LINE('',#66453,#9415);
#7427=LINE('',#66459,#9416);
#7428=LINE('',#66465,#9417);
#7429=LINE('',#66471,#9418);
#7430=LINE('',#66477,#9419);
#7431=LINE('',#66483,#9420);
#7432=LINE('',#66488,#9421);
#7433=LINE('',#66490,#9422);
#7434=LINE('',#66492,#9423);
#7435=LINE('',#66493,#9424);
#7436=LINE('',#66496,#9425);
#7437=LINE('',#66498,#9426);
#7438=LINE('',#66499,#9427);
#7439=LINE('',#66502,#9428);
#7440=LINE('',#66504,#9429);
#7441=LINE('',#66506,#9430);
#7442=LINE('',#66507,#9431);
#7443=LINE('',#66510,#9432);
#7444=LINE('',#66512,#9433);
#7445=LINE('',#66513,#9434);
#7446=LINE('',#66516,#9435);
#7447=LINE('',#66517,#9436);
#7448=LINE('',#66518,#9437);
#7449=LINE('',#66521,#9438);
#7450=LINE('',#66528,#9439);
#7451=LINE('',#66532,#9440);
#7452=LINE('',#66539,#9441);
#7453=LINE('',#66544,#9442);
#7454=LINE('',#66550,#9443);
#7455=LINE('',#66552,#9444);
#7456=LINE('',#66554,#9445);
#7457=LINE('',#66556,#9446);
#7458=LINE('',#66558,#9447);
#7459=LINE('',#66559,#9448);
#7460=LINE('',#66563,#9449);
#7461=LINE('',#66565,#9450);
#7462=LINE('',#66566,#9451);
#7463=LINE('',#66569,#9452);
#7464=LINE('',#66570,#9453);
#7465=LINE('',#66573,#9454);
#7466=LINE('',#66574,#9455);
#7467=LINE('',#66577,#9456);
#7468=LINE('',#66578,#9457);
#7469=LINE('',#66581,#9458);
#7470=LINE('',#66582,#9459);
#7471=LINE('',#66584,#9460);
#7472=VECTOR('',#28764,3.4);
#7473=VECTOR('',#28771,3.4);
#7474=VECTOR('',#28778,2.99999999999999);
#7475=VECTOR('',#28785,2.99999999999999);
#7476=VECTOR('',#28790,1000.);
#7477=VECTOR('',#28791,1000.);
#7478=VECTOR('',#28792,1000.);
#7479=VECTOR('',#28793,1000.);
#7480=VECTOR('',#28796,1000.);
#7481=VECTOR('',#28797,1000.);
#7482=VECTOR('',#28798,1000.);
#7483=VECTOR('',#28801,1000.);
#7484=VECTOR('',#28802,1000.);
#7485=VECTOR('',#28803,1000.);
#7486=VECTOR('',#28806,1000.);
#7487=VECTOR('',#28807,1000.);
#7488=VECTOR('',#28810,1000.);
#7489=VECTOR('',#28811,1000.);
#7490=VECTOR('',#28812,1000.);
#7491=VECTOR('',#28813,1000.);
#7492=VECTOR('',#28814,1000.);
#7493=VECTOR('',#28815,1000.);
#7494=VECTOR('',#28816,1000.);
#7495=VECTOR('',#28817,1000.);
#7496=VECTOR('',#28820,1000.);
#7497=VECTOR('',#28821,1000.);
#7498=VECTOR('',#28822,1000.);
#7499=VECTOR('',#28823,1000.);
#7500=VECTOR('',#28824,1000.);
#7501=VECTOR('',#28825,1000.);
#7502=VECTOR('',#28826,1000.);
#7503=VECTOR('',#28827,1000.);
#7504=VECTOR('',#28830,1000.);
#7505=VECTOR('',#28831,1000.);
#7506=VECTOR('',#28834,1000.);
#7507=VECTOR('',#28837,1000.);
#7508=VECTOR('',#28842,1000.);
#7509=VECTOR('',#28843,1000.);
#7510=VECTOR('',#28846,1000.);
#7511=VECTOR('',#28849,1000.);
#7512=VECTOR('',#28860,3.);
#7513=VECTOR('',#28867,3.);
#7514=VECTOR('',#28874,4.25000000000001);
#7515=VECTOR('',#28881,4.25000000000001);
#7516=VECTOR('',#28886,1000.);
#7517=VECTOR('',#28887,1000.);
#7518=VECTOR('',#28888,1000.);
#7519=VECTOR('',#28889,1000.);
#7520=VECTOR('',#28892,1000.);
#7521=VECTOR('',#28893,1000.);
#7522=VECTOR('',#28894,1000.);
#7523=VECTOR('',#28895,1000.);
#7524=VECTOR('',#28896,1000.);
#7525=VECTOR('',#28899,1000.);
#7526=VECTOR('',#28900,1000.);
#7527=VECTOR('',#28901,1000.);
#7528=VECTOR('',#28902,1000.);
#7529=VECTOR('',#28905,1000.);
#7530=VECTOR('',#28906,1000.);
#7531=VECTOR('',#28907,1000.);
#7532=VECTOR('',#28908,1000.);
#7533=VECTOR('',#28909,1000.);
#7534=VECTOR('',#28912,1000.);
#7535=VECTOR('',#28913,1000.);
#7536=VECTOR('',#28914,1000.);
#7537=VECTOR('',#28915,1000.);
#7538=VECTOR('',#28918,1000.);
#7539=VECTOR('',#28919,1000.);
#7540=VECTOR('',#28924,1000.);
#7541=VECTOR('',#28925,1000.);
#7542=VECTOR('',#28928,1000.);
#7543=VECTOR('',#28931,1000.);
#7544=VECTOR('',#28932,1000.);
#7545=VECTOR('',#28935,1000.);
#7546=VECTOR('',#28944,2.1);
#7547=VECTOR('',#28951,2.1);
#7548=VECTOR('',#28958,2.1);
#7549=VECTOR('',#28965,2.1);
#7550=VECTOR('',#28972,3.);
#7551=VECTOR('',#28979,3.);
#7552=VECTOR('',#28986,5.5);
#7553=VECTOR('',#28993,3.3);
#7554=VECTOR('',#29000,5.5);
#7555=VECTOR('',#29007,3.3);
#7556=VECTOR('',#29014,17.5);
#7557=VECTOR('',#29021,35.);
#7558=VECTOR('',#29026,1000.);
#7559=VECTOR('',#29027,1000.);
#7560=VECTOR('',#29028,1000.);
#7561=VECTOR('',#29029,1000.);
#7562=VECTOR('',#29032,1000.);
#7563=VECTOR('',#29033,1000.);
#7564=VECTOR('',#29034,1000.);
#7565=VECTOR('',#29037,1000.);
#7566=VECTOR('',#29038,1000.);
#7567=VECTOR('',#29041,1000.);
#7568=VECTOR('',#29042,1000.);
#7569=VECTOR('',#29045,1000.);
#7570=VECTOR('',#29062,2.1);
#7571=VECTOR('',#29069,2.1);
#7572=VECTOR('',#29076,2.1);
#7573=VECTOR('',#29083,2.1);
#7574=VECTOR('',#29090,2.1);
#7575=VECTOR('',#29097,2.1);
#7576=VECTOR('',#29104,18.);
#7577=VECTOR('',#29109,1000.);
#7578=VECTOR('',#29112,1000.);
#7579=VECTOR('',#29113,1000.);
#7580=VECTOR('',#29114,1000.);
#7581=VECTOR('',#29119,1000.);
#7582=VECTOR('',#29120,1000.);
#7583=VECTOR('',#29121,1000.);
#7584=VECTOR('',#29124,1000.);
#7585=VECTOR('',#29129,1000.);
#7586=VECTOR('',#29130,1000.);
#7587=VECTOR('',#29133,1000.);
#7588=VECTOR('',#29134,1000.);
#7589=VECTOR('',#29137,1000.);
#7590=VECTOR('',#29140,1000.);
#7591=VECTOR('',#29151,2.99999999999999);
#7592=VECTOR('',#29158,2.99999999999999);
#7593=VECTOR('',#29165,3.3);
#7594=VECTOR('',#29172,3.3);
#7595=VECTOR('',#29179,3.3);
#7596=VECTOR('',#29186,3.3);
#7597=VECTOR('',#29191,1000.);
#7598=VECTOR('',#29192,1000.);
#7599=VECTOR('',#29193,1000.);
#7600=VECTOR('',#29194,1000.);
#7601=VECTOR('',#29197,1000.);
#7602=VECTOR('',#29198,1000.);
#7603=VECTOR('',#29199,1000.);
#7604=VECTOR('',#29202,1000.);
#7605=VECTOR('',#29203,1000.);
#7606=VECTOR('',#29204,1000.);
#7607=VECTOR('',#29207,1000.);
#7608=VECTOR('',#29208,1000.);
#7609=VECTOR('',#29223,3.3);
#7610=VECTOR('',#29230,3.3);
#7611=VECTOR('',#29237,3.3);
#7612=VECTOR('',#29244,3.3);
#7613=VECTOR('',#29251,3.3);
#7614=VECTOR('',#29258,3.3);
#7615=VECTOR('',#29263,1000.);
#7616=VECTOR('',#29264,1000.);
#7617=VECTOR('',#29265,1000.);
#7618=VECTOR('',#29266,1000.);
#7619=VECTOR('',#29269,1000.);
#7620=VECTOR('',#29270,1000.);
#7621=VECTOR('',#29271,1000.);
#7622=VECTOR('',#29274,1000.);
#7623=VECTOR('',#29275,1000.);
#7624=VECTOR('',#29276,1000.);
#7625=VECTOR('',#29279,1000.);
#7626=VECTOR('',#29280,1000.);
#7627=VECTOR('',#29293,5.49999999999995);
#7628=VECTOR('',#29308,3.49999999999995);
#7629=VECTOR('',#29323,5.49999999999995);
#7630=VECTOR('',#29338,3.49999999999995);
#7631=VECTOR('',#29353,5.49999999999995);
#7632=VECTOR('',#29368,3.49999999999995);
#7633=VECTOR('',#29383,5.49999999999995);
#7634=VECTOR('',#29398,3.49999999999995);
#7635=VECTOR('',#29413,5.49999999999995);
#7636=VECTOR('',#29428,3.49999999999995);
#7637=VECTOR('',#29443,5.49999999999995);
#7638=VECTOR('',#29458,3.49999999999995);
#7639=VECTOR('',#29473,5.50000000000001);
#7640=VECTOR('',#29488,3.5);
#7641=VECTOR('',#29503,5.50000000000001);
#7642=VECTOR('',#29518,3.5);
#7643=VECTOR('',#29533,5.50000000000001);
#7644=VECTOR('',#29548,3.5);
#7645=VECTOR('',#29563,5.50000000000001);
#7646=VECTOR('',#29578,3.5);
#7647=VECTOR('',#29593,5.50000000000001);
#7648=VECTOR('',#29608,3.5);
#7649=VECTOR('',#29623,5.50000000000001);
#7650=VECTOR('',#29638,3.5);
#7651=VECTOR('',#29653,5.50000000000001);
#7652=VECTOR('',#29668,3.5);
#7653=VECTOR('',#29683,5.5);
#7654=VECTOR('',#29698,3.5);
#7655=VECTOR('',#29713,5.5);
#7656=VECTOR('',#29728,3.5);
#7657=VECTOR('',#29741,1000.);
#7658=VECTOR('',#29742,1000.);
#7659=VECTOR('',#29743,1000.);
#7660=VECTOR('',#29746,1000.);
#7661=VECTOR('',#29747,1000.);
#7662=VECTOR('',#29750,1000.);
#7663=VECTOR('',#29751,1000.);
#7664=VECTOR('',#29752,1000.);
#7665=VECTOR('',#29753,1000.);
#7666=VECTOR('',#29754,1000.);
#7667=VECTOR('',#29755,1000.);
#7668=VECTOR('',#29756,1000.);
#7669=VECTOR('',#29757,1000.);
#7670=VECTOR('',#29758,1000.);
#7671=VECTOR('',#29759,1000.);
#7672=VECTOR('',#29760,1000.);
#7673=VECTOR('',#29761,1000.);
#7674=VECTOR('',#29762,1000.);
#7675=VECTOR('',#29763,1000.);
#7676=VECTOR('',#29764,1000.);
#7677=VECTOR('',#29765,1000.);
#7678=VECTOR('',#29766,1000.);
#7679=VECTOR('',#29767,1000.);
#7680=VECTOR('',#29770,1000.);
#7681=VECTOR('',#29773,1000.);
#7682=VECTOR('',#29774,1000.);
#7683=VECTOR('',#29775,1000.);
#7684=VECTOR('',#29776,1000.);
#7685=VECTOR('',#29777,1000.);
#7686=VECTOR('',#29778,1000.);
#7687=VECTOR('',#29779,1000.);
#7688=VECTOR('',#29780,1000.);
#7689=VECTOR('',#29781,1000.);
#7690=VECTOR('',#29782,1000.);
#7691=VECTOR('',#29783,1000.);
#7692=VECTOR('',#29784,1000.);
#7693=VECTOR('',#29785,1000.);
#7694=VECTOR('',#29786,1000.);
#7695=VECTOR('',#29787,1000.);
#7696=VECTOR('',#29788,1000.);
#7697=VECTOR('',#29789,1000.);
#7698=VECTOR('',#29790,1000.);
#7699=VECTOR('',#29795,1000.);
#7700=VECTOR('',#29796,1000.);
#7701=VECTOR('',#29803,1000.);
#7702=VECTOR('',#29804,1000.);
#7703=VECTOR('',#29811,1000.);
#7704=VECTOR('',#29812,1000.);
#7705=VECTOR('',#29819,1000.);
#7706=VECTOR('',#29820,1000.);
#7707=VECTOR('',#29827,1000.);
#7708=VECTOR('',#29828,1000.);
#7709=VECTOR('',#29835,1000.);
#7710=VECTOR('',#29836,1000.);
#7711=VECTOR('',#29843,1000.);
#7712=VECTOR('',#29844,1000.);
#7713=VECTOR('',#29851,1000.);
#7714=VECTOR('',#29852,1000.);
#7715=VECTOR('',#29859,1000.);
#7716=VECTOR('',#29860,1000.);
#7717=VECTOR('',#29865,1000.);
#7718=VECTOR('',#29866,1000.);
#7719=VECTOR('',#29875,1000.);
#7720=VECTOR('',#29876,1000.);
#7721=VECTOR('',#29883,1000.);
#7722=VECTOR('',#29884,1000.);
#7723=VECTOR('',#29889,1000.);
#7724=VECTOR('',#29890,1000.);
#7725=VECTOR('',#29897,1000.);
#7726=VECTOR('',#29898,1000.);
#7727=VECTOR('',#29899,1000.);
#7728=VECTOR('',#29904,1000.);
#7729=VECTOR('',#29907,1000.);
#7730=VECTOR('',#29908,1000.);
#7731=VECTOR('',#29911,1000.);
#7732=VECTOR('',#29914,1000.);
#7733=VECTOR('',#29917,1000.);
#7734=VECTOR('',#29924,1000.);
#7735=VECTOR('',#29927,1000.);
#7736=VECTOR('',#29930,1000.);
#7737=VECTOR('',#29937,1000.);
#7738=VECTOR('',#29938,1000.);
#7739=VECTOR('',#29939,1000.);
#7740=VECTOR('',#29946,1000.);
#7741=VECTOR('',#29949,1000.);
#7742=VECTOR('',#29952,1000.);
#7743=VECTOR('',#29959,1000.);
#7744=VECTOR('',#29962,1000.);
#7745=VECTOR('',#29965,1000.);
#7746=VECTOR('',#29968,1000.);
#7747=VECTOR('',#29969,1000.);
#7748=VECTOR('',#29970,1000.);
#7749=VECTOR('',#29971,1000.);
#7750=VECTOR('',#29974,1000.);
#7751=VECTOR('',#29975,1000.);
#7752=VECTOR('',#29976,1000.);
#7753=VECTOR('',#29979,1000.);
#7754=VECTOR('',#29982,1000.);
#7755=VECTOR('',#29985,1000.);
#7756=VECTOR('',#29992,1000.);
#7757=VECTOR('',#29995,1000.);
#7758=VECTOR('',#29998,1000.);
#7759=VECTOR('',#30005,1000.);
#7760=VECTOR('',#30006,1000.);
#7761=VECTOR('',#30007,1000.);
#7762=VECTOR('',#30014,1000.);
#7763=VECTOR('',#30017,1000.);
#7764=VECTOR('',#30020,1000.);
#7765=VECTOR('',#30027,1000.);
#7766=VECTOR('',#30030,1000.);
#7767=VECTOR('',#30033,1000.);
#7768=VECTOR('',#30036,1000.);
#7769=VECTOR('',#30037,1000.);
#7770=VECTOR('',#30040,1000.);
#7771=VECTOR('',#30041,1000.);
#7772=VECTOR('',#30044,1000.);
#7773=VECTOR('',#30045,1000.);
#7774=VECTOR('',#30048,1000.);
#7775=VECTOR('',#30049,1000.);
#7776=VECTOR('',#30052,1000.);
#7777=VECTOR('',#30053,1000.);
#7778=VECTOR('',#30056,1000.);
#7779=VECTOR('',#30057,1000.);
#7780=VECTOR('',#30060,1000.);
#7781=VECTOR('',#30061,1000.);
#7782=VECTOR('',#30064,1000.);
#7783=VECTOR('',#30067,1000.);
#7784=VECTOR('',#30070,1000.);
#7785=VECTOR('',#30073,1000.);
#7786=VECTOR('',#30074,1000.);
#7787=VECTOR('',#30077,1000.);
#7788=VECTOR('',#30078,1000.);
#7789=VECTOR('',#30081,1000.);
#7790=VECTOR('',#30082,1000.);
#7791=VECTOR('',#30085,1000.);
#7792=VECTOR('',#30086,1000.);
#7793=VECTOR('',#30089,1000.);
#7794=VECTOR('',#30092,1000.);
#7795=VECTOR('',#30093,1000.);
#7796=VECTOR('',#30096,1000.);
#7797=VECTOR('',#30097,1000.);
#7798=VECTOR('',#30118,1000.);
#7799=VECTOR('',#30119,1000.);
#7800=VECTOR('',#30122,1000.);
#7801=VECTOR('',#30123,1000.);
#7802=VECTOR('',#30126,1000.);
#7803=VECTOR('',#30127,1000.);
#7804=VECTOR('',#30130,1000.);
#7805=VECTOR('',#30131,1000.);
#7806=VECTOR('',#30136,1000.);
#7807=VECTOR('',#30137,1000.);
#7808=VECTOR('',#30140,1000.);
#7809=VECTOR('',#30141,1000.);
#7810=VECTOR('',#30164,1000.);
#7811=VECTOR('',#30203,2.5);
#7812=VECTOR('',#30210,2.5);
#7813=VECTOR('',#30217,3.65);
#7814=VECTOR('',#30222,2.5);
#7815=VECTOR('',#30225,2.5);
#7816=VECTOR('',#30230,3.32349999999999);
#7817=VECTOR('',#30237,3.3235);
#7818=VECTOR('',#30244,3.32349999999999);
#7819=VECTOR('',#30251,3.3235);
#7820=VECTOR('',#30258,2.5);
#7821=VECTOR('',#30265,2.5);
#7822=VECTOR('',#30272,3.65);
#7823=VECTOR('',#30279,0.500000000000006);
#7824=VECTOR('',#30282,1000.);
#7825=VECTOR('',#30285,1000.);
#7826=VECTOR('',#30288,2.5);
#7827=VECTOR('',#30291,2.5);
#7828=VECTOR('',#30296,0.5);
#7829=VECTOR('',#30297,1000.);
#7830=VECTOR('',#30300,1000.);
#7831=VECTOR('',#30311,4.);
#7832=VECTOR('',#30316,4.99995);
#7833=VECTOR('',#30323,1000.);
#7834=VECTOR('',#30324,1000.);
#7835=VECTOR('',#30325,1000.);
#7836=VECTOR('',#30330,1000.);
#7837=VECTOR('',#30333,1000.);
#7838=VECTOR('',#30338,1000.);
#7839=VECTOR('',#30341,1000.);
#7840=VECTOR('',#30346,1000.);
#7841=VECTOR('',#30347,1000.);
#7842=VECTOR('',#30348,1000.);
#7843=VECTOR('',#30351,1000.);
#7844=VECTOR('',#30352,1000.);
#7845=VECTOR('',#30353,1000.);
#7846=VECTOR('',#30354,1000.);
#7847=VECTOR('',#30357,1000.);
#7848=VECTOR('',#30358,1000.);
#7849=VECTOR('',#30359,1000.);
#7850=VECTOR('',#30360,1000.);
#7851=VECTOR('',#30363,1000.);
#7852=VECTOR('',#30364,1000.);
#7853=VECTOR('',#30365,1000.);
#7854=VECTOR('',#30366,1000.);
#7855=VECTOR('',#30369,1000.);
#7856=VECTOR('',#30370,1000.);
#7857=VECTOR('',#30371,1000.);
#7858=VECTOR('',#30372,1000.);
#7859=VECTOR('',#30375,1000.);
#7860=VECTOR('',#30376,1000.);
#7861=VECTOR('',#30377,1000.);
#7862=VECTOR('',#30378,1000.);
#7863=VECTOR('',#30381,1000.);
#7864=VECTOR('',#30382,1000.);
#7865=VECTOR('',#30383,1000.);
#7866=VECTOR('',#30384,1000.);
#7867=VECTOR('',#30387,1000.);
#7868=VECTOR('',#30388,1000.);
#7869=VECTOR('',#30389,1000.);
#7870=VECTOR('',#30390,1000.);
#7871=VECTOR('',#30393,1000.);
#7872=VECTOR('',#30394,1000.);
#7873=VECTOR('',#30395,1000.);
#7874=VECTOR('',#30396,1000.);
#7875=VECTOR('',#30399,1000.);
#7876=VECTOR('',#30400,1000.);
#7877=VECTOR('',#30401,1000.);
#7878=VECTOR('',#30402,1000.);
#7879=VECTOR('',#30405,1000.);
#7880=VECTOR('',#30406,1000.);
#7881=VECTOR('',#30407,1000.);
#7882=VECTOR('',#30410,1000.);
#7883=VECTOR('',#30411,1000.);
#7884=VECTOR('',#30412,1000.);
#7885=VECTOR('',#30413,1000.);
#7886=VECTOR('',#30416,1000.);
#7887=VECTOR('',#30417,1000.);
#7888=VECTOR('',#30418,1000.);
#7889=VECTOR('',#30421,1000.);
#7890=VECTOR('',#30422,1000.);
#7891=VECTOR('',#30423,1000.);
#7892=VECTOR('',#30424,1000.);
#7893=VECTOR('',#30427,1000.);
#7894=VECTOR('',#30428,1000.);
#7895=VECTOR('',#30429,1000.);
#7896=VECTOR('',#30430,1000.);
#7897=VECTOR('',#30433,1000.);
#7898=VECTOR('',#30434,1000.);
#7899=VECTOR('',#30435,1000.);
#7900=VECTOR('',#30436,1000.);
#7901=VECTOR('',#30439,1000.);
#7902=VECTOR('',#30440,1000.);
#7903=VECTOR('',#30441,1000.);
#7904=VECTOR('',#30442,1000.);
#7905=VECTOR('',#30445,1000.);
#7906=VECTOR('',#30446,1000.);
#7907=VECTOR('',#30451,1000.);
#7908=VECTOR('',#30454,1000.);
#7909=VECTOR('',#30459,1000.);
#7910=VECTOR('',#30462,1000.);
#7911=VECTOR('',#30467,1000.);
#7912=VECTOR('',#30470,1000.);
#7913=VECTOR('',#30475,1000.);
#7914=VECTOR('',#30478,1000.);
#7915=VECTOR('',#30579,1000.);
#7916=VECTOR('',#30580,1000.);
#7917=VECTOR('',#30581,1000.);
#7918=VECTOR('',#30582,1000.);
#7919=VECTOR('',#30585,1000.);
#7920=VECTOR('',#30586,1000.);
#7921=VECTOR('',#30587,1000.);
#7922=VECTOR('',#30588,1000.);
#7923=VECTOR('',#30589,1000.);
#7924=VECTOR('',#30590,1000.);
#7925=VECTOR('',#30593,1000.);
#7926=VECTOR('',#30594,1000.);
#7927=VECTOR('',#30597,1000.);
#7928=VECTOR('',#30598,1000.);
#7929=VECTOR('',#30601,1000.);
#7930=VECTOR('',#30604,1000.);
#7931=VECTOR('',#30605,1000.);
#7932=VECTOR('',#30608,1000.);
#7933=VECTOR('',#30609,1000.);
#7934=VECTOR('',#30612,1000.);
#7935=VECTOR('',#30615,1000.);
#7936=VECTOR('',#30616,1000.);
#7937=VECTOR('',#30617,1000.);
#7938=VECTOR('',#30620,1000.);
#7939=VECTOR('',#30621,1000.);
#7940=VECTOR('',#30624,1000.);
#7941=VECTOR('',#30625,1000.);
#7942=VECTOR('',#30628,1000.);
#7943=VECTOR('',#30629,1000.);
#7944=VECTOR('',#30632,1000.);
#7945=VECTOR('',#30633,1000.);
#7946=VECTOR('',#30636,1000.);
#7947=VECTOR('',#30641,1000.);
#7948=VECTOR('',#30644,1000.);
#7949=VECTOR('',#30647,1000.);
#7950=VECTOR('',#30654,1000.);
#7951=VECTOR('',#30657,1000.);
#7952=VECTOR('',#30660,1000.);
#7953=VECTOR('',#30667,1000.);
#7954=VECTOR('',#30668,1000.);
#7955=VECTOR('',#30669,1000.);
#7956=VECTOR('',#30676,1000.);
#7957=VECTOR('',#30679,1000.);
#7958=VECTOR('',#30682,1000.);
#7959=VECTOR('',#30689,1000.);
#7960=VECTOR('',#30692,1000.);
#7961=VECTOR('',#30695,1000.);
#7962=VECTOR('',#30696,1000.);
#7963=VECTOR('',#30697,1000.);
#7964=VECTOR('',#30698,1000.);
#7965=VECTOR('',#30699,1000.);
#7966=VECTOR('',#30700,1000.);
#7967=VECTOR('',#30701,1000.);
#7968=VECTOR('',#30702,1000.);
#7969=VECTOR('',#30703,1000.);
#7970=VECTOR('',#30704,1000.);
#7971=VECTOR('',#30707,1000.);
#7972=VECTOR('',#30708,1000.);
#7973=VECTOR('',#30709,1000.);
#7974=VECTOR('',#30714,1000.);
#7975=VECTOR('',#30717,1000.);
#7976=VECTOR('',#30718,1000.);
#7977=VECTOR('',#30723,1000.);
#7978=VECTOR('',#30726,1000.);
#7979=VECTOR('',#30727,1000.);
#7980=VECTOR('',#30732,1000.);
#7981=VECTOR('',#30737,1000.);
#7982=VECTOR('',#30742,1000.);
#7983=VECTOR('',#30745,1000.);
#7984=VECTOR('',#30746,1000.);
#7985=VECTOR('',#30751,1000.);
#7986=VECTOR('',#30754,1000.);
#7987=VECTOR('',#30755,1000.);
#7988=VECTOR('',#30760,1000.);
#7989=VECTOR('',#30763,1000.);
#7990=VECTOR('',#30764,1000.);
#7991=VECTOR('',#30769,1000.);
#7992=VECTOR('',#30774,1000.);
#7993=VECTOR('',#30779,1000.);
#7994=VECTOR('',#30782,1000.);
#7995=VECTOR('',#30783,1000.);
#7996=VECTOR('',#30786,1000.);
#7997=VECTOR('',#30787,1000.);
#7998=VECTOR('',#30790,1000.);
#7999=VECTOR('',#30791,1000.);
#8000=VECTOR('',#30796,1000.);
#8001=VECTOR('',#30801,1000.);
#8002=VECTOR('',#30806,1000.);
#8003=VECTOR('',#30809,1000.);
#8004=VECTOR('',#30810,1000.);
#8005=VECTOR('',#30815,1000.);
#8006=VECTOR('',#30818,1000.);
#8007=VECTOR('',#30819,1000.);
#8008=VECTOR('',#30824,1000.);
#8009=VECTOR('',#30827,1000.);
#8010=VECTOR('',#30828,1000.);
#8011=VECTOR('',#30833,1000.);
#8012=VECTOR('',#30838,1000.);
#8013=VECTOR('',#30843,1000.);
#8014=VECTOR('',#30846,1000.);
#8015=VECTOR('',#30847,1000.);
#8016=VECTOR('',#30852,1000.);
#8017=VECTOR('',#30855,1000.);
#8018=VECTOR('',#30856,1000.);
#8019=VECTOR('',#30861,1000.);
#8020=VECTOR('',#30864,1000.);
#8021=VECTOR('',#30865,1000.);
#8022=VECTOR('',#30868,1000.);
#8023=VECTOR('',#30869,1000.);
#8024=VECTOR('',#30872,1000.);
#8025=VECTOR('',#30873,1000.);
#8026=VECTOR('',#30876,1000.);
#8027=VECTOR('',#30877,1000.);
#8028=VECTOR('',#30880,1000.);
#8029=VECTOR('',#30881,1000.);
#8030=VECTOR('',#30884,1000.);
#8031=VECTOR('',#30885,1000.);
#8032=VECTOR('',#30888,1000.);
#8033=VECTOR('',#30889,1000.);
#8034=VECTOR('',#30892,1000.);
#8035=VECTOR('',#30893,1000.);
#8036=VECTOR('',#30896,1000.);
#8037=VECTOR('',#30897,1000.);
#8038=VECTOR('',#30900,1000.);
#8039=VECTOR('',#30905,1000.);
#8040=VECTOR('',#30908,1000.);
#8041=VECTOR('',#30911,1000.);
#8042=VECTOR('',#30912,1000.);
#8043=VECTOR('',#30915,1000.);
#8044=VECTOR('',#30916,1000.);
#8045=VECTOR('',#30917,1000.);
#8046=VECTOR('',#30918,1000.);
#8047=VECTOR('',#30919,1000.);
#8048=VECTOR('',#30920,1000.);
#8049=VECTOR('',#30921,1000.);
#8050=VECTOR('',#30924,1000.);
#8051=VECTOR('',#30927,1000.);
#8052=VECTOR('',#30934,1000.);
#8053=VECTOR('',#30937,1000.);
#8054=VECTOR('',#30940,1000.);
#8055=VECTOR('',#30947,1000.);
#8056=VECTOR('',#30948,1000.);
#8057=VECTOR('',#30949,1000.);
#8058=VECTOR('',#30956,1000.);
#8059=VECTOR('',#30959,1000.);
#8060=VECTOR('',#30962,1000.);
#8061=VECTOR('',#30969,1000.);
#8062=VECTOR('',#30972,1000.);
#8063=VECTOR('',#30975,1000.);
#8064=VECTOR('',#30976,1000.);
#8065=VECTOR('',#30977,1000.);
#8066=VECTOR('',#30978,1000.);
#8067=VECTOR('',#30979,1000.);
#8068=VECTOR('',#30982,1000.);
#8069=VECTOR('',#30983,1000.);
#8070=VECTOR('',#30986,1000.);
#8071=VECTOR('',#30987,1000.);
#8072=VECTOR('',#30996,1000.);
#8073=VECTOR('',#30999,1000.);
#8074=VECTOR('',#31002,1000.);
#8075=VECTOR('',#31003,1000.);
#8076=VECTOR('',#31004,1000.);
#8077=VECTOR('',#31007,1000.);
#8078=VECTOR('',#31008,1000.);
#8079=VECTOR('',#31011,1000.);
#8080=VECTOR('',#31012,1000.);
#8081=VECTOR('',#31015,1000.);
#8082=VECTOR('',#31016,1000.);
#8083=VECTOR('',#31019,1000.);
#8084=VECTOR('',#31020,1000.);
#8085=VECTOR('',#31021,1000.);
#8086=VECTOR('',#31022,1000.);
#8087=VECTOR('',#31023,1000.);
#8088=VECTOR('',#31026,1000.);
#8089=VECTOR('',#31027,1000.);
#8090=VECTOR('',#31030,1000.);
#8091=VECTOR('',#31031,1000.);
#8092=VECTOR('',#31034,1000.);
#8093=VECTOR('',#31035,1000.);
#8094=VECTOR('',#31038,1000.);
#8095=VECTOR('',#31039,1000.);
#8096=VECTOR('',#31042,1000.);
#8097=VECTOR('',#31043,1000.);
#8098=VECTOR('',#31048,1000.);
#8099=VECTOR('',#31051,1000.);
#8100=VECTOR('',#31052,1000.);
#8101=VECTOR('',#31057,1000.);
#8102=VECTOR('',#31060,1000.);
#8103=VECTOR('',#31061,1000.);
#8104=VECTOR('',#31066,1000.);
#8105=VECTOR('',#31071,1000.);
#8106=VECTOR('',#31076,1000.);
#8107=VECTOR('',#31079,1000.);
#8108=VECTOR('',#31080,1000.);
#8109=VECTOR('',#31085,1000.);
#8110=VECTOR('',#31088,1000.);
#8111=VECTOR('',#31089,1000.);
#8112=VECTOR('',#31094,1000.);
#8113=VECTOR('',#31097,1000.);
#8114=VECTOR('',#31098,1000.);
#8115=VECTOR('',#31103,1000.);
#8116=VECTOR('',#31108,1000.);
#8117=VECTOR('',#31113,1000.);
#8118=VECTOR('',#31116,1000.);
#8119=VECTOR('',#31117,1000.);
#8120=VECTOR('',#31120,1000.);
#8121=VECTOR('',#31121,1000.);
#8122=VECTOR('',#31124,1000.);
#8123=VECTOR('',#31125,1000.);
#8124=VECTOR('',#31130,1000.);
#8125=VECTOR('',#31135,1000.);
#8126=VECTOR('',#31140,1000.);
#8127=VECTOR('',#31143,1000.);
#8128=VECTOR('',#31144,1000.);
#8129=VECTOR('',#31149,1000.);
#8130=VECTOR('',#31152,1000.);
#8131=VECTOR('',#31153,1000.);
#8132=VECTOR('',#31158,1000.);
#8133=VECTOR('',#31161,1000.);
#8134=VECTOR('',#31162,1000.);
#8135=VECTOR('',#31167,1000.);
#8136=VECTOR('',#31172,1000.);
#8137=VECTOR('',#31177,1000.);
#8138=VECTOR('',#31180,1000.);
#8139=VECTOR('',#31181,1000.);
#8140=VECTOR('',#31186,1000.);
#8141=VECTOR('',#31189,1000.);
#8142=VECTOR('',#31190,1000.);
#8143=VECTOR('',#31195,1000.);
#8144=VECTOR('',#31198,1000.);
#8145=VECTOR('',#31203,1000.);
#8146=VECTOR('',#31204,1000.);
#8147=VECTOR('',#31205,1000.);
#8148=VECTOR('',#31206,1000.);
#8149=VECTOR('',#31209,1000.);
#8150=VECTOR('',#31210,1000.);
#8151=VECTOR('',#31211,1000.);
#8152=VECTOR('',#31212,1000.);
#8153=VECTOR('',#31215,1000.);
#8154=VECTOR('',#31216,1000.);
#8155=VECTOR('',#31219,1000.);
#8156=VECTOR('',#31220,1000.);
#8157=VECTOR('',#31231,1000.);
#8158=VECTOR('',#31234,1000.);
#8159=VECTOR('',#31235,1000.);
#8160=VECTOR('',#31236,1000.);
#8161=VECTOR('',#31237,1000.);
#8162=VECTOR('',#31240,1000.);
#8163=VECTOR('',#31241,1000.);
#8164=VECTOR('',#31242,1000.);
#8165=VECTOR('',#31245,1000.);
#8166=VECTOR('',#31246,1000.);
#8167=VECTOR('',#31247,1000.);
#8168=VECTOR('',#31248,1000.);
#8169=VECTOR('',#31251,1000.);
#8170=VECTOR('',#31254,1000.);
#8171=VECTOR('',#31255,1000.);
#8172=VECTOR('',#31258,1000.);
#8173=VECTOR('',#31263,1000.);
#8174=VECTOR('',#31264,1000.);
#8175=VECTOR('',#31265,1000.);
#8176=VECTOR('',#31266,1000.);
#8177=VECTOR('',#31267,1000.);
#8178=VECTOR('',#31268,1000.);
#8179=VECTOR('',#31269,1000.);
#8180=VECTOR('',#31270,1000.);
#8181=VECTOR('',#31271,1000.);
#8182=VECTOR('',#31272,1000.);
#8183=VECTOR('',#31275,1000.);
#8184=VECTOR('',#31278,1000.);
#8185=VECTOR('',#31285,1000.);
#8186=VECTOR('',#31288,1000.);
#8187=VECTOR('',#31291,1000.);
#8188=VECTOR('',#31298,1000.);
#8189=VECTOR('',#31299,1000.);
#8190=VECTOR('',#31300,1000.);
#8191=VECTOR('',#31307,1000.);
#8192=VECTOR('',#31310,1000.);
#8193=VECTOR('',#31313,1000.);
#8194=VECTOR('',#31320,1000.);
#8195=VECTOR('',#31323,1000.);
#8196=VECTOR('',#31326,1000.);
#8197=VECTOR('',#31329,1000.);
#8198=VECTOR('',#31330,1000.);
#8199=VECTOR('',#31333,1000.);
#8200=VECTOR('',#31334,1000.);
#8201=VECTOR('',#31337,1000.);
#8202=VECTOR('',#31338,1000.);
#8203=VECTOR('',#31339,1000.);
#8204=VECTOR('',#31342,1000.);
#8205=VECTOR('',#31343,1000.);
#8206=VECTOR('',#31344,1000.);
#8207=VECTOR('',#31347,1000.);
#8208=VECTOR('',#31348,1000.);
#8209=VECTOR('',#31349,1000.);
#8210=VECTOR('',#31352,1000.);
#8211=VECTOR('',#31353,1000.);
#8212=VECTOR('',#31354,1000.);
#8213=VECTOR('',#31367,1000.);
#8214=VECTOR('',#31368,1000.);
#8215=VECTOR('',#31369,1000.);
#8216=VECTOR('',#31372,1000.);
#8217=VECTOR('',#31373,1000.);
#8218=VECTOR('',#31374,1000.);
#8219=VECTOR('',#31379,1000.);
#8220=VECTOR('',#31380,1000.);
#8221=VECTOR('',#31383,1000.);
#8222=VECTOR('',#31384,1000.);
#8223=VECTOR('',#31385,1000.);
#8224=VECTOR('',#31388,1000.);
#8225=VECTOR('',#31389,1000.);
#8226=VECTOR('',#31396,1000.);
#8227=VECTOR('',#31397,1000.);
#8228=VECTOR('',#31406,1000.);
#8229=VECTOR('',#31407,1000.);
#8230=VECTOR('',#31408,1000.);
#8231=VECTOR('',#31411,1000.);
#8232=VECTOR('',#31412,1000.);
#8233=VECTOR('',#31415,1000.);
#8234=VECTOR('',#31416,1000.);
#8235=VECTOR('',#31419,1000.);
#8236=VECTOR('',#31420,1000.);
#8237=VECTOR('',#31423,1000.);
#8238=VECTOR('',#31424,1000.);
#8239=VECTOR('',#31427,1000.);
#8240=VECTOR('',#31428,1000.);
#8241=VECTOR('',#31431,1000.);
#8242=VECTOR('',#31432,1000.);
#8243=VECTOR('',#31435,1000.);
#8244=VECTOR('',#31436,1000.);
#8245=VECTOR('',#31439,1000.);
#8246=VECTOR('',#31440,1000.);
#8247=VECTOR('',#31443,1000.);
#8248=VECTOR('',#31444,1000.);
#8249=VECTOR('',#31449,1000.);
#8250=VECTOR('',#31452,1000.);
#8251=VECTOR('',#31453,1000.);
#8252=VECTOR('',#31458,1000.);
#8253=VECTOR('',#31461,1000.);
#8254=VECTOR('',#31462,1000.);
#8255=VECTOR('',#31467,1000.);
#8256=VECTOR('',#31472,1000.);
#8257=VECTOR('',#31477,1000.);
#8258=VECTOR('',#31480,1000.);
#8259=VECTOR('',#31481,1000.);
#8260=VECTOR('',#31486,1000.);
#8261=VECTOR('',#31489,1000.);
#8262=VECTOR('',#31490,1000.);
#8263=VECTOR('',#31495,1000.);
#8264=VECTOR('',#31498,1000.);
#8265=VECTOR('',#31499,1000.);
#8266=VECTOR('',#31504,1000.);
#8267=VECTOR('',#31509,1000.);
#8268=VECTOR('',#31514,1000.);
#8269=VECTOR('',#31517,1000.);
#8270=VECTOR('',#31518,1000.);
#8271=VECTOR('',#31521,1000.);
#8272=VECTOR('',#31522,1000.);
#8273=VECTOR('',#31525,1000.);
#8274=VECTOR('',#31526,1000.);
#8275=VECTOR('',#31531,1000.);
#8276=VECTOR('',#31536,1000.);
#8277=VECTOR('',#31541,1000.);
#8278=VECTOR('',#31544,1000.);
#8279=VECTOR('',#31545,1000.);
#8280=VECTOR('',#31550,1000.);
#8281=VECTOR('',#31553,1000.);
#8282=VECTOR('',#31554,1000.);
#8283=VECTOR('',#31559,1000.);
#8284=VECTOR('',#31562,1000.);
#8285=VECTOR('',#31563,1000.);
#8286=VECTOR('',#31568,1000.);
#8287=VECTOR('',#31573,1000.);
#8288=VECTOR('',#31578,1000.);
#8289=VECTOR('',#31581,1000.);
#8290=VECTOR('',#31582,1000.);
#8291=VECTOR('',#31587,1000.);
#8292=VECTOR('',#31590,1000.);
#8293=VECTOR('',#31591,1000.);
#8294=VECTOR('',#31596,1000.);
#8295=VECTOR('',#31599,1000.);
#8296=VECTOR('',#31602,1000.);
#8297=VECTOR('',#31603,1000.);
#8298=VECTOR('',#31604,1000.);
#8299=VECTOR('',#31605,1000.);
#8300=VECTOR('',#31608,1000.);
#8301=VECTOR('',#31609,1000.);
#8302=VECTOR('',#31610,1000.);
#8303=VECTOR('',#31613,1000.);
#8304=VECTOR('',#31614,1000.);
#8305=VECTOR('',#31615,1000.);
#8306=VECTOR('',#31618,1000.);
#8307=VECTOR('',#31619,1000.);
#8308=VECTOR('',#31620,1000.);
#8309=VECTOR('',#31623,1000.);
#8310=VECTOR('',#31624,1000.);
#8311=VECTOR('',#31625,1000.);
#8312=VECTOR('',#31628,1000.);
#8313=VECTOR('',#31629,1000.);
#8314=VECTOR('',#31630,1000.);
#8315=VECTOR('',#31631,1000.);
#8316=VECTOR('',#31634,1000.);
#8317=VECTOR('',#31635,1000.);
#8318=VECTOR('',#31636,1000.);
#8319=VECTOR('',#31639,1000.);
#8320=VECTOR('',#31640,1000.);
#8321=VECTOR('',#31641,1000.);
#8322=VECTOR('',#31644,1000.);
#8323=VECTOR('',#31645,1000.);
#8324=VECTOR('',#31648,1000.);
#8325=VECTOR('',#31649,1000.);
#8326=VECTOR('',#31650,1000.);
#8327=VECTOR('',#31651,1000.);
#8328=VECTOR('',#31654,1000.);
#8329=VECTOR('',#31655,1000.);
#8330=VECTOR('',#31656,1000.);
#8331=VECTOR('',#31659,1000.);
#8332=VECTOR('',#31660,1000.);
#8333=VECTOR('',#31661,1000.);
#8334=VECTOR('',#31664,1000.);
#8335=VECTOR('',#31665,1000.);
#8336=VECTOR('',#31666,1000.);
#8337=VECTOR('',#31669,1000.);
#8338=VECTOR('',#31670,1000.);
#8339=VECTOR('',#31671,1000.);
#8340=VECTOR('',#31674,1000.);
#8341=VECTOR('',#31675,1000.);
#8342=VECTOR('',#31676,1000.);
#8343=VECTOR('',#31679,1000.);
#8344=VECTOR('',#31680,1000.);
#8345=VECTOR('',#31681,1000.);
#8346=VECTOR('',#31684,1000.);
#8347=VECTOR('',#31685,1000.);
#8348=VECTOR('',#31686,1000.);
#8349=VECTOR('',#31689,1000.);
#8350=VECTOR('',#31690,1000.);
#8351=VECTOR('',#31691,1000.);
#8352=VECTOR('',#31694,1000.);
#8353=VECTOR('',#31695,1000.);
#8354=VECTOR('',#31696,1000.);
#8355=VECTOR('',#31699,1000.);
#8356=VECTOR('',#31700,1000.);
#8357=VECTOR('',#31701,1000.);
#8358=VECTOR('',#31704,1000.);
#8359=VECTOR('',#31705,1000.);
#8360=VECTOR('',#31706,1000.);
#8361=VECTOR('',#31709,1000.);
#8362=VECTOR('',#31710,1000.);
#8363=VECTOR('',#31711,1000.);
#8364=VECTOR('',#31714,1000.);
#8365=VECTOR('',#31715,1000.);
#8366=VECTOR('',#31716,1000.);
#8367=VECTOR('',#31719,1000.);
#8368=VECTOR('',#31720,1000.);
#8369=VECTOR('',#31721,1000.);
#8370=VECTOR('',#31726,1000.);
#8371=VECTOR('',#31727,1000.);
#8372=VECTOR('',#31730,1000.);
#8373=VECTOR('',#31731,1000.);
#8374=VECTOR('',#31732,1000.);
#8375=VECTOR('',#31737,1000.);
#8376=VECTOR('',#31738,1000.);
#8377=VECTOR('',#31743,1000.);
#8378=VECTOR('',#31744,1000.);
#8379=VECTOR('',#31747,1000.);
#8380=VECTOR('',#31748,1000.);
#8381=VECTOR('',#31749,1000.);
#8382=VECTOR('',#31752,1000.);
#8383=VECTOR('',#31759,1000.);
#8384=VECTOR('',#31760,1000.);
#8385=VECTOR('',#31763,1000.);
#8386=VECTOR('',#31764,1000.);
#8387=VECTOR('',#31765,1000.);
#8388=VECTOR('',#31768,1000.);
#8389=VECTOR('',#31769,1000.);
#8390=VECTOR('',#31770,1000.);
#8391=VECTOR('',#31773,1000.);
#8392=VECTOR('',#31774,1000.);
#8393=VECTOR('',#31775,1000.);
#8394=VECTOR('',#31780,1000.);
#8395=VECTOR('',#31783,1000.);
#8396=VECTOR('',#31784,1000.);
#8397=VECTOR('',#31787,1000.);
#8398=VECTOR('',#31790,1000.);
#8399=VECTOR('',#31797,1000.);
#8400=VECTOR('',#31800,1000.);
#8401=VECTOR('',#31803,1000.);
#8402=VECTOR('',#31810,1000.);
#8403=VECTOR('',#31811,1000.);
#8404=VECTOR('',#31812,1000.);
#8405=VECTOR('',#31819,1000.);
#8406=VECTOR('',#31822,1000.);
#8407=VECTOR('',#31825,1000.);
#8408=VECTOR('',#31832,1000.);
#8409=VECTOR('',#31835,1000.);
#8410=VECTOR('',#31838,1000.);
#8411=VECTOR('',#31839,1000.);
#8412=VECTOR('',#31842,1000.);
#8413=VECTOR('',#31843,1000.);
#8414=VECTOR('',#31844,1000.);
#8415=VECTOR('',#31845,1000.);
#8416=VECTOR('',#31846,1000.);
#8417=VECTOR('',#31847,1000.);
#8418=VECTOR('',#31848,1000.);
#8419=VECTOR('',#31849,1000.);
#8420=VECTOR('',#31850,1000.);
#8421=VECTOR('',#31851,1000.);
#8422=VECTOR('',#31852,1000.);
#8423=VECTOR('',#31853,1000.);
#8424=VECTOR('',#31854,1000.);
#8425=VECTOR('',#31857,1000.);
#8426=VECTOR('',#31858,1000.);
#8427=VECTOR('',#31859,1000.);
#8428=VECTOR('',#31862,1000.);
#8429=VECTOR('',#31863,1000.);
#8430=VECTOR('',#31864,1000.);
#8431=VECTOR('',#31867,1000.);
#8432=VECTOR('',#31868,1000.);
#8433=VECTOR('',#31871,1000.);
#8434=VECTOR('',#31872,1000.);
#8435=VECTOR('',#31875,1000.);
#8436=VECTOR('',#31876,1000.);
#8437=VECTOR('',#31879,1000.);
#8438=VECTOR('',#31882,1000.);
#8439=VECTOR('',#31885,1000.);
#8440=VECTOR('',#31888,1000.);
#8441=VECTOR('',#31891,1000.);
#8442=VECTOR('',#31894,1000.);
#8443=VECTOR('',#31895,1000.);
#8444=VECTOR('',#31898,1000.);
#8445=VECTOR('',#31903,1000.);
#8446=VECTOR('',#31904,1000.);
#8447=VECTOR('',#31909,1000.);
#8448=VECTOR('',#31910,1000.);
#8449=VECTOR('',#31919,1000.);
#8450=VECTOR('',#31920,1000.);
#8451=VECTOR('',#31925,1000.);
#8452=VECTOR('',#31926,1000.);
#8453=VECTOR('',#31929,1000.);
#8454=VECTOR('',#31932,1000.);
#8455=VECTOR('',#31937,1000.);
#8456=VECTOR('',#31938,1000.);
#8457=VECTOR('',#31943,1000.);
#8458=VECTOR('',#31944,1000.);
#8459=VECTOR('',#31951,1000.);
#8460=VECTOR('',#31952,1000.);
#8461=VECTOR('',#31953,1000.);
#8462=VECTOR('',#31956,1000.);
#8463=VECTOR('',#31961,1000.);
#8464=VECTOR('',#31962,1000.);
#8465=VECTOR('',#31967,1000.);
#8466=VECTOR('',#31968,1000.);
#8467=VECTOR('',#31977,1000.);
#8468=VECTOR('',#31978,1000.);
#8469=VECTOR('',#31983,1000.);
#8470=VECTOR('',#31984,1000.);
#8471=VECTOR('',#31987,1000.);
#8472=VECTOR('',#31990,1000.);
#8473=VECTOR('',#31993,1000.);
#8474=VECTOR('',#31998,1000.);
#8475=VECTOR('',#31999,1000.);
#8476=VECTOR('',#32004,1000.);
#8477=VECTOR('',#32005,1000.);
#8478=VECTOR('',#32012,1000.);
#8479=VECTOR('',#32015,1000.);
#8480=VECTOR('',#32018,1000.);
#8481=VECTOR('',#32021,1000.);
#8482=VECTOR('',#32024,1000.);
#8483=VECTOR('',#32025,1000.);
#8484=VECTOR('',#32026,1000.);
#8485=VECTOR('',#32029,1000.);
#8486=VECTOR('',#32030,1000.);
#8487=VECTOR('',#32033,1000.);
#8488=VECTOR('',#32034,1000.);
#8489=VECTOR('',#32037,1000.);
#8490=VECTOR('',#32040,1000.);
#8491=VECTOR('',#32041,1000.);
#8492=VECTOR('',#32044,1000.);
#8493=VECTOR('',#32047,1000.);
#8494=VECTOR('',#32050,1000.);
#8495=VECTOR('',#32053,1000.);
#8496=VECTOR('',#32056,1000.);
#8497=VECTOR('',#32059,1000.);
#8498=VECTOR('',#32062,1000.);
#8499=VECTOR('',#32063,1000.);
#8500=VECTOR('',#32066,1000.);
#8501=VECTOR('',#32071,1000.);
#8502=VECTOR('',#32072,1000.);
#8503=VECTOR('',#32077,1000.);
#8504=VECTOR('',#32080,1000.);
#8505=VECTOR('',#32107,2.5);
#8506=VECTOR('',#32126,3.);
#8507=VECTOR('',#32137,4.);
#8508=VECTOR('',#32180,1000.);
#8509=VECTOR('',#32181,1000.);
#8510=VECTOR('',#32184,1000.);
#8511=VECTOR('',#32185,1000.);
#8512=VECTOR('',#32188,1000.);
#8513=VECTOR('',#32189,1000.);
#8514=VECTOR('',#32192,1000.);
#8515=VECTOR('',#32193,1000.);
#8516=VECTOR('',#32196,1000.);
#8517=VECTOR('',#32197,1000.);
#8518=VECTOR('',#32200,1000.);
#8519=VECTOR('',#32201,1000.);
#8520=VECTOR('',#32204,1000.);
#8521=VECTOR('',#32205,1000.);
#8522=VECTOR('',#32206,1000.);
#8523=VECTOR('',#32209,1000.);
#8524=VECTOR('',#32210,1000.);
#8525=VECTOR('',#32213,1000.);
#8526=VECTOR('',#32214,1000.);
#8527=VECTOR('',#32217,1000.);
#8528=VECTOR('',#32218,1000.);
#8529=VECTOR('',#32221,1000.);
#8530=VECTOR('',#32222,1000.);
#8531=VECTOR('',#32225,1000.);
#8532=VECTOR('',#32250,1000.);
#8533=VECTOR('',#32251,1000.);
#8534=VECTOR('',#32254,1000.);
#8535=VECTOR('',#32257,1000.);
#8536=VECTOR('',#32260,1000.);
#8537=VECTOR('',#32263,1000.);
#8538=VECTOR('',#32296,6.00000000000003);
#8539=VECTOR('',#32299,1000.);
#8540=VECTOR('',#32300,1000.);
#8541=VECTOR('',#32313,7.00000000000019);
#8542=VECTOR('',#32320,7.5000000000001);
#8543=VECTOR('',#32331,9.00000000000005);
#8544=VECTOR('',#32340,9.99999999999998);
#8545=VECTOR('',#32343,9.9999999999999);
#8546=VECTOR('',#32358,7.5);
#8547=VECTOR('',#32363,7.15);
#8548=VECTOR('',#32372,7.5);
#8549=VECTOR('',#32377,7.5);
#8550=VECTOR('',#32396,1000.);
#8551=VECTOR('',#32397,1000.);
#8552=VECTOR('',#32398,1000.);
#8553=VECTOR('',#32403,1000.);
#8554=VECTOR('',#32404,1000.);
#8555=VECTOR('',#32407,1000.);
#8556=VECTOR('',#32408,1000.);
#8557=VECTOR('',#32419,2.45849999999999);
#8558=VECTOR('',#32424,3.3);
#8559=VECTOR('',#32431,3.3);
#8560=VECTOR('',#32438,3.3);
#8561=VECTOR('',#32445,3.3);
#8562=VECTOR('',#32452,3.3);
#8563=VECTOR('',#32459,3.3);
#8564=VECTOR('',#32466,18.);
#8565=VECTOR('',#32473,13.);
#8566=VECTOR('',#32480,12.75);
#8567=VECTOR('',#32487,10.);
#8568=VECTOR('',#32494,12.75);
#8569=VECTOR('',#32501,13.);
#8570=VECTOR('',#32512,1000.);
#8571=VECTOR('',#32515,1000.);
#8572=VECTOR('',#32528,1000.);
#8573=VECTOR('',#32531,1000.);
#8574=VECTOR('',#32534,1000.);
#8575=VECTOR('',#32535,1000.);
#8576=VECTOR('',#32548,1000.);
#8577=VECTOR('',#32549,1000.);
#8578=VECTOR('',#32576,16.);
#8579=VECTOR('',#32583,7.5);
#8580=VECTOR('',#32590,16.);
#8581=VECTOR('',#32597,5.5);
#8582=VECTOR('',#32604,3.3);
#8583=VECTOR('',#32611,5.5);
#8584=VECTOR('',#32618,3.3);
#8585=VECTOR('',#32623,1000.);
#8586=VECTOR('',#32624,1000.);
#8587=VECTOR('',#32625,1000.);
#8588=VECTOR('',#32626,1000.);
#8589=VECTOR('',#32629,1000.);
#8590=VECTOR('',#32630,1000.);
#8591=VECTOR('',#32631,1000.);
#8592=VECTOR('',#32634,1000.);
#8593=VECTOR('',#32635,1000.);
#8594=VECTOR('',#32636,1000.);
#8595=VECTOR('',#32639,1000.);
#8596=VECTOR('',#32640,1000.);
#8597=VECTOR('',#32641,1000.);
#8598=VECTOR('',#32644,1000.);
#8599=VECTOR('',#32645,1000.);
#8600=VECTOR('',#32646,1000.);
#8601=VECTOR('',#32649,1000.);
#8602=VECTOR('',#32650,1000.);
#8603=VECTOR('',#32651,1000.);
#8604=VECTOR('',#32654,1000.);
#8605=VECTOR('',#32655,1000.);
#8606=VECTOR('',#32656,1000.);
#8607=VECTOR('',#32659,1000.);
#8608=VECTOR('',#32660,1000.);
#8609=VECTOR('',#32661,1000.);
#8610=VECTOR('',#32664,1000.);
#8611=VECTOR('',#32665,1000.);
#8612=VECTOR('',#32666,1000.);
#8613=VECTOR('',#32669,1000.);
#8614=VECTOR('',#32670,1000.);
#8615=VECTOR('',#32671,1000.);
#8616=VECTOR('',#32674,1000.);
#8617=VECTOR('',#32675,1000.);
#8618=VECTOR('',#32676,1000.);
#8619=VECTOR('',#32679,1000.);
#8620=VECTOR('',#32680,1000.);
#8621=VECTOR('',#32699,0.85);
#8622=VECTOR('',#32706,0.85);
#8623=VECTOR('',#32713,1000.);
#8624=VECTOR('',#32716,1000.);
#8625=VECTOR('',#32721,1000.);
#8626=VECTOR('',#32724,1000.);
#8627=VECTOR('',#32727,1000.);
#8628=VECTOR('',#32730,1000.);
#8629=VECTOR('',#32735,1000.);
#8630=VECTOR('',#32738,1000.);
#8631=VECTOR('',#32739,1000.);
#8632=VECTOR('',#32740,1000.);
#8633=VECTOR('',#32743,1000.);
#8634=VECTOR('',#32744,1000.);
#8635=VECTOR('',#32745,1000.);
#8636=VECTOR('',#32746,1000.);
#8637=VECTOR('',#32749,1000.);
#8638=VECTOR('',#32754,1000.);
#8639=VECTOR('',#32759,1000.);
#8640=VECTOR('',#32760,1000.);
#8641=VECTOR('',#32763,1000.);
#8642=VECTOR('',#32766,1000.);
#8643=VECTOR('',#32771,1000.);
#8644=VECTOR('',#32774,1000.);
#8645=VECTOR('',#32777,1000.);
#8646=VECTOR('',#32780,1000.);
#8647=VECTOR('',#32797,14.);
#8648=VECTOR('',#32804,9.75);
#8649=VECTOR('',#32811,7.5);
#8650=VECTOR('',#32818,9.75);
#8651=VECTOR('',#32825,14.);
#8652=VECTOR('',#32832,3.1);
#8653=VECTOR('',#32839,3.1);
#8654=VECTOR('',#32846,3.1);
#8655=VECTOR('',#32853,3.1);
#8656=VECTOR('',#32860,3.50000000000001);
#8657=VECTOR('',#32867,3.5);
#8658=VECTOR('',#32874,3.50000000000001);
#8659=VECTOR('',#32881,3.50000000000001);
#8660=VECTOR('',#32888,5.5);
#8661=VECTOR('',#32895,3.3);
#8662=VECTOR('',#32902,5.5);
#8663=VECTOR('',#32909,3.3);
#8664=VECTOR('',#32916,5.5);
#8665=VECTOR('',#32923,3.3);
#8666=VECTOR('',#32930,5.5);
#8667=VECTOR('',#32937,3.3);
#8668=VECTOR('',#32950,1000.);
#8669=VECTOR('',#32951,1000.);
#8670=VECTOR('',#32952,1000.);
#8671=VECTOR('',#32953,1000.);
#8672=VECTOR('',#32954,1000.);
#8673=VECTOR('',#32955,1000.);
#8674=VECTOR('',#32956,1000.);
#8675=VECTOR('',#32957,1000.);
#8676=VECTOR('',#32958,1000.);
#8677=VECTOR('',#32959,1000.);
#8678=VECTOR('',#32960,1000.);
#8679=VECTOR('',#32961,1000.);
#8680=VECTOR('',#32962,1000.);
#8681=VECTOR('',#32963,1000.);
#8682=VECTOR('',#32964,1000.);
#8683=VECTOR('',#32965,1000.);
#8684=VECTOR('',#32966,1000.);
#8685=VECTOR('',#32967,1000.);
#8686=VECTOR('',#32968,1000.);
#8687=VECTOR('',#32969,1000.);
#8688=VECTOR('',#32972,1000.);
#8689=VECTOR('',#32973,1000.);
#8690=VECTOR('',#32974,1000.);
#8691=VECTOR('',#32977,1000.);
#8692=VECTOR('',#32978,1000.);
#8693=VECTOR('',#32981,1000.);
#8694=VECTOR('',#32982,1000.);
#8695=VECTOR('',#32985,1000.);
#8696=VECTOR('',#32986,1000.);
#8697=VECTOR('',#32989,1000.);
#8698=VECTOR('',#32990,1000.);
#8699=VECTOR('',#32993,1000.);
#8700=VECTOR('',#32994,1000.);
#8701=VECTOR('',#32997,1000.);
#8702=VECTOR('',#32998,1000.);
#8703=VECTOR('',#33001,1000.);
#8704=VECTOR('',#33002,1000.);
#8705=VECTOR('',#33005,1000.);
#8706=VECTOR('',#33006,1000.);
#8707=VECTOR('',#33009,1000.);
#8708=VECTOR('',#33010,1000.);
#8709=VECTOR('',#33013,1000.);
#8710=VECTOR('',#33014,1000.);
#8711=VECTOR('',#33017,1000.);
#8712=VECTOR('',#33030,1000.);
#8713=VECTOR('',#33031,1000.);
#8714=VECTOR('',#33032,1000.);
#8715=VECTOR('',#33033,1000.);
#8716=VECTOR('',#33034,1000.);
#8717=VECTOR('',#33035,1000.);
#8718=VECTOR('',#33036,1000.);
#8719=VECTOR('',#33037,1000.);
#8720=VECTOR('',#33040,1000.);
#8721=VECTOR('',#33041,1000.);
#8722=VECTOR('',#33044,1000.);
#8723=VECTOR('',#33047,1000.);
#8724=VECTOR('',#33050,1000.);
#8725=VECTOR('',#33053,1000.);
#8726=VECTOR('',#33056,1000.);
#8727=VECTOR('',#33059,1000.);
#8728=VECTOR('',#33064,1000.);
#8729=VECTOR('',#33065,1000.);
#8730=VECTOR('',#33066,1000.);
#8731=VECTOR('',#33067,1000.);
#8732=VECTOR('',#33068,1000.);
#8733=VECTOR('',#33069,1000.);
#8734=VECTOR('',#33072,1000.);
#8735=VECTOR('',#33073,1000.);
#8736=VECTOR('',#33074,1000.);
#8737=VECTOR('',#33075,1000.);
#8738=VECTOR('',#33076,1000.);
#8739=VECTOR('',#33077,1000.);
#8740=VECTOR('',#33080,1000.);
#8741=VECTOR('',#33081,1000.);
#8742=VECTOR('',#33082,1000.);
#8743=VECTOR('',#33083,1000.);
#8744=VECTOR('',#33084,1000.);
#8745=VECTOR('',#33085,1000.);
#8746=VECTOR('',#33088,1000.);
#8747=VECTOR('',#33089,1000.);
#8748=VECTOR('',#33090,1000.);
#8749=VECTOR('',#33091,1000.);
#8750=VECTOR('',#33092,1000.);
#8751=VECTOR('',#33093,1000.);
#8752=VECTOR('',#33096,1000.);
#8753=VECTOR('',#33097,1000.);
#8754=VECTOR('',#33098,1000.);
#8755=VECTOR('',#33101,1000.);
#8756=VECTOR('',#33102,1000.);
#8757=VECTOR('',#33105,1000.);
#8758=VECTOR('',#33106,1000.);
#8759=VECTOR('',#33109,1000.);
#8760=VECTOR('',#33110,1000.);
#8761=VECTOR('',#33113,1000.);
#8762=VECTOR('',#33114,1000.);
#8763=VECTOR('',#33117,1000.);
#8764=VECTOR('',#33122,1000.);
#8765=VECTOR('',#33123,1000.);
#8766=VECTOR('',#33124,1000.);
#8767=VECTOR('',#33127,1000.);
#8768=VECTOR('',#33128,1000.);
#8769=VECTOR('',#33131,1000.);
#8770=VECTOR('',#33132,1000.);
#8771=VECTOR('',#33135,1000.);
#8772=VECTOR('',#33136,1000.);
#8773=VECTOR('',#33139,1000.);
#8774=VECTOR('',#33140,1000.);
#8775=VECTOR('',#33143,1000.);
#8776=VECTOR('',#33148,1000.);
#8777=VECTOR('',#33149,1000.);
#8778=VECTOR('',#33150,1000.);
#8779=VECTOR('',#33153,1000.);
#8780=VECTOR('',#33154,1000.);
#8781=VECTOR('',#33157,1000.);
#8782=VECTOR('',#33158,1000.);
#8783=VECTOR('',#33161,1000.);
#8784=VECTOR('',#33162,1000.);
#8785=VECTOR('',#33165,1000.);
#8786=VECTOR('',#33166,1000.);
#8787=VECTOR('',#33169,1000.);
#8788=VECTOR('',#33174,1000.);
#8789=VECTOR('',#33175,1000.);
#8790=VECTOR('',#33176,1000.);
#8791=VECTOR('',#33179,1000.);
#8792=VECTOR('',#33180,1000.);
#8793=VECTOR('',#33183,1000.);
#8794=VECTOR('',#33184,1000.);
#8795=VECTOR('',#33187,1000.);
#8796=VECTOR('',#33188,1000.);
#8797=VECTOR('',#33191,1000.);
#8798=VECTOR('',#33192,1000.);
#8799=VECTOR('',#33195,1000.);
#8800=VECTOR('',#33210,1.);
#8801=VECTOR('',#33225,2.);
#8802=VECTOR('',#33230,2.);
#8803=VECTOR('',#33235,1.25);
#8804=VECTOR('',#33242,2.);
#8805=VECTOR('',#33247,6.9585);
#8806=VECTOR('',#33256,7.5);
#8807=VECTOR('',#33263,1000.);
#8808=VECTOR('',#33266,1000.);
#8809=VECTOR('',#33271,10.5);
#8810=VECTOR('',#33276,6.9585);
#8811=VECTOR('',#33295,1000.);
#8812=VECTOR('',#33298,1000.);
#8813=VECTOR('',#33303,1000.);
#8814=VECTOR('',#33306,1000.);
#8815=VECTOR('',#33311,1000.);
#8816=VECTOR('',#33314,1000.);
#8817=VECTOR('',#33319,1000.);
#8818=VECTOR('',#33320,1000.);
#8819=VECTOR('',#33321,1000.);
#8820=VECTOR('',#33322,1000.);
#8821=VECTOR('',#33325,1000.);
#8822=VECTOR('',#33326,1000.);
#8823=VECTOR('',#33327,1000.);
#8824=VECTOR('',#33328,1000.);
#8825=VECTOR('',#33341,1000.);
#8826=VECTOR('',#33342,1000.);
#8827=VECTOR('',#33343,1000.);
#8828=VECTOR('',#33344,1000.);
#8829=VECTOR('',#33347,1000.);
#8830=VECTOR('',#33348,1000.);
#8831=VECTOR('',#33349,1000.);
#8832=VECTOR('',#33352,1000.);
#8833=VECTOR('',#33353,1000.);
#8834=VECTOR('',#33354,1000.);
#8835=VECTOR('',#33357,1000.);
#8836=VECTOR('',#33358,1000.);
#8837=VECTOR('',#33359,1000.);
#8838=VECTOR('',#33362,1000.);
#8839=VECTOR('',#33363,1000.);
#8840=VECTOR('',#33364,1000.);
#8841=VECTOR('',#33367,1000.);
#8842=VECTOR('',#33368,1000.);
#8843=VECTOR('',#33387,9.75);
#8844=VECTOR('',#33394,7.5);
#8845=VECTOR('',#33415,3.);
#8846=VECTOR('',#33422,3.);
#8847=VECTOR('',#33429,3.25);
#8848=VECTOR('',#33436,3.25);
#8849=VECTOR('',#33443,3.25);
#8850=VECTOR('',#33450,3.25);
#8851=VECTOR('',#33455,1000.);
#8852=VECTOR('',#33456,1000.);
#8853=VECTOR('',#33457,1000.);
#8854=VECTOR('',#33458,1000.);
#8855=VECTOR('',#33461,1000.);
#8856=VECTOR('',#33462,1000.);
#8857=VECTOR('',#33463,1000.);
#8858=VECTOR('',#33464,1000.);
#8859=VECTOR('',#33465,1000.);
#8860=VECTOR('',#33468,1000.);
#8861=VECTOR('',#33469,1000.);
#8862=VECTOR('',#33470,1000.);
#8863=VECTOR('',#33471,1000.);
#8864=VECTOR('',#33474,1000.);
#8865=VECTOR('',#33475,1000.);
#8866=VECTOR('',#33476,1000.);
#8867=VECTOR('',#33477,1000.);
#8868=VECTOR('',#33478,1000.);
#8869=VECTOR('',#33481,1000.);
#8870=VECTOR('',#33482,1000.);
#8871=VECTOR('',#33483,1000.);
#8872=VECTOR('',#33484,1000.);
#8873=VECTOR('',#33487,1000.);
#8874=VECTOR('',#33488,1000.);
#8875=VECTOR('',#33493,1000.);
#8876=VECTOR('',#33494,1000.);
#8877=VECTOR('',#33497,1000.);
#8878=VECTOR('',#33500,1000.);
#8879=VECTOR('',#33501,1000.);
#8880=VECTOR('',#33504,1000.);
#8881=VECTOR('',#33519,2.);
#8882=VECTOR('',#33530,2.);
#8883=VECTOR('',#33923,2.);
#8884=VECTOR('',#33932,2.);
#8885=VECTOR('',#33941,2.);
#8886=VECTOR('',#33950,13.5);
#8887=VECTOR('',#33957,2.);
#8888=VECTOR('',#33966,2.);
#8889=VECTOR('',#33975,2.);
#8890=VECTOR('',#33986,1000.);
#8891=VECTOR('',#33987,1000.);
#8892=VECTOR('',#33988,1000.);
#8893=VECTOR('',#33989,1000.);
#8894=VECTOR('',#33990,1000.);
#8895=VECTOR('',#33991,1000.);
#8896=VECTOR('',#33998,2.5);
#8897=VECTOR('',#34001,1000.);
#8898=VECTOR('',#34002,1000.);
#8899=VECTOR('',#34003,1000.);
#8900=VECTOR('',#34004,1000.);
#8901=VECTOR('',#34005,1000.);
#8902=VECTOR('',#34006,1000.);
#8903=VECTOR('',#34009,1000.);
#8904=VECTOR('',#34010,1000.);
#8905=VECTOR('',#34013,1000.);
#8906=VECTOR('',#34016,1000.);
#8907=VECTOR('',#34019,1000.);
#8908=VECTOR('',#34022,1000.);
#8909=VECTOR('',#34035,5.);
#8910=VECTOR('',#34046,1000.);
#8911=VECTOR('',#34047,1000.);
#8912=VECTOR('',#34048,1000.);
#8913=VECTOR('',#34049,1000.);
#8914=VECTOR('',#34050,1000.);
#8915=VECTOR('',#34051,1000.);
#8916=VECTOR('',#34054,1000.);
#8917=VECTOR('',#34055,1000.);
#8918=VECTOR('',#34056,1000.);
#8919=VECTOR('',#34057,1000.);
#8920=VECTOR('',#34058,1000.);
#8921=VECTOR('',#34059,1000.);
#8922=VECTOR('',#34062,1000.);
#8923=VECTOR('',#34063,1000.);
#8924=VECTOR('',#34066,1000.);
#8925=VECTOR('',#34069,1000.);
#8926=VECTOR('',#34072,1000.);
#8927=VECTOR('',#34075,1000.);
#8928=VECTOR('',#34086,2.693275);
#8929=VECTOR('',#34089,3.);
#8930=VECTOR('',#34100,5.);
#8931=VECTOR('',#34111,1000.);
#8932=VECTOR('',#34112,1000.);
#8933=VECTOR('',#34113,1000.);
#8934=VECTOR('',#34114,1000.);
#8935=VECTOR('',#34115,1000.);
#8936=VECTOR('',#34116,1000.);
#8937=VECTOR('',#34119,1000.);
#8938=VECTOR('',#34120,1000.);
#8939=VECTOR('',#34121,1000.);
#8940=VECTOR('',#34122,1000.);
#8941=VECTOR('',#34123,1000.);
#8942=VECTOR('',#34124,1000.);
#8943=VECTOR('',#34127,1000.);
#8944=VECTOR('',#34128,1000.);
#8945=VECTOR('',#34131,1000.);
#8946=VECTOR('',#34134,1000.);
#8947=VECTOR('',#34137,1000.);
#8948=VECTOR('',#34140,1000.);
#8949=VECTOR('',#34151,2.693275);
#8950=VECTOR('',#34154,3.);
#8951=VECTOR('',#34159,1000.);
#8952=VECTOR('',#34162,1000.);
#8953=VECTOR('',#34169,1000.);
#8954=VECTOR('',#34170,1000.);
#8955=VECTOR('',#34195,1000.);
#8956=VECTOR('',#34196,1000.);
#8957=VECTOR('',#34199,1000.);
#8958=VECTOR('',#34200,1000.);
#8959=VECTOR('',#34205,1000.);
#8960=VECTOR('',#34210,1000.);
#8961=VECTOR('',#34217,1000.);
#8962=VECTOR('',#34222,1000.);
#8963=VECTOR('',#34229,1000.);
#8964=VECTOR('',#34230,1000.);
#8965=VECTOR('',#34233,1000.);
#8966=VECTOR('',#34236,1000.);
#8967=VECTOR('',#34239,1000.);
#8968=VECTOR('',#34242,1000.);
#8969=VECTOR('',#34243,1000.);
#8970=VECTOR('',#34246,2.5);
#8971=VECTOR('',#34259,3.3);
#8972=VECTOR('',#34268,2.5);
#8973=VECTOR('',#34281,1000.);
#8974=VECTOR('',#34282,1000.);
#8975=VECTOR('',#34283,1000.);
#8976=VECTOR('',#34284,1000.);
#8977=VECTOR('',#34285,1000.);
#8978=VECTOR('',#34290,2.5);
#8979=VECTOR('',#34295,2.5);
#8980=VECTOR('',#34304,3.3);
#8981=VECTOR('',#34309,1000.);
#8982=VECTOR('',#34312,1000.);
#8983=VECTOR('',#34313,1000.);
#8984=VECTOR('',#34314,1000.);
#8985=VECTOR('',#34315,1000.);
#8986=VECTOR('',#34316,1000.);
#8987=VECTOR('',#34321,1000.);
#8988=VECTOR('',#34322,1000.);
#8989=VECTOR('',#34323,1000.);
#8990=VECTOR('',#34354,1000.);
#8991=VECTOR('',#34355,1000.);
#8992=VECTOR('',#34356,1000.);
#8993=VECTOR('',#34361,1000.);
#8994=VECTOR('',#34362,1000.);
#8995=VECTOR('',#34365,1000.);
#8996=VECTOR('',#34366,1000.);
#8997=VECTOR('',#34369,1000.);
#8998=VECTOR('',#34370,1000.);
#8999=VECTOR('',#34377,2.1);
#9000=VECTOR('',#34380,1000.);
#9001=VECTOR('',#34381,1000.);
#9002=VECTOR('',#34384,1000.);
#9003=VECTOR('',#34385,1000.);
#9004=VECTOR('',#34388,1000.);
#9005=VECTOR('',#34391,1000.);
#9006=VECTOR('',#34394,1000.);
#9007=VECTOR('',#34397,1000.);
#9008=VECTOR('',#34406,1000.);
#9009=VECTOR('',#34407,1000.);
#9010=VECTOR('',#34412,1000.);
#9011=VECTOR('',#34413,1000.);
#9012=VECTOR('',#34416,1000.);
#9013=VECTOR('',#34419,1000.);
#9014=VECTOR('',#34424,1000.);
#9015=VECTOR('',#34431,1000.);
#9016=VECTOR('',#34446,1000.);
#9017=VECTOR('',#34449,1000.);
#9018=VECTOR('',#34452,1000.);
#9019=VECTOR('',#34455,1000.);
#9020=VECTOR('',#34458,1000.);
#9021=VECTOR('',#34461,1000.);
#9022=VECTOR('',#34464,1000.);
#9023=VECTOR('',#34467,1000.);
#9024=VECTOR('',#34468,1000.);
#9025=VECTOR('',#34473,1000.);
#9026=VECTOR('',#34480,1000.);
#9027=VECTOR('',#34485,1000.);
#9028=VECTOR('',#34488,1000.);
#9029=VECTOR('',#34493,1000.);
#9030=VECTOR('',#34498,1000.);
#9031=VECTOR('',#34503,1000.);
#9032=VECTOR('',#34510,1000.);
#9033=VECTOR('',#34513,1000.);
#9034=VECTOR('',#34516,1000.);
#9035=VECTOR('',#34519,1000.);
#9036=VECTOR('',#34522,1000.);
#9037=VECTOR('',#34523,1000.);
#9038=VECTOR('',#34526,1000.);
#9039=VECTOR('',#34529,1000.);
#9040=VECTOR('',#34532,1000.);
#9041=VECTOR('',#34535,1000.);
#9042=VECTOR('',#34538,1000.);
#9043=VECTOR('',#34541,1000.);
#9044=VECTOR('',#34546,1000.);
#9045=VECTOR('',#34549,1000.);
#9046=VECTOR('',#34552,1000.);
#9047=VECTOR('',#34553,1000.);
#9048=VECTOR('',#34556,1000.);
#9049=VECTOR('',#34561,1000.);
#9050=VECTOR('',#34562,1000.);
#9051=VECTOR('',#34563,1000.);
#9052=VECTOR('',#34566,1000.);
#9053=VECTOR('',#34571,1000.);
#9054=VECTOR('',#34576,1000.);
#9055=VECTOR('',#34577,1000.);
#9056=VECTOR('',#34580,1000.);
#9057=VECTOR('',#34585,1000.);
#9058=VECTOR('',#34586,1000.);
#9059=VECTOR('',#34601,1000.);
#9060=VECTOR('',#34606,1000.);
#9061=VECTOR('',#34611,1000.);
#9062=VECTOR('',#34612,1000.);
#9063=VECTOR('',#34615,1000.);
#9064=VECTOR('',#34618,1000.);
#9065=VECTOR('',#34621,1000.);
#9066=VECTOR('',#34624,1000.);
#9067=VECTOR('',#34629,1000.);
#9068=VECTOR('',#34630,1000.);
#9069=VECTOR('',#34631,1000.);
#9070=VECTOR('',#34634,1000.);
#9071=VECTOR('',#34639,1000.);
#9072=VECTOR('',#34644,1000.);
#9073=VECTOR('',#34645,1000.);
#9074=VECTOR('',#34650,1000.);
#9075=VECTOR('',#34659,1000.);
#9076=VECTOR('',#34662,1000.);
#9077=VECTOR('',#34665,1000.);
#9078=VECTOR('',#34666,1000.);
#9079=VECTOR('',#34669,1000.);
#9080=VECTOR('',#34674,1000.);
#9081=VECTOR('',#34677,1000.);
#9082=VECTOR('',#34678,1000.);
#9083=VECTOR('',#34681,1000.);
#9084=VECTOR('',#34684,1000.);
#9085=VECTOR('',#34687,1000.);
#9086=VECTOR('',#34688,1000.);
#9087=VECTOR('',#34691,1000.);
#9088=VECTOR('',#34696,1000.);
#9089=VECTOR('',#34697,1000.);
#9090=VECTOR('',#34700,1000.);
#9091=VECTOR('',#34705,1000.);
#9092=VECTOR('',#34708,1000.);
#9093=VECTOR('',#34711,1000.);
#9094=VECTOR('',#34720,1000.);
#9095=VECTOR('',#34721,1000.);
#9096=VECTOR('',#34722,1000.);
#9097=VECTOR('',#34723,1000.);
#9098=VECTOR('',#34724,1000.);
#9099=VECTOR('',#34725,1000.);
#9100=VECTOR('',#34732,2.5);
#9101=VECTOR('',#34735,1000.);
#9102=VECTOR('',#34736,1000.);
#9103=VECTOR('',#34737,1000.);
#9104=VECTOR('',#34738,1000.);
#9105=VECTOR('',#34739,1000.);
#9106=VECTOR('',#34740,1000.);
#9107=VECTOR('',#34743,1000.);
#9108=VECTOR('',#34744,1000.);
#9109=VECTOR('',#34747,1000.);
#9110=VECTOR('',#34750,1000.);
#9111=VECTOR('',#34753,1000.);
#9112=VECTOR('',#34756,1000.);
#9113=VECTOR('',#34769,5.);
#9114=VECTOR('',#34780,1000.);
#9115=VECTOR('',#34781,1000.);
#9116=VECTOR('',#34782,1000.);
#9117=VECTOR('',#34783,1000.);
#9118=VECTOR('',#34784,1000.);
#9119=VECTOR('',#34785,1000.);
#9120=VECTOR('',#34788,1000.);
#9121=VECTOR('',#34789,1000.);
#9122=VECTOR('',#34790,1000.);
#9123=VECTOR('',#34791,1000.);
#9124=VECTOR('',#34792,1000.);
#9125=VECTOR('',#34793,1000.);
#9126=VECTOR('',#34796,1000.);
#9127=VECTOR('',#34797,1000.);
#9128=VECTOR('',#34800,1000.);
#9129=VECTOR('',#34803,1000.);
#9130=VECTOR('',#34806,1000.);
#9131=VECTOR('',#34809,1000.);
#9132=VECTOR('',#34820,2.693275);
#9133=VECTOR('',#34823,3.);
#9134=VECTOR('',#34834,5.);
#9135=VECTOR('',#34845,1000.);
#9136=VECTOR('',#34846,1000.);
#9137=VECTOR('',#34847,1000.);
#9138=VECTOR('',#34848,1000.);
#9139=VECTOR('',#34849,1000.);
#9140=VECTOR('',#34850,1000.);
#9141=VECTOR('',#34853,1000.);
#9142=VECTOR('',#34854,1000.);
#9143=VECTOR('',#34855,1000.);
#9144=VECTOR('',#34856,1000.);
#9145=VECTOR('',#34857,1000.);
#9146=VECTOR('',#34858,1000.);
#9147=VECTOR('',#34861,1000.);
#9148=VECTOR('',#34862,1000.);
#9149=VECTOR('',#34865,1000.);
#9150=VECTOR('',#34868,1000.);
#9151=VECTOR('',#34871,1000.);
#9152=VECTOR('',#34874,1000.);
#9153=VECTOR('',#34885,2.693275);
#9154=VECTOR('',#34888,3.);
#9155=VECTOR('',#34893,1000.);
#9156=VECTOR('',#34896,1000.);
#9157=VECTOR('',#34903,1000.);
#9158=VECTOR('',#34904,1000.);
#9159=VECTOR('',#34929,1000.);
#9160=VECTOR('',#34930,1000.);
#9161=VECTOR('',#34933,1000.);
#9162=VECTOR('',#34934,1000.);
#9163=VECTOR('',#34939,1000.);
#9164=VECTOR('',#34944,1000.);
#9165=VECTOR('',#34951,1000.);
#9166=VECTOR('',#34956,1000.);
#9167=VECTOR('',#34963,1000.);
#9168=VECTOR('',#34964,1000.);
#9169=VECTOR('',#34967,1000.);
#9170=VECTOR('',#34970,1000.);
#9171=VECTOR('',#34973,1000.);
#9172=VECTOR('',#34976,1000.);
#9173=VECTOR('',#34977,1000.);
#9174=VECTOR('',#34980,2.5);
#9175=VECTOR('',#34993,3.3);
#9176=VECTOR('',#35002,2.5);
#9177=VECTOR('',#35015,1000.);
#9178=VECTOR('',#35016,1000.);
#9179=VECTOR('',#35017,1000.);
#9180=VECTOR('',#35018,1000.);
#9181=VECTOR('',#35019,1000.);
#9182=VECTOR('',#35024,2.5);
#9183=VECTOR('',#35029,2.5);
#9184=VECTOR('',#35038,3.3);
#9185=VECTOR('',#35043,1000.);
#9186=VECTOR('',#35046,1000.);
#9187=VECTOR('',#35047,1000.);
#9188=VECTOR('',#35048,1000.);
#9189=VECTOR('',#35049,1000.);
#9190=VECTOR('',#35050,1000.);
#9191=VECTOR('',#35055,1000.);
#9192=VECTOR('',#35056,1000.);
#9193=VECTOR('',#35057,1000.);
#9194=VECTOR('',#35088,1000.);
#9195=VECTOR('',#35089,1000.);
#9196=VECTOR('',#35090,1000.);
#9197=VECTOR('',#35095,1000.);
#9198=VECTOR('',#35098,1000.);
#9199=VECTOR('',#35101,1000.);
#9200=VECTOR('',#35102,1000.);
#9201=VECTOR('',#35109,2.1);
#9202=VECTOR('',#35112,1000.);
#9203=VECTOR('',#35115,1000.);
#9204=VECTOR('',#35122,1000.);
#9205=VECTOR('',#35123,1000.);
#9206=VECTOR('',#35128,1000.);
#9207=VECTOR('',#35129,1000.);
#9208=VECTOR('',#35132,1000.);
#9209=VECTOR('',#35135,1000.);
#9210=VECTOR('',#35140,1000.);
#9211=VECTOR('',#35147,1000.);
#9212=VECTOR('',#35162,1000.);
#9213=VECTOR('',#35165,1000.);
#9214=VECTOR('',#35168,1000.);
#9215=VECTOR('',#35171,1000.);
#9216=VECTOR('',#35174,1000.);
#9217=VECTOR('',#35177,1000.);
#9218=VECTOR('',#35180,1000.);
#9219=VECTOR('',#35183,1000.);
#9220=VECTOR('',#35184,1000.);
#9221=VECTOR('',#35189,1000.);
#9222=VECTOR('',#35196,1000.);
#9223=VECTOR('',#35201,1000.);
#9224=VECTOR('',#35204,1000.);
#9225=VECTOR('',#35209,1000.);
#9226=VECTOR('',#35214,1000.);
#9227=VECTOR('',#35219,1000.);
#9228=VECTOR('',#35226,1000.);
#9229=VECTOR('',#35229,1000.);
#9230=VECTOR('',#35232,1000.);
#9231=VECTOR('',#35235,1000.);
#9232=VECTOR('',#35238,1000.);
#9233=VECTOR('',#35239,1000.);
#9234=VECTOR('',#35242,1000.);
#9235=VECTOR('',#35245,1000.);
#9236=VECTOR('',#35248,1000.);
#9237=VECTOR('',#35251,1000.);
#9238=VECTOR('',#35254,1000.);
#9239=VECTOR('',#35257,1000.);
#9240=VECTOR('',#35262,1000.);
#9241=VECTOR('',#35265,1000.);
#9242=VECTOR('',#35268,1000.);
#9243=VECTOR('',#35269,1000.);
#9244=VECTOR('',#35272,1000.);
#9245=VECTOR('',#35277,1000.);
#9246=VECTOR('',#35278,1000.);
#9247=VECTOR('',#35279,1000.);
#9248=VECTOR('',#35282,1000.);
#9249=VECTOR('',#35287,1000.);
#9250=VECTOR('',#35292,1000.);
#9251=VECTOR('',#35293,1000.);
#9252=VECTOR('',#35296,1000.);
#9253=VECTOR('',#35301,1000.);
#9254=VECTOR('',#35302,1000.);
#9255=VECTOR('',#35317,1000.);
#9256=VECTOR('',#35322,1000.);
#9257=VECTOR('',#35327,1000.);
#9258=VECTOR('',#35328,1000.);
#9259=VECTOR('',#35331,1000.);
#9260=VECTOR('',#35334,1000.);
#9261=VECTOR('',#35337,1000.);
#9262=VECTOR('',#35340,1000.);
#9263=VECTOR('',#35345,1000.);
#9264=VECTOR('',#35346,1000.);
#9265=VECTOR('',#35347,1000.);
#9266=VECTOR('',#35350,1000.);
#9267=VECTOR('',#35355,1000.);
#9268=VECTOR('',#35360,1000.);
#9269=VECTOR('',#35361,1000.);
#9270=VECTOR('',#35366,1000.);
#9271=VECTOR('',#35375,1000.);
#9272=VECTOR('',#35378,1000.);
#9273=VECTOR('',#35381,1000.);
#9274=VECTOR('',#35382,1000.);
#9275=VECTOR('',#35385,1000.);
#9276=VECTOR('',#35390,1000.);
#9277=VECTOR('',#35393,1000.);
#9278=VECTOR('',#35394,1000.);
#9279=VECTOR('',#35397,1000.);
#9280=VECTOR('',#35400,1000.);
#9281=VECTOR('',#35403,1000.);
#9282=VECTOR('',#35404,1000.);
#9283=VECTOR('',#35407,1000.);
#9284=VECTOR('',#35412,1000.);
#9285=VECTOR('',#35413,1000.);
#9286=VECTOR('',#35416,1000.);
#9287=VECTOR('',#35421,1000.);
#9288=VECTOR('',#35424,1000.);
#9289=VECTOR('',#35427,1000.);
#9290=VECTOR('',#35456,2.5);
#9291=VECTOR('',#35461,2.5);
#9292=VECTOR('',#35466,2.5);
#9293=VECTOR('',#35471,2.5);
#9294=VECTOR('',#35476,2.5);
#9295=VECTOR('',#35481,2.5);
#9296=VECTOR('',#35486,2.5);
#9297=VECTOR('',#35491,2.5);
#9298=VECTOR('',#35496,2.5);
#9299=VECTOR('',#35501,2.5);
#9300=VECTOR('',#35506,2.5);
#9301=VECTOR('',#35511,2.5);
#9302=VECTOR('',#35516,2.5);
#9303=VECTOR('',#35521,2.5);
#9304=VECTOR('',#35526,2.5);
#9305=VECTOR('',#35531,2.5);
#9306=VECTOR('',#35536,2.5);
#9307=VECTOR('',#35541,2.5);
#9308=VECTOR('',#35546,2.5);
#9309=VECTOR('',#35551,2.5);
#9310=VECTOR('',#35556,2.5);
#9311=VECTOR('',#35561,2.5);
#9312=VECTOR('',#35566,2.5);
#9313=VECTOR('',#35571,2.5);
#9314=VECTOR('',#35576,2.5);
#9315=VECTOR('',#35581,2.5);
#9316=VECTOR('',#35586,2.5);
#9317=VECTOR('',#35591,2.5);
#9318=VECTOR('',#35596,2.5);
#9319=VECTOR('',#35601,2.5);
#9320=VECTOR('',#35606,2.5);
#9321=VECTOR('',#35611,2.5);
#9322=VECTOR('',#35616,2.5);
#9323=VECTOR('',#35621,2.5);
#9324=VECTOR('',#35624,1000.);
#9325=VECTOR('',#35625,1000.);
#9326=VECTOR('',#35626,1000.);
#9327=VECTOR('',#35627,1000.);
#9328=VECTOR('',#35630,1000.);
#9329=VECTOR('',#35633,1000.);
#9330=VECTOR('',#35636,1000.);
#9331=VECTOR('',#35637,1000.);
#9332=VECTOR('',#35638,1000.);
#9333=VECTOR('',#35639,1000.);
#9334=VECTOR('',#35640,1000.);
#9335=VECTOR('',#35643,1000.);
#9336=VECTOR('',#35644,1000.);
#9337=VECTOR('',#35645,1000.);
#9338=VECTOR('',#35648,1000.);
#9339=VECTOR('',#35651,1000.);
#9340=VECTOR('',#35654,1000.);
#9341=VECTOR('',#35655,1000.);
#9342=VECTOR('',#35656,1000.);
#9343=VECTOR('',#35657,1000.);
#9344=VECTOR('',#35660,1000.);
#9345=VECTOR('',#35661,1000.);
#9346=VECTOR('',#35668,1000.);
#9347=VECTOR('',#35671,1000.);
#9348=VECTOR('',#35672,1000.);
#9349=VECTOR('',#35675,1000.);
#9350=VECTOR('',#35686,5.);
#9351=VECTOR('',#35691,5.);
#9352=VECTOR('',#35698,2.4585);
#9353=VECTOR('',#35705,3.);
#9354=VECTOR('',#35712,1000.);
#9355=VECTOR('',#35713,1000.);
#9356=VECTOR('',#35714,1000.);
#9357=VECTOR('',#35715,1000.);
#9358=VECTOR('',#35716,1000.);
#9359=VECTOR('',#35717,1000.);
#9360=VECTOR('',#35722,1000.);
#9361=VECTOR('',#35723,1000.);
#9362=VECTOR('',#35724,1000.);
#9363=VECTOR('',#35727,1000.);
#9364=VECTOR('',#35728,1000.);
#9365=VECTOR('',#35731,1000.);
#9366=VECTOR('',#35732,1000.);
#9367=VECTOR('',#35735,1000.);
#9368=VECTOR('',#35736,1000.);
#9369=VECTOR('',#35739,1000.);
#9370=VECTOR('',#35740,1000.);
#9371=VECTOR('',#35743,1000.);
#9372=VECTOR('',#35754,3.75);
#9373=VECTOR('',#35759,1664.2794823505);
#9374=VECTOR('',#35776,4.25);
#9375=VECTOR('',#35783,2.065);
#9376=VECTOR('',#35790,3.);
#9377=VECTOR('',#35795,1000.);
#9378=VECTOR('',#35796,1000.);
#9379=VECTOR('',#35797,1000.);
#9380=VECTOR('',#35798,1000.);
#9381=VECTOR('',#35799,1000.);
#9382=VECTOR('',#35800,1000.);
#9383=VECTOR('',#35809,1000.);
#9384=VECTOR('',#35810,1000.);
#9385=VECTOR('',#35811,1000.);
#9386=VECTOR('',#35812,1000.);
#9387=VECTOR('',#35815,1000.);
#9388=VECTOR('',#35816,1000.);
#9389=VECTOR('',#35817,1000.);
#9390=VECTOR('',#35820,1000.);
#9391=VECTOR('',#35821,1000.);
#9392=VECTOR('',#35822,1000.);
#9393=VECTOR('',#35825,1000.);
#9394=VECTOR('',#35826,1000.);
#9395=VECTOR('',#35827,1000.);
#9396=VECTOR('',#35830,1000.);
#9397=VECTOR('',#35831,1000.);
#9398=VECTOR('',#35832,1000.);
#9399=VECTOR('',#35835,1000.);
#9400=VECTOR('',#35836,1000.);
#9401=VECTOR('',#35853,5.);
#9402=VECTOR('',#35860,2.5);
#9403=VECTOR('',#35871,1000.);
#9404=VECTOR('',#35874,1000.);
#9405=VECTOR('',#35879,1000.);
#9406=VECTOR('',#35882,1000.);
#9407=VECTOR('',#35885,1000.);
#9408=VECTOR('',#35886,1000.);
#9409=VECTOR('',#35889,1000.);
#9410=VECTOR('',#35890,1000.);
#9411=VECTOR('',#35901,4.);
#9412=VECTOR('',#35908,4.);
#9413=VECTOR('',#35915,3.25);
#9414=VECTOR('',#35922,3.25);
#9415=VECTOR('',#35929,3.25);
#9416=VECTOR('',#35936,3.25);
#9417=VECTOR('',#35943,3.25);
#9418=VECTOR('',#35950,3.25);
#9419=VECTOR('',#35957,3.25);
#9420=VECTOR('',#35964,3.25);
#9421=VECTOR('',#35969,1000.);
#9422=VECTOR('',#35970,1000.);
#9423=VECTOR('',#35971,1000.);
#9424=VECTOR('',#35972,1000.);
#9425=VECTOR('',#35975,1000.);
#9426=VECTOR('',#35976,1000.);
#9427=VECTOR('',#35977,1000.);
#9428=VECTOR('',#35980,1000.);
#9429=VECTOR('',#35981,1000.);
#9430=VECTOR('',#35982,1000.);
#9431=VECTOR('',#35983,1000.);
#9432=VECTOR('',#35986,1000.);
#9433=VECTOR('',#35987,1000.);
#9434=VECTOR('',#35988,1000.);
#9435=VECTOR('',#35991,1000.);
#9436=VECTOR('',#35992,1000.);
#9437=VECTOR('',#35993,1000.);
#9438=VECTOR('',#35998,1000.);
#9439=VECTOR('',#36007,5.);
#9440=VECTOR('',#36012,5.);
#9441=VECTOR('',#36019,2.4585);
#9442=VECTOR('',#36026,3.);
#9443=VECTOR('',#36033,1000.);
#9444=VECTOR('',#36034,1000.);
#9445=VECTOR('',#36035,1000.);
#9446=VECTOR('',#36036,1000.);
#9447=VECTOR('',#36037,1000.);
#9448=VECTOR('',#36038,1000.);
#9449=VECTOR('',#36043,1000.);
#9450=VECTOR('',#36044,1000.);
#9451=VECTOR('',#36045,1000.);
#9452=VECTOR('',#36048,1000.);
#9453=VECTOR('',#36049,1000.);
#9454=VECTOR('',#36052,1000.);
#9455=VECTOR('',#36053,1000.);
#9456=VECTOR('',#36056,1000.);
#9457=VECTOR('',#36057,1000.);
#9458=VECTOR('',#36060,1000.);
#9459=VECTOR('',#36061,1000.);
#9460=VECTOR('',#36064,1000.);
#9461=CIRCLE('',#26044,3.4);
#9462=CIRCLE('',#26045,3.4);
#9463=CIRCLE('',#26047,3.4);
#9464=CIRCLE('',#26048,3.4);
#9465=CIRCLE('',#26050,3.);
#9466=CIRCLE('',#26051,2.99999999999999);
#9467=CIRCLE('',#26053,3.);
#9468=CIRCLE('',#26054,2.99999999999999);
#9469=CIRCLE('',#26072,3.);
#9470=CIRCLE('',#26073,3.);
#9471=CIRCLE('',#26075,3.);
#9472=CIRCLE('',#26076,3.);
#9473=CIRCLE('',#26078,4.25000000000001);
#9474=CIRCLE('',#26079,4.25000000000001);
#9475=CIRCLE('',#26081,4.25000000000001);
#9476=CIRCLE('',#26082,4.25000000000001);
#9477=CIRCLE('',#26097,2.1);
#9478=CIRCLE('',#26098,2.1);
#9479=CIRCLE('',#26100,2.1);
#9480=CIRCLE('',#26101,2.1);
#9481=CIRCLE('',#26103,2.1);
#9482=CIRCLE('',#26104,2.1);
#9483=CIRCLE('',#26106,2.1);
#9484=CIRCLE('',#26107,2.1);
#9485=CIRCLE('',#26109,3.);
#9486=CIRCLE('',#26110,3.);
#9487=CIRCLE('',#26112,3.);
#9488=CIRCLE('',#26113,3.);
#9489=CIRCLE('',#26115,5.5);
#9490=CIRCLE('',#26116,5.5);
#9491=CIRCLE('',#26118,3.3);
#9492=CIRCLE('',#26119,3.3);
#9493=CIRCLE('',#26121,5.5);
#9494=CIRCLE('',#26122,5.5);
#9495=CIRCLE('',#26124,3.3);
#9496=CIRCLE('',#26125,3.3);
#9497=CIRCLE('',#26127,17.5);
#9498=CIRCLE('',#26128,17.5);
#9499=CIRCLE('',#26130,35.);
#9500=CIRCLE('',#26131,35.);
#9501=CIRCLE('',#26144,2.1);
#9502=CIRCLE('',#26145,2.1);
#9503=CIRCLE('',#26147,2.1);
#9504=CIRCLE('',#26148,2.1);
#9505=CIRCLE('',#26150,2.1);
#9506=CIRCLE('',#26151,2.1);
#9507=CIRCLE('',#26153,2.1);
#9508=CIRCLE('',#26154,2.1);
#9509=CIRCLE('',#26156,2.1);
#9510=CIRCLE('',#26157,2.1);
#9511=CIRCLE('',#26159,2.1);
#9512=CIRCLE('',#26160,2.1);
#9513=CIRCLE('',#26162,18.);
#9514=CIRCLE('',#26163,18.);
#9515=CIRCLE('',#26165,10.);
#9516=CIRCLE('',#26166,10.);
#9517=CIRCLE('',#26169,10.);
#9518=CIRCLE('',#26170,10.);
#9519=CIRCLE('',#26178,2.99999999999999);
#9520=CIRCLE('',#26179,2.99999999999999);
#9521=CIRCLE('',#26181,2.99999999999999);
#9522=CIRCLE('',#26182,2.99999999999999);
#9523=CIRCLE('',#26184,3.3);
#9524=CIRCLE('',#26185,3.3);
#9525=CIRCLE('',#26187,3.3);
#9526=CIRCLE('',#26188,3.3);
#9527=CIRCLE('',#26190,3.3);
#9528=CIRCLE('',#26191,3.3);
#9529=CIRCLE('',#26193,3.3);
#9530=CIRCLE('',#26194,3.3);
#9531=CIRCLE('',#26205,3.3);
#9532=CIRCLE('',#26206,3.3);
#9533=CIRCLE('',#26208,3.3);
#9534=CIRCLE('',#26209,3.3);
#9535=CIRCLE('',#26211,3.3);
#9536=CIRCLE('',#26212,3.3);
#9537=CIRCLE('',#26214,3.3);
#9538=CIRCLE('',#26215,3.3);
#9539=CIRCLE('',#26217,3.3);
#9540=CIRCLE('',#26218,3.3);
#9541=CIRCLE('',#26220,3.3);
#9542=CIRCLE('',#26221,3.3);
#9543=CIRCLE('',#26231,5.49999999999995);
#9544=CIRCLE('',#26232,5.49999999999995);
#9545=CIRCLE('',#26234,3.5);
#9546=CIRCLE('',#26236,3.49999999999995);
#9547=CIRCLE('',#26238,3.5);
#9548=CIRCLE('',#26239,3.49999999999995);
#9549=CIRCLE('',#26240,3.5);
#9550=CIRCLE('',#26242,3.49999999999995);
#9551=CIRCLE('',#26245,5.49999999999995);
#9552=CIRCLE('',#26246,5.49999999999995);
#9553=CIRCLE('',#26248,3.5);
#9554=CIRCLE('',#26250,3.49999999999995);
#9555=CIRCLE('',#26252,3.5);
#9556=CIRCLE('',#26253,3.49999999999995);
#9557=CIRCLE('',#26254,3.5);
#9558=CIRCLE('',#26256,3.49999999999995);
#9559=CIRCLE('',#26259,5.49999999999995);
#9560=CIRCLE('',#26260,5.49999999999995);
#9561=CIRCLE('',#26262,3.5);
#9562=CIRCLE('',#26264,3.49999999999995);
#9563=CIRCLE('',#26266,3.5);
#9564=CIRCLE('',#26267,3.49999999999995);
#9565=CIRCLE('',#26268,3.5);
#9566=CIRCLE('',#26270,3.49999999999995);
#9567=CIRCLE('',#26273,5.49999999999995);
#9568=CIRCLE('',#26274,5.49999999999995);
#9569=CIRCLE('',#26276,3.5);
#9570=CIRCLE('',#26278,3.49999999999995);
#9571=CIRCLE('',#26280,3.5);
#9572=CIRCLE('',#26281,3.49999999999995);
#9573=CIRCLE('',#26282,3.5);
#9574=CIRCLE('',#26284,3.49999999999995);
#9575=CIRCLE('',#26287,5.49999999999995);
#9576=CIRCLE('',#26288,5.49999999999995);
#9577=CIRCLE('',#26290,3.5);
#9578=CIRCLE('',#26292,3.49999999999995);
#9579=CIRCLE('',#26294,3.5);
#9580=CIRCLE('',#26295,3.49999999999995);
#9581=CIRCLE('',#26296,3.5);
#9582=CIRCLE('',#26298,3.49999999999995);
#9583=CIRCLE('',#26301,5.49999999999995);
#9584=CIRCLE('',#26302,5.49999999999995);
#9585=CIRCLE('',#26304,3.5);
#9586=CIRCLE('',#26306,3.49999999999995);
#9587=CIRCLE('',#26308,3.5);
#9588=CIRCLE('',#26309,3.49999999999995);
#9589=CIRCLE('',#26310,3.5);
#9590=CIRCLE('',#26312,3.49999999999995);
#9591=CIRCLE('',#26315,5.50000000000001);
#9592=CIRCLE('',#26316,5.50000000000001);
#9593=CIRCLE('',#26318,3.5);
#9594=CIRCLE('',#26320,3.5);
#9595=CIRCLE('',#26322,3.5);
#9596=CIRCLE('',#26323,3.5);
#9597=CIRCLE('',#26324,3.5);
#9598=CIRCLE('',#26326,3.5);
#9599=CIRCLE('',#26329,5.50000000000001);
#9600=CIRCLE('',#26330,5.50000000000001);
#9601=CIRCLE('',#26332,3.5);
#9602=CIRCLE('',#26334,3.5);
#9603=CIRCLE('',#26336,3.5);
#9604=CIRCLE('',#26337,3.5);
#9605=CIRCLE('',#26338,3.5);
#9606=CIRCLE('',#26340,3.5);
#9607=CIRCLE('',#26343,5.50000000000001);
#9608=CIRCLE('',#26344,5.50000000000001);
#9609=CIRCLE('',#26346,3.5);
#9610=CIRCLE('',#26348,3.5);
#9611=CIRCLE('',#26350,3.5);
#9612=CIRCLE('',#26351,3.5);
#9613=CIRCLE('',#26352,3.5);
#9614=CIRCLE('',#26354,3.5);
#9615=CIRCLE('',#26357,5.50000000000001);
#9616=CIRCLE('',#26358,5.50000000000001);
#9617=CIRCLE('',#26360,3.5);
#9618=CIRCLE('',#26362,3.5);
#9619=CIRCLE('',#26364,3.5);
#9620=CIRCLE('',#26365,3.5);
#9621=CIRCLE('',#26366,3.5);
#9622=CIRCLE('',#26368,3.5);
#9623=CIRCLE('',#26371,5.50000000000001);
#9624=CIRCLE('',#26372,5.50000000000001);
#9625=CIRCLE('',#26374,3.5);
#9626=CIRCLE('',#26376,3.5);
#9627=CIRCLE('',#26378,3.5);
#9628=CIRCLE('',#26379,3.5);
#9629=CIRCLE('',#26380,3.5);
#9630=CIRCLE('',#26382,3.5);
#9631=CIRCLE('',#26385,5.50000000000001);
#9632=CIRCLE('',#26386,5.50000000000001);
#9633=CIRCLE('',#26388,3.5);
#9634=CIRCLE('',#26390,3.5);
#9635=CIRCLE('',#26392,3.5);
#9636=CIRCLE('',#26393,3.5);
#9637=CIRCLE('',#26394,3.5);
#9638=CIRCLE('',#26396,3.5);
#9639=CIRCLE('',#26399,5.50000000000001);
#9640=CIRCLE('',#26400,5.50000000000001);
#9641=CIRCLE('',#26402,3.5);
#9642=CIRCLE('',#26404,3.49999999999999);
#9643=CIRCLE('',#26406,3.5);
#9644=CIRCLE('',#26407,3.5);
#9645=CIRCLE('',#26408,3.5);
#9646=CIRCLE('',#26410,3.49999999999999);
#9647=CIRCLE('',#26413,5.5);
#9648=CIRCLE('',#26414,5.5);
#9649=CIRCLE('',#26416,3.5);
#9650=CIRCLE('',#26418,3.5);
#9651=CIRCLE('',#26420,3.5);
#9652=CIRCLE('',#26421,3.5);
#9653=CIRCLE('',#26422,3.5);
#9654=CIRCLE('',#26424,3.5);
#9655=CIRCLE('',#26427,5.5);
#9656=CIRCLE('',#26428,5.5);
#9657=CIRCLE('',#26430,3.5);
#9658=CIRCLE('',#26432,3.49999999999999);
#9659=CIRCLE('',#26434,3.5);
#9660=CIRCLE('',#26435,3.5);
#9661=CIRCLE('',#26436,3.5);
#9662=CIRCLE('',#26438,3.49999999999999);
#9663=CIRCLE('',#26488,1.);
#9664=CIRCLE('',#26489,0.5);
#9665=CIRCLE('',#26490,0.5);
#9666=CIRCLE('',#26491,0.5);
#9667=CIRCLE('',#26492,2.3);
#9668=CIRCLE('',#26493,0.5);
#9669=CIRCLE('',#26494,0.5);
#9670=CIRCLE('',#26495,0.5);
#9671=CIRCLE('',#26496,0.5);
#9672=CIRCLE('',#26497,2.3);
#9673=CIRCLE('',#26498,0.5);
#9674=CIRCLE('',#26499,0.5);
#9675=CIRCLE('',#26500,2.3);
#9676=CIRCLE('',#26501,0.5);
#9677=CIRCLE('',#26502,0.5);
#9678=CIRCLE('',#26503,0.5);
#9679=CIRCLE('',#26504,0.5);
#9680=CIRCLE('',#26505,2.3);
#9681=CIRCLE('',#26506,0.5);
#9682=CIRCLE('',#26507,0.5);
#9683=CIRCLE('',#26508,0.5);
#9684=CIRCLE('',#26509,1.);
#9685=CIRCLE('',#26511,1.);
#9686=CIRCLE('',#26512,0.5);
#9687=CIRCLE('',#26513,0.5);
#9688=CIRCLE('',#26514,0.5);
#9689=CIRCLE('',#26515,2.3);
#9690=CIRCLE('',#26516,0.5);
#9691=CIRCLE('',#26517,0.5);
#9692=CIRCLE('',#26518,0.5);
#9693=CIRCLE('',#26519,0.5);
#9694=CIRCLE('',#26520,2.3);
#9695=CIRCLE('',#26521,0.5);
#9696=CIRCLE('',#26522,0.5);
#9697=CIRCLE('',#26523,2.3);
#9698=CIRCLE('',#26524,0.5);
#9699=CIRCLE('',#26525,0.5);
#9700=CIRCLE('',#26526,0.5);
#9701=CIRCLE('',#26527,0.5);
#9702=CIRCLE('',#26528,2.3);
#9703=CIRCLE('',#26529,0.5);
#9704=CIRCLE('',#26530,0.5);
#9705=CIRCLE('',#26531,0.5);
#9706=CIRCLE('',#26532,1.);
#9707=CIRCLE('',#26594,2.5);
#9708=CIRCLE('',#26595,2.5);
#9709=CIRCLE('',#26597,2.5);
#9710=CIRCLE('',#26598,2.5);
#9711=CIRCLE('',#26600,3.65);
#9712=CIRCLE('',#26601,3.65);
#9713=CIRCLE('',#26605,3.3235);
#9714=CIRCLE('',#26606,3.3235);
#9715=CIRCLE('',#26608,3.3235);
#9716=CIRCLE('',#26609,3.3235);
#9717=CIRCLE('',#26611,3.3235);
#9718=CIRCLE('',#26612,3.32349999999999);
#9719=CIRCLE('',#26614,3.32349999999999);
#9720=CIRCLE('',#26615,3.3235);
#9721=CIRCLE('',#26617,2.5);
#9722=CIRCLE('',#26618,2.5);
#9723=CIRCLE('',#26620,2.5);
#9724=CIRCLE('',#26621,2.5);
#9725=CIRCLE('',#26623,3.65);
#9726=CIRCLE('',#26624,3.65);
#9727=CIRCLE('',#26626,0.500000000000004);
#9728=CIRCLE('',#26627,0.500000000000004);
#9729=CIRCLE('',#26628,0.500000000000006);
#9730=CIRCLE('',#26632,0.5);
#9731=CIRCLE('',#26633,0.5);
#9732=CIRCLE('',#26634,0.5);
#9733=CIRCLE('',#26635,4.);
#9734=CIRCLE('',#26636,4.);
#9735=CIRCLE('',#26638,4.);
#9736=CIRCLE('',#26640,4.99995);
#9737=CIRCLE('',#26641,4.99995);
#9738=CIRCLE('',#26670,2.3);
#9739=CIRCLE('',#26671,2.3);
#9740=CIRCLE('',#26673,2.3);
#9741=CIRCLE('',#26674,2.3);
#9742=CIRCLE('',#26676,2.3);
#9743=CIRCLE('',#26677,2.3);
#9744=CIRCLE('',#26679,2.3);
#9745=CIRCLE('',#26680,2.3);
#9746=CIRCLE('',#26682,0.5);
#9747=CIRCLE('',#26683,0.5);
#9748=CIRCLE('',#26685,0.5);
#9749=CIRCLE('',#26686,0.5);
#9750=CIRCLE('',#26688,0.5);
#9751=CIRCLE('',#26689,0.5);
#9752=CIRCLE('',#26691,0.5);
#9753=CIRCLE('',#26692,0.5);
#9754=CIRCLE('',#26694,0.5);
#9755=CIRCLE('',#26695,0.5);
#9756=CIRCLE('',#26697,0.5);
#9757=CIRCLE('',#26698,0.5);
#9758=CIRCLE('',#26700,0.5);
#9759=CIRCLE('',#26701,0.5);
#9760=CIRCLE('',#26703,0.5);
#9761=CIRCLE('',#26704,0.5);
#9762=CIRCLE('',#26706,0.5);
#9763=CIRCLE('',#26707,0.5);
#9764=CIRCLE('',#26709,0.5);
#9765=CIRCLE('',#26710,0.5);
#9766=CIRCLE('',#26712,0.5);
#9767=CIRCLE('',#26713,0.5);
#9768=CIRCLE('',#26715,0.499999999999999);
#9769=CIRCLE('',#26716,0.5);
#9770=CIRCLE('',#26718,0.5);
#9771=CIRCLE('',#26719,0.5);
#9772=CIRCLE('',#26721,0.5);
#9773=CIRCLE('',#26722,0.5);
#9774=CIRCLE('',#26724,0.5);
#9775=CIRCLE('',#26725,0.5);
#9776=CIRCLE('',#26727,0.500000000000001);
#9777=CIRCLE('',#26728,0.5);
#9778=CIRCLE('',#26746,0.450000000000001);
#9779=CIRCLE('',#26747,0.450000000000001);
#9780=CIRCLE('',#26748,0.55);
#9781=CIRCLE('',#26749,2.25);
#9782=CIRCLE('',#26750,0.549999999999998);
#9783=CIRCLE('',#26751,0.55);
#9784=CIRCLE('',#26752,0.55);
#9785=CIRCLE('',#26753,0.55);
#9786=CIRCLE('',#26754,2.25);
#9787=CIRCLE('',#26755,0.55);
#9788=CIRCLE('',#26756,0.550000000000001);
#9789=CIRCLE('',#26757,2.25);
#9790=CIRCLE('',#26758,0.550000000000002);
#9791=CIRCLE('',#26759,0.55);
#9792=CIRCLE('',#26760,0.55);
#9793=CIRCLE('',#26761,0.55);
#9794=CIRCLE('',#26762,2.25);
#9795=CIRCLE('',#26763,0.55);
#9796=CIRCLE('',#26764,0.450000000000001);
#9797=CIRCLE('',#26765,0.450000000000001);
#9798=CIRCLE('',#26768,0.450000000000001);
#9799=CIRCLE('',#26771,0.450000000000001);
#9800=CIRCLE('',#26774,0.55);
#9801=CIRCLE('',#26776,2.25);
#9802=CIRCLE('',#26778,0.549999999999998);
#9803=CIRCLE('',#26781,0.55);
#9804=CIRCLE('',#26784,0.55);
#9805=CIRCLE('',#26787,0.55);
#9806=CIRCLE('',#26789,2.25);
#9807=CIRCLE('',#26791,0.55);
#9808=CIRCLE('',#26796,0.550000000000001);
#9809=CIRCLE('',#26798,2.25);
#9810=CIRCLE('',#26800,0.550000000000002);
#9811=CIRCLE('',#26803,0.55);
#9812=CIRCLE('',#26806,0.55);
#9813=CIRCLE('',#26809,0.55);
#9814=CIRCLE('',#26811,2.25);
#9815=CIRCLE('',#26813,0.55);
#9816=CIRCLE('',#26816,0.450000000000001);
#9817=CIRCLE('',#26819,0.450000000000001);
#9818=CIRCLE('',#26832,0.5);
#9819=CIRCLE('',#26834,4.99995);
#9820=CIRCLE('',#26835,0.5);
#9821=CIRCLE('',#26836,0.5);
#9822=CIRCLE('',#26837,0.5);
#9823=CIRCLE('',#26838,2.3);
#9824=CIRCLE('',#26839,0.5);
#9825=CIRCLE('',#26840,0.5);
#9826=CIRCLE('',#26841,0.5);
#9827=CIRCLE('',#26842,0.5);
#9828=CIRCLE('',#26843,2.3);
#9829=CIRCLE('',#26844,0.5);
#9830=CIRCLE('',#26845,0.5);
#9831=CIRCLE('',#26846,2.3);
#9832=CIRCLE('',#26847,0.5);
#9833=CIRCLE('',#26848,0.5);
#9834=CIRCLE('',#26849,0.5);
#9835=CIRCLE('',#26850,0.5);
#9836=CIRCLE('',#26851,2.3);
#9837=CIRCLE('',#26852,0.5);
#9838=CIRCLE('',#26853,0.5);
#9839=CIRCLE('',#26854,0.5);
#9840=CIRCLE('',#26858,0.5);
#9841=CIRCLE('',#26861,0.500000000000006);
#9842=CIRCLE('',#26873,0.5);
#9843=CIRCLE('',#26876,0.5);
#9844=CIRCLE('',#26879,0.5);
#9845=CIRCLE('',#26881,2.3);
#9846=CIRCLE('',#26883,0.499999999999999);
#9847=CIRCLE('',#26886,0.5);
#9848=CIRCLE('',#26889,0.5);
#9849=CIRCLE('',#26892,0.5);
#9850=CIRCLE('',#26894,2.3);
#9851=CIRCLE('',#26896,0.500000000000001);
#9852=CIRCLE('',#26901,0.5);
#9853=CIRCLE('',#26903,2.3);
#9854=CIRCLE('',#26905,0.5);
#9855=CIRCLE('',#26908,0.5);
#9856=CIRCLE('',#26911,0.5);
#9857=CIRCLE('',#26914,0.5);
#9858=CIRCLE('',#26916,2.3);
#9859=CIRCLE('',#26918,0.5);
#9860=CIRCLE('',#26921,0.5);
#9861=CIRCLE('',#26924,0.5);
#9862=CIRCLE('',#26932,0.500000000000006);
#9863=CIRCLE('',#26934,2.);
#9864=CIRCLE('',#26935,2.);
#9865=CIRCLE('',#26940,2.);
#9866=CIRCLE('',#26942,2.);
#9867=CIRCLE('',#26944,0.450000000000001);
#9868=CIRCLE('',#26945,0.450000000000001);
#9869=CIRCLE('',#26946,0.55);
#9870=CIRCLE('',#26947,2.25);
#9871=CIRCLE('',#26948,0.55);
#9872=CIRCLE('',#26949,0.55);
#9873=CIRCLE('',#26950,0.55);
#9874=CIRCLE('',#26951,0.550000000000002);
#9875=CIRCLE('',#26952,2.25);
#9876=CIRCLE('',#26953,0.550000000000001);
#9877=CIRCLE('',#26954,0.55);
#9878=CIRCLE('',#26955,2.25);
#9879=CIRCLE('',#26956,0.55);
#9880=CIRCLE('',#26957,0.55);
#9881=CIRCLE('',#26958,0.55);
#9882=CIRCLE('',#26959,0.549999999999998);
#9883=CIRCLE('',#26960,2.25);
#9884=CIRCLE('',#26961,0.55);
#9885=CIRCLE('',#26962,0.450000000000001);
#9886=CIRCLE('',#26963,0.450000000000001);
#9887=CIRCLE('',#26975,5.5);
#9888=CIRCLE('',#26981,5.5);
#9889=CIRCLE('',#26998,0.450000000000001);
#9890=CIRCLE('',#27001,0.450000000000001);
#9891=CIRCLE('',#27004,0.55);
#9892=CIRCLE('',#27006,2.25);
#9893=CIRCLE('',#27008,0.55);
#9894=CIRCLE('',#27011,0.55);
#9895=CIRCLE('',#27014,0.55);
#9896=CIRCLE('',#27017,0.550000000000002);
#9897=CIRCLE('',#27019,2.25);
#9898=CIRCLE('',#27021,0.550000000000001);
#9899=CIRCLE('',#27026,0.55);
#9900=CIRCLE('',#27028,2.25);
#9901=CIRCLE('',#27030,0.55);
#9902=CIRCLE('',#27033,0.55);
#9903=CIRCLE('',#27036,0.55);
#9904=CIRCLE('',#27039,0.549999999999998);
#9905=CIRCLE('',#27041,2.25);
#9906=CIRCLE('',#27043,0.55);
#9907=CIRCLE('',#27046,0.450000000000001);
#9908=CIRCLE('',#27049,0.450000000000001);
#9909=CIRCLE('',#27076,5.50000000000001);
#9910=CIRCLE('',#27084,5.49999999999999);
#9911=CIRCLE('',#27093,0.5);
#9912=CIRCLE('',#27094,0.5);
#9913=CIRCLE('',#27095,0.5);
#9914=CIRCLE('',#27096,2.3);
#9915=CIRCLE('',#27097,0.499999999999999);
#9916=CIRCLE('',#27098,0.5);
#9917=CIRCLE('',#27099,0.5);
#9918=CIRCLE('',#27100,0.5);
#9919=CIRCLE('',#27101,2.3);
#9920=CIRCLE('',#27102,0.500000000000001);
#9921=CIRCLE('',#27103,0.5);
#9922=CIRCLE('',#27104,2.3);
#9923=CIRCLE('',#27105,0.5);
#9924=CIRCLE('',#27106,0.5);
#9925=CIRCLE('',#27107,0.5);
#9926=CIRCLE('',#27108,0.5);
#9927=CIRCLE('',#27109,2.3);
#9928=CIRCLE('',#27110,0.5);
#9929=CIRCLE('',#27111,0.5);
#9930=CIRCLE('',#27112,0.5);
#9931=CIRCLE('',#27120,0.5);
#9932=CIRCLE('',#27122,0.5);
#9933=CIRCLE('',#27127,0.5);
#9934=CIRCLE('',#27129,0.5);
#9935=CIRCLE('',#27131,2.3);
#9936=CIRCLE('',#27133,0.5);
#9937=CIRCLE('',#27135,0.5);
#9938=CIRCLE('',#27139,0.5);
#9939=CIRCLE('',#27141,0.5);
#9940=CIRCLE('',#27143,2.3);
#9941=CIRCLE('',#27147,0.500000000000001);
#9942=CIRCLE('',#27149,0.5);
#9943=CIRCLE('',#27151,2.3);
#9944=CIRCLE('',#27153,0.5);
#9945=CIRCLE('',#27155,0.5);
#9946=CIRCLE('',#27160,0.499999999999999);
#9947=CIRCLE('',#27162,0.5);
#9948=CIRCLE('',#27164,2.3);
#9949=CIRCLE('',#27166,0.5);
#9950=CIRCLE('',#27168,0.5);
#9951=CIRCLE('',#27185,4.99995);
#9952=CIRCLE('',#27194,3.44123551017618);
#9953=CIRCLE('',#27195,1.21);
#9954=CIRCLE('',#27196,3.21339563862929);
#9955=CIRCLE('',#27197,2.);
#9956=CIRCLE('',#27198,3.36374346224613);
#9957=CIRCLE('',#27200,2.5);
#9958=CIRCLE('',#27202,1.09087121146357);
#9959=CIRCLE('',#27204,3.46410161513777);
#9960=CIRCLE('',#27206,3.46410161513775);
#9961=CIRCLE('',#27208,3.);
#9962=CIRCLE('',#27209,3.);
#9963=CIRCLE('',#27211,4.);
#9964=CIRCLE('',#27212,4.);
#9965=CIRCLE('',#27213,4.);
#9966=CIRCLE('',#27214,4.);
#9967=CIRCLE('',#27215,4.);
#9968=CIRCLE('',#27216,4.);
#9969=CIRCLE('',#27217,4.);
#9970=CIRCLE('',#27218,4.);
#9971=CIRCLE('',#27219,4.);
#9972=CIRCLE('',#27221,4.);
#9973=CIRCLE('',#27223,3.46410161513776);
#9974=CIRCLE('',#27224,3.46410161513777);
#9975=CIRCLE('',#27225,3.46410161513777);
#9976=CIRCLE('',#27226,3.46410161513777);
#9977=CIRCLE('',#27227,3.46410161513777);
#9978=CIRCLE('',#27229,3.46410161513775);
#9979=CIRCLE('',#27230,3.46410161513775);
#9980=CIRCLE('',#27231,3.46410161513775);
#9981=CIRCLE('',#27232,3.46410161513775);
#9982=CIRCLE('',#27233,3.46410161513776);
#9983=CIRCLE('',#27277,6.00000000000004);
#9984=CIRCLE('',#27278,6.00000000000002);
#9985=CIRCLE('',#27279,6.00000000000002);
#9986=CIRCLE('',#27281,6.20000000000003);
#9987=CIRCLE('',#27282,0.199999999999989);
#9988=CIRCLE('',#27284,7.5000000000001);
#9989=CIRCLE('',#27285,7.00000000000019);
#9990=CIRCLE('',#27287,7.50000000000011);
#9991=CIRCLE('',#27289,7.7000000000001);
#9992=CIRCLE('',#27290,0.199999999999989);
#9993=CIRCLE('',#27292,10.0000000000001);
#9994=CIRCLE('',#27293,9.00000000000005);
#9995=CIRCLE('',#27295,9.9999999999999);
#9996=CIRCLE('',#27296,9.9999999999999);
#9997=CIRCLE('',#27298,8.99999999999991);
#9998=CIRCLE('',#27300,7.5);
#9999=CIRCLE('',#27301,0.200000000000001);
#10000=CIRCLE('',#27302,7.7);
#10001=CIRCLE('',#27304,7.5);
#10002=CIRCLE('',#27306,7.15);
#10003=CIRCLE('',#27307,7.15);
#10004=CIRCLE('',#27309,7.5);
#10005=CIRCLE('',#27310,7.5);
#10006=CIRCLE('',#27311,7.5);
#10007=CIRCLE('',#27313,6.5);
#10008=CIRCLE('',#27320,5.00000000000007);
#10009=CIRCLE('',#27326,2.);
#10010=CIRCLE('',#27331,3.3);
#10011=CIRCLE('',#27332,3.29999999999999);
#10012=CIRCLE('',#27334,3.3);
#10013=CIRCLE('',#27335,3.29999999999999);
#10014=CIRCLE('',#27337,3.3);
#10015=CIRCLE('',#27338,3.3);
#10016=CIRCLE('',#27340,3.3);
#10017=CIRCLE('',#27341,3.3);
#10018=CIRCLE('',#27343,3.3);
#10019=CIRCLE('',#27344,3.29999999999999);
#10020=CIRCLE('',#27346,3.3);
#10021=CIRCLE('',#27347,3.3);
#10022=CIRCLE('',#27349,18.);
#10023=CIRCLE('',#27350,18.);
#10024=CIRCLE('',#27352,13.);
#10025=CIRCLE('',#27353,13.);
#10026=CIRCLE('',#27355,12.75);
#10027=CIRCLE('',#27356,12.75);
#10028=CIRCLE('',#27358,10.);
#10029=CIRCLE('',#27359,10.);
#10030=CIRCLE('',#27361,12.75);
#10031=CIRCLE('',#27362,12.75);
#10032=CIRCLE('',#27364,13.);
#10033=CIRCLE('',#27365,13.);
#10034=CIRCLE('',#27367,17.5);
#10035=CIRCLE('',#27368,0.5);
#10036=CIRCLE('',#27370,28.);
#10037=CIRCLE('',#27371,28.);
#10038=CIRCLE('',#27373,29.);
#10039=CIRCLE('',#27375,29.);
#10040=CIRCLE('',#27377,29.);
#10041=CIRCLE('',#27379,29.);
#10042=CIRCLE('',#27381,28.);
#10043=CIRCLE('',#27383,28.);
#10044=CIRCLE('',#27397,16.);
#10045=CIRCLE('',#27398,16.);
#10046=CIRCLE('',#27400,7.5);
#10047=CIRCLE('',#27401,7.5);
#10048=CIRCLE('',#27403,16.);
#10049=CIRCLE('',#27404,16.);
#10050=CIRCLE('',#27406,5.5);
#10051=CIRCLE('',#27407,5.5);
#10052=CIRCLE('',#27409,3.29999999999999);
#10053=CIRCLE('',#27410,3.3);
#10054=CIRCLE('',#27412,5.5);
#10055=CIRCLE('',#27413,5.5);
#10056=CIRCLE('',#27415,3.29999999999999);
#10057=CIRCLE('',#27416,3.3);
#10058=CIRCLE('',#27437,0.85);
#10059=CIRCLE('',#27438,0.85);
#10060=CIRCLE('',#27440,0.85);
#10061=CIRCLE('',#27441,0.85);
#10062=CIRCLE('',#27443,7.15);
#10063=CIRCLE('',#27444,7.15);
#10064=CIRCLE('',#27446,8.8);
#10065=CIRCLE('',#27447,8.8);
#10066=CIRCLE('',#27449,1.9);
#10067=CIRCLE('',#27450,1.9);
#10068=CIRCLE('',#27451,1.9);
#10069=CIRCLE('',#27452,1.9);
#10070=CIRCLE('',#27454,1.9);
#10071=CIRCLE('',#27455,1.9);
#10072=CIRCLE('',#27456,1.9);
#10073=CIRCLE('',#27457,1.9);
#10074=CIRCLE('',#27473,14.);
#10075=CIRCLE('',#27474,14.);
#10076=CIRCLE('',#27476,9.75);
#10077=CIRCLE('',#27477,9.75);
#10078=CIRCLE('',#27479,7.5);
#10079=CIRCLE('',#27480,7.5);
#10080=CIRCLE('',#27482,9.75);
#10081=CIRCLE('',#27483,9.75);
#10082=CIRCLE('',#27485,14.);
#10083=CIRCLE('',#27486,14.);
#10084=CIRCLE('',#27488,3.1);
#10085=CIRCLE('',#27489,3.1);
#10086=CIRCLE('',#27491,3.1);
#10087=CIRCLE('',#27492,3.1);
#10088=CIRCLE('',#27494,3.1);
#10089=CIRCLE('',#27495,3.1);
#10090=CIRCLE('',#27497,3.1);
#10091=CIRCLE('',#27498,3.1);
#10092=CIRCLE('',#27500,3.50000000000001);
#10093=CIRCLE('',#27501,3.50000000000001);
#10094=CIRCLE('',#27503,3.5);
#10095=CIRCLE('',#27504,3.5);
#10096=CIRCLE('',#27506,3.50000000000001);
#10097=CIRCLE('',#27507,3.50000000000001);
#10098=CIRCLE('',#27509,3.50000000000001);
#10099=CIRCLE('',#27510,3.50000000000001);
#10100=CIRCLE('',#27512,5.5);
#10101=CIRCLE('',#27513,5.5);
#10102=CIRCLE('',#27515,3.29999999999999);
#10103=CIRCLE('',#27516,3.3);
#10104=CIRCLE('',#27518,5.5);
#10105=CIRCLE('',#27519,5.5);
#10106=CIRCLE('',#27521,3.29999999999999);
#10107=CIRCLE('',#27522,3.3);
#10108=CIRCLE('',#27524,5.5);
#10109=CIRCLE('',#27525,5.5);
#10110=CIRCLE('',#27527,3.29999999999999);
#10111=CIRCLE('',#27528,3.3);
#10112=CIRCLE('',#27530,5.5);
#10113=CIRCLE('',#27531,5.5);
#10114=CIRCLE('',#27533,3.29999999999999);
#10115=CIRCLE('',#27534,3.3);
#10116=CIRCLE('',#27604,1.);
#10117=CIRCLE('',#27605,1.);
#10118=CIRCLE('',#27606,1.);
#10119=CIRCLE('',#27607,1.);
#10120=CIRCLE('',#27608,1.);
#10121=CIRCLE('',#27609,1.);
#10122=CIRCLE('',#27611,2.);
#10123=CIRCLE('',#27614,2.);
#10124=CIRCLE('',#27615,1.25);
#10125=CIRCLE('',#27616,2.);
#10126=CIRCLE('',#27619,6.9585);
#10127=CIRCLE('',#27620,7.5);
#10128=CIRCLE('',#27621,6.9585);
#10129=CIRCLE('',#27623,6.9585);
#10130=CIRCLE('',#27624,7.5);
#10131=CIRCLE('',#27626,12.5);
#10132=CIRCLE('',#27627,12.5);
#10133=CIRCLE('',#27629,10.5);
#10134=CIRCLE('',#27630,10.5);
#10135=CIRCLE('',#27633,12.5);
#10136=CIRCLE('',#27634,49.725094979045);
#10137=CIRCLE('',#27635,49.7250949790431);
#10138=CIRCLE('',#27636,12.5);
#10139=CIRCLE('',#27637,49.7250949790141);
#10140=CIRCLE('',#27638,49.7250949790647);
#10141=CIRCLE('',#27640,12.5);
#10142=CIRCLE('',#27641,12.5);
#10143=CIRCLE('',#27643,12.5);
#10144=CIRCLE('',#27644,12.5);
#10145=CIRCLE('',#27646,12.5);
#10146=CIRCLE('',#27647,12.5);
#10147=CIRCLE('',#27670,9.75);
#10148=CIRCLE('',#27671,9.75);
#10149=CIRCLE('',#27673,7.5);
#10150=CIRCLE('',#27674,7.5);
#10151=CIRCLE('',#27683,3.);
#10152=CIRCLE('',#27684,3.);
#10153=CIRCLE('',#27686,3.);
#10154=CIRCLE('',#27687,3.);
#10155=CIRCLE('',#27689,3.25);
#10156=CIRCLE('',#27690,3.25);
#10157=CIRCLE('',#27692,3.25);
#10158=CIRCLE('',#27693,3.25);
#10159=CIRCLE('',#27695,3.25);
#10160=CIRCLE('',#27696,3.25);
#10161=CIRCLE('',#27698,3.25);
#10162=CIRCLE('',#27699,3.25);
#10163=CIRCLE('',#27716,2.);
#10164=CIRCLE('',#27718,2.);
#10165=CIRCLE('',#27720,2.);
#10166=CIRCLE('',#27722,2.);
#10167=CIRCLE('',#27723,1.000000009999);
#10168=CIRCLE('',#27724,1.000000122615);
#10169=CIRCLE('',#27725,1.000000000939);
#10170=CIRCLE('',#27726,39.901435785627);
#10171=CIRCLE('',#27727,0.999999999999998);
#10172=CIRCLE('',#27728,38.8921101653477);
#10173=CIRCLE('',#27730,1.00000197298164);
#10174=CIRCLE('',#27731,1.000005019194);
#10175=CIRCLE('',#27732,1.00001938568424);
#10176=CIRCLE('',#27734,1.000000068316);
#10177=CIRCLE('',#27735,1.00001946091789);
#10178=CIRCLE('',#27737,1.000005006638);
#10179=CIRCLE('',#27738,1.000000068317);
#10180=CIRCLE('',#27739,39.8991935477595);
#10181=CIRCLE('',#27740,38.874817547618);
#10182=CIRCLE('',#27741,1.000000000939);
#10183=CIRCLE('',#27743,1.00003031349091);
#10184=CIRCLE('',#27744,0.999996385196527);
#10185=CIRCLE('',#27745,1.000000122615);
#10186=CIRCLE('',#27746,1.000000000939);
#10187=CIRCLE('',#27747,39.9014357641817);
#10188=CIRCLE('',#27748,0.999999999999999);
#10189=CIRCLE('',#27749,38.8921101994134);
#10190=CIRCLE('',#27751,1.00000197297109);
#10191=CIRCLE('',#27752,1.000005019194);
#10192=CIRCLE('',#27753,1.00000191452219);
#10193=CIRCLE('',#27754,1.00001938569039);
#10194=CIRCLE('',#27756,1.000000068316);
#10195=CIRCLE('',#27757,1.00001946091372);
#10196=CIRCLE('',#27759,1.000005006638);
#10197=CIRCLE('',#27760,1.000000068317);
#10198=CIRCLE('',#27761,39.8991935573533);
#10199=CIRCLE('',#27762,38.8748146429027);
#10200=CIRCLE('',#27763,1.000000000939);
#10201=CIRCLE('',#27765,1.00003031350209);
#10202=CIRCLE('',#27766,0.999996390589362);
#10203=CIRCLE('',#27767,1.000000122615);
#10204=CIRCLE('',#27768,1.000000000939);
#10205=CIRCLE('',#27769,39.9014357932221);
#10206=CIRCLE('',#27770,1.);
#10207=CIRCLE('',#27771,38.8921101598015);
#10208=CIRCLE('',#27773,1.00000197298478);
#10209=CIRCLE('',#27774,1.000005019194);
#10210=CIRCLE('',#27775,1.00001938568406);
#10211=CIRCLE('',#27777,1.000000068316);
#10212=CIRCLE('',#27778,1.00001946091692);
#10213=CIRCLE('',#27780,1.000005006638);
#10214=CIRCLE('',#27781,1.000000068317);
#10215=CIRCLE('',#27782,39.899193552042);
#10216=CIRCLE('',#27783,38.8748161532142);
#10217=CIRCLE('',#27784,1.000000000939);
#10218=CIRCLE('',#27786,1.00003031349466);
#10219=CIRCLE('',#27787,0.999996305682662);
#10220=CIRCLE('',#27788,1.000000009973);
#10221=CIRCLE('',#27789,1.000000122615);
#10222=CIRCLE('',#27790,1.000000000939);
#10223=CIRCLE('',#27791,39.9014357779458);
#10224=CIRCLE('',#27792,0.999999999999999);
#10225=CIRCLE('',#27793,38.8921099760719);
#10226=CIRCLE('',#27795,1.00000197298803);
#10227=CIRCLE('',#27796,1.0000050192);
#10228=CIRCLE('',#27797,1.00001938562544);
#10229=CIRCLE('',#27799,1.000000068316);
#10230=CIRCLE('',#27800,1.0000000086);
#10231=CIRCLE('',#27801,1.00001946091164);
#10232=CIRCLE('',#27803,1.000005006635);
#10233=CIRCLE('',#27804,1.000000068317);
#10234=CIRCLE('',#27805,39.8991935595103);
#10235=CIRCLE('',#27806,38.8748146565752);
#10236=CIRCLE('',#27807,1.000000000939);
#10237=CIRCLE('',#27809,1.00003031414254);
#10238=CIRCLE('',#27810,1.000000004171);
#10239=CIRCLE('',#27811,1.000000122616);
#10240=CIRCLE('',#27812,1.000000000939);
#10241=CIRCLE('',#27813,39.9014357924868);
#10242=CIRCLE('',#27814,1.);
#10243=CIRCLE('',#27815,38.8921099732382);
#10244=CIRCLE('',#27817,1.00000197301089);
#10245=CIRCLE('',#27818,1.0000050192);
#10246=CIRCLE('',#27819,1.00000191098175);
#10247=CIRCLE('',#27820,1.00001938561266);
#10248=CIRCLE('',#27822,1.000000068316);
#10249=CIRCLE('',#27823,1.00001946090666);
#10250=CIRCLE('',#27825,1.000005006635);
#10251=CIRCLE('',#27826,1.000000068317);
#10252=CIRCLE('',#27827,39.8991935511885);
#10253=CIRCLE('',#27828,38.8748175664677);
#10254=CIRCLE('',#27829,1.000000000939);
#10255=CIRCLE('',#27831,1.00003031414535);
#10256=CIRCLE('',#27832,1.000000122616);
#10257=CIRCLE('',#27833,1.000000000939);
#10258=CIRCLE('',#27834,39.9014357636129);
#10259=CIRCLE('',#27835,1.);
#10260=CIRCLE('',#27836,38.8921099760377);
#10261=CIRCLE('',#27838,1.0000019729999);
#10262=CIRCLE('',#27839,1.0000050192);
#10263=CIRCLE('',#27840,1.00001938562086);
#10264=CIRCLE('',#27842,1.000000068316);
#10265=CIRCLE('',#27843,0.999996375475787);
#10266=CIRCLE('',#27844,1.0000194609088);
#10267=CIRCLE('',#27846,1.000005006635);
#10268=CIRCLE('',#27847,1.000000068317);
#10269=CIRCLE('',#27848,39.8991935494084);
#10270=CIRCLE('',#27849,38.874816056833);
#10271=CIRCLE('',#27850,1.000000000939);
#10272=CIRCLE('',#27852,1.00003031413779);
#10273=CIRCLE('',#27853,0.999996384223477);
#10274=CIRCLE('',#27854,1.000000122614);
#10275=CIRCLE('',#27855,1.00000197292957);
#10276=CIRCLE('',#27856,1.000005019194);
#10277=CIRCLE('',#27858,1.);
#10278=CIRCLE('',#27859,1.00000000094);
#10279=CIRCLE('',#27860,39.9014356027643);
#10280=CIRCLE('',#27861,38.8921102040137);
#10281=CIRCLE('',#27862,39.8991935568584);
#10282=CIRCLE('',#27863,1.00000000094);
#10283=CIRCLE('',#27864,1.000005006638);
#10284=CIRCLE('',#27866,1.0000303135037);
#10285=CIRCLE('',#27867,0.999996369425503);
#10286=CIRCLE('',#27868,0.999976684049138);
#10287=CIRCLE('',#27869,1.00001946095475);
#10288=CIRCLE('',#27871,1.000000068378);
#10289=CIRCLE('',#27872,1.000000068377);
#10290=CIRCLE('',#27873,38.8748167422972);
#10291=CIRCLE('',#27875,1.00001938573349);
#10292=CIRCLE('',#27876,1.000000251468);
#10293=CIRCLE('',#27877,1.000000122616);
#10294=CIRCLE('',#27878,1.000000000939);
#10295=CIRCLE('',#27879,39.9014357922065);
#10296=CIRCLE('',#27880,0.999999999999998);
#10297=CIRCLE('',#27881,38.8921099729939);
#10298=CIRCLE('',#27883,1.00000197301321);
#10299=CIRCLE('',#27884,1.0000050192);
#10300=CIRCLE('',#27885,1.00000650505067);
#10301=CIRCLE('',#27886,1.00001938561205);
#10302=CIRCLE('',#27888,1.000000068316);
#10303=CIRCLE('',#27889,1.0000194609075);
#10304=CIRCLE('',#27891,1.000005006635);
#10305=CIRCLE('',#27892,1.000000068317);
#10306=CIRCLE('',#27893,39.8991935508386);
#10307=CIRCLE('',#27894,38.8748160719392);
#10308=CIRCLE('',#27895,1.000000000939);
#10309=CIRCLE('',#27897,1.00003031415272);
#10310=CIRCLE('',#27898,1.000000046838);
#10311=CIRCLE('',#27899,14.88340478034);
#10312=CIRCLE('',#27900,14.88340478034);
#10313=CIRCLE('',#27901,14.88340478034);
#10314=CIRCLE('',#27902,14.88340478034);
#10315=CIRCLE('',#27903,14.88340478034);
#10316=CIRCLE('',#27904,14.88340478034);
#10317=CIRCLE('',#27905,14.88340478034);
#10318=CIRCLE('',#27906,14.88340478034);
#10319=CIRCLE('',#27907,14.88340478034);
#10320=CIRCLE('',#27908,14.88340478034);
#10321=CIRCLE('',#27909,14.88340478034);
#10322=CIRCLE('',#27910,14.88340478034);
#10323=CIRCLE('',#27911,14.88340478034);
#10324=CIRCLE('',#27912,14.88340478034);
#10325=CIRCLE('',#27913,14.88340478034);
#10326=CIRCLE('',#27914,14.88340478034);
#10327=CIRCLE('',#27916,2.);
#10328=CIRCLE('',#27918,2.);
#10329=CIRCLE('',#27920,2.);
#10330=CIRCLE('',#27922,2.);
#10331=CIRCLE('',#27924,2.);
#10332=CIRCLE('',#27926,2.);
#10333=CIRCLE('',#27928,13.5);
#10334=CIRCLE('',#27930,13.5);
#10335=CIRCLE('',#27932,2.);
#10336=CIRCLE('',#27934,2.);
#10337=CIRCLE('',#27936,2.);
#10338=CIRCLE('',#27938,2.);
#10339=CIRCLE('',#27940,2.);
#10340=CIRCLE('',#27942,2.);
#10341=CIRCLE('',#27946,2.5);
#10342=CIRCLE('',#27948,2.5);
#10343=CIRCLE('',#27959,5.);
#10344=CIRCLE('',#27960,3.);
#10345=CIRCLE('',#27962,5.);
#10346=CIRCLE('',#27964,0.6);
#10347=CIRCLE('',#27965,4.4);
#10348=CIRCLE('',#27975,2.38655);
#10349=CIRCLE('',#27977,3.);
#10350=CIRCLE('',#27981,5.);
#10351=CIRCLE('',#27982,3.);
#10352=CIRCLE('',#27984,5.);
#10353=CIRCLE('',#27986,0.6);
#10354=CIRCLE('',#27987,4.4);
#10355=CIRCLE('',#27997,2.38655);
#10356=CIRCLE('',#27999,3.);
#10357=CIRCLE('',#28003,26.);
#10358=CIRCLE('',#28004,6.);
#10359=CIRCLE('',#28006,27.5);
#10360=CIRCLE('',#28008,13.);
#10361=CIRCLE('',#28009,27.5);
#10362=CIRCLE('',#28010,13.);
#10363=CIRCLE('',#28011,17.5);
#10364=CIRCLE('',#28013,13.);
#10365=CIRCLE('',#28014,27.5);
#10366=CIRCLE('',#28015,13.);
#10367=CIRCLE('',#28016,17.5);
#10368=CIRCLE('',#28018,17.5);
#10369=CIRCLE('',#28020,17.5);
#10370=CIRCLE('',#28022,13.);
#10371=CIRCLE('',#28024,13.);
#10372=CIRCLE('',#28026,13.);
#10373=CIRCLE('',#28028,13.);
#10374=CIRCLE('',#28030,27.5);
#10375=CIRCLE('',#28031,27.5);
#10376=CIRCLE('',#28032,27.5);
#10377=CIRCLE('',#28034,6.);
#10378=CIRCLE('',#28037,2.5);
#10379=CIRCLE('',#28039,5.5);
#10380=CIRCLE('',#28040,3.3);
#10381=CIRCLE('',#28042,3.3);
#10382=CIRCLE('',#28044,2.5);
#10383=CIRCLE('',#28046,2.5);
#10384=CIRCLE('',#28051,5.5);
#10385=CIRCLE('',#28053,2.5);
#10386=CIRCLE('',#28056,2.5);
#10387=CIRCLE('',#28057,2.5);
#10388=CIRCLE('',#28059,3.3);
#10389=CIRCLE('',#28061,3.3);
#10390=CIRCLE('',#28065,6.);
#10391=CIRCLE('',#28066,6.);
#10392=CIRCLE('',#28067,26.);
#10393=CIRCLE('',#28069,27.5);
#10394=CIRCLE('',#28071,27.5);
#10395=CIRCLE('',#28072,13.);
#10396=CIRCLE('',#28073,17.5);
#10397=CIRCLE('',#28074,13.);
#10398=CIRCLE('',#28075,27.5);
#10399=CIRCLE('',#28076,13.);
#10400=CIRCLE('',#28077,17.5);
#10401=CIRCLE('',#28078,13.);
#10402=CIRCLE('',#28079,27.5);
#10403=CIRCLE('',#28080,6.);
#10404=CIRCLE('',#28081,6.);
#10405=CIRCLE('',#28085,27.5);
#10406=CIRCLE('',#28087,2.1);
#10407=CIRCLE('',#28088,2.1);
#10408=CIRCLE('',#28089,2.1);
#10409=CIRCLE('',#28097,13.);
#10410=CIRCLE('',#28099,13.);
#10411=CIRCLE('',#28101,13.);
#10412=CIRCLE('',#28103,17.5);
#10413=CIRCLE('',#28105,17.5);
#10414=CIRCLE('',#28107,13.);
#10415=CIRCLE('',#28109,27.5);
#10416=CIRCLE('',#28111,27.5);
#10417=CIRCLE('',#28113,30.7157076297161);
#10418=CIRCLE('',#28114,30.7139923780105);
#10419=CIRCLE('',#28115,27.5);
#10420=CIRCLE('',#28116,27.5);
#10421=CIRCLE('',#28117,27.5);
#10422=CIRCLE('',#28118,27.5);
#10423=CIRCLE('',#28119,27.5);
#10424=CIRCLE('',#28120,27.5);
#10425=CIRCLE('',#28126,37.5686105496298);
#10426=CIRCLE('',#28127,27.5);
#10427=CIRCLE('',#28128,27.5);
#10428=CIRCLE('',#28129,27.5);
#10429=CIRCLE('',#28130,39.9577086924719);
#10430=CIRCLE('',#28137,27.);
#10431=CIRCLE('',#28138,27.);
#10432=CIRCLE('',#28139,27.);
#10433=CIRCLE('',#28140,27.);
#10434=CIRCLE('',#28156,39.2292319119626);
#10435=CIRCLE('',#28158,27.);
#10436=CIRCLE('',#28161,27.);
#10437=CIRCLE('',#28164,27.);
#10438=CIRCLE('',#28191,30.1550686144397);
#10439=CIRCLE('',#28194,30.1568155811873);
#10440=CIRCLE('',#28198,27.);
#10441=CIRCLE('',#28201,27.);
#10442=CIRCLE('',#28204,27.);
#10443=CIRCLE('',#28211,2.5);
#10444=CIRCLE('',#28213,2.5);
#10445=CIRCLE('',#28224,5.);
#10446=CIRCLE('',#28225,3.);
#10447=CIRCLE('',#28227,5.);
#10448=CIRCLE('',#28229,0.6);
#10449=CIRCLE('',#28230,4.4);
#10450=CIRCLE('',#28240,2.38655);
#10451=CIRCLE('',#28242,3.);
#10452=CIRCLE('',#28246,5.);
#10453=CIRCLE('',#28247,3.);
#10454=CIRCLE('',#28249,5.);
#10455=CIRCLE('',#28251,0.6);
#10456=CIRCLE('',#28252,4.4);
#10457=CIRCLE('',#28262,2.38655);
#10458=CIRCLE('',#28264,3.);
#10459=CIRCLE('',#28268,26.);
#10460=CIRCLE('',#28269,9.5);
#10461=CIRCLE('',#28271,27.5);
#10462=CIRCLE('',#28273,13.);
#10463=CIRCLE('',#28274,27.5);
#10464=CIRCLE('',#28275,13.);
#10465=CIRCLE('',#28276,17.5);
#10466=CIRCLE('',#28278,13.);
#10467=CIRCLE('',#28279,27.5);
#10468=CIRCLE('',#28280,13.);
#10469=CIRCLE('',#28281,17.5);
#10470=CIRCLE('',#28283,17.5);
#10471=CIRCLE('',#28285,17.5);
#10472=CIRCLE('',#28287,13.);
#10473=CIRCLE('',#28289,13.);
#10474=CIRCLE('',#28291,13.);
#10475=CIRCLE('',#28293,13.);
#10476=CIRCLE('',#28295,27.5);
#10477=CIRCLE('',#28296,27.5);
#10478=CIRCLE('',#28297,27.5);
#10479=CIRCLE('',#28299,9.5);
#10480=CIRCLE('',#28302,2.5);
#10481=CIRCLE('',#28304,5.5);
#10482=CIRCLE('',#28305,3.3);
#10483=CIRCLE('',#28307,3.3);
#10484=CIRCLE('',#28309,2.5);
#10485=CIRCLE('',#28311,2.5);
#10486=CIRCLE('',#28316,5.5);
#10487=CIRCLE('',#28318,2.5);
#10488=CIRCLE('',#28321,2.5);
#10489=CIRCLE('',#28322,2.5);
#10490=CIRCLE('',#28324,3.3);
#10491=CIRCLE('',#28326,3.3);
#10492=CIRCLE('',#28330,9.5);
#10493=CIRCLE('',#28331,9.5);
#10494=CIRCLE('',#28332,26.);
#10495=CIRCLE('',#28334,27.5);
#10496=CIRCLE('',#28336,27.5);
#10497=CIRCLE('',#28337,13.);
#10498=CIRCLE('',#28338,17.5);
#10499=CIRCLE('',#28339,13.);
#10500=CIRCLE('',#28340,27.5);
#10501=CIRCLE('',#28341,13.);
#10502=CIRCLE('',#28342,17.5);
#10503=CIRCLE('',#28343,13.);
#10504=CIRCLE('',#28344,27.5);
#10505=CIRCLE('',#28345,9.5);
#10506=CIRCLE('',#28346,9.5);
#10507=CIRCLE('',#28350,27.5);
#10508=CIRCLE('',#28352,2.1);
#10509=CIRCLE('',#28357,13.);
#10510=CIRCLE('',#28359,13.);
#10511=CIRCLE('',#28361,13.);
#10512=CIRCLE('',#28363,17.5);
#10513=CIRCLE('',#28365,17.5);
#10514=CIRCLE('',#28367,13.);
#10515=CIRCLE('',#28369,27.5);
#10516=CIRCLE('',#28371,27.5);
#10517=CIRCLE('',#28373,30.7157076295626);
#10518=CIRCLE('',#28374,30.7139923779046);
#10519=CIRCLE('',#28375,27.5);
#10520=CIRCLE('',#28376,27.5);
#10521=CIRCLE('',#28377,27.5);
#10522=CIRCLE('',#28378,27.5);
#10523=CIRCLE('',#28379,27.5);
#10524=CIRCLE('',#28380,27.5);
#10525=CIRCLE('',#28386,37.5686105495472);
#10526=CIRCLE('',#28387,27.5);
#10527=CIRCLE('',#28388,27.5);
#10528=CIRCLE('',#28389,27.5);
#10529=CIRCLE('',#28390,39.9577086923309);
#10530=CIRCLE('',#28397,27.);
#10531=CIRCLE('',#28398,27.);
#10532=CIRCLE('',#28399,27.);
#10533=CIRCLE('',#28400,27.);
#10534=CIRCLE('',#28416,39.2292319120603);
#10535=CIRCLE('',#28418,27.);
#10536=CIRCLE('',#28421,27.);
#10537=CIRCLE('',#28424,27.);
#10538=CIRCLE('',#28451,30.15506861437);
#10539=CIRCLE('',#28454,30.1568155811663);
#10540=CIRCLE('',#28458,27.);
#10541=CIRCLE('',#28461,27.);
#10542=CIRCLE('',#28464,27.);
#10543=CIRCLE('',#28481,2.5);
#10544=CIRCLE('',#28482,2.5);
#10545=CIRCLE('',#28485,2.5);
#10546=CIRCLE('',#28486,2.5);
#10547=CIRCLE('',#28489,2.5);
#10548=CIRCLE('',#28490,2.5);
#10549=CIRCLE('',#28493,2.5);
#10550=CIRCLE('',#28494,2.5);
#10551=CIRCLE('',#28497,2.5);
#10552=CIRCLE('',#28498,2.5);
#10553=CIRCLE('',#28501,2.5);
#10554=CIRCLE('',#28502,2.5);
#10555=CIRCLE('',#28505,2.5);
#10556=CIRCLE('',#28506,2.5);
#10557=CIRCLE('',#28509,2.5);
#10558=CIRCLE('',#28510,2.5);
#10559=CIRCLE('',#28513,2.5);
#10560=CIRCLE('',#28514,2.5);
#10561=CIRCLE('',#28517,2.5);
#10562=CIRCLE('',#28518,2.5);
#10563=CIRCLE('',#28521,2.5);
#10564=CIRCLE('',#28522,2.5);
#10565=CIRCLE('',#28525,2.5);
#10566=CIRCLE('',#28526,2.5);
#10567=CIRCLE('',#28529,2.5);
#10568=CIRCLE('',#28530,2.5);
#10569=CIRCLE('',#28533,2.5);
#10570=CIRCLE('',#28534,2.5);
#10571=CIRCLE('',#28537,2.5);
#10572=CIRCLE('',#28538,2.5);
#10573=CIRCLE('',#28541,2.5);
#10574=CIRCLE('',#28542,2.5);
#10575=CIRCLE('',#28545,2.5);
#10576=CIRCLE('',#28546,2.5);
#10577=CIRCLE('',#28550,0.200000000000001);
#10578=CIRCLE('',#28551,0.200000000000001);
#10579=CIRCLE('',#28554,0.200000000000001);
#10580=CIRCLE('',#28555,0.200000000000001);
#10581=CIRCLE('',#28566,5.);
#10582=CIRCLE('',#28567,5.);
#10583=CIRCLE('',#28569,4.4);
#10584=CIRCLE('',#28571,3.);
#10585=CIRCLE('',#28572,2.4585);
#10586=CIRCLE('',#28573,3.);
#10587=CIRCLE('',#28575,3.);
#10588=CIRCLE('',#28588,4.25);
#10589=CIRCLE('',#28589,4.25);
#10590=CIRCLE('',#28590,3.75);
#10591=CIRCLE('',#28592,2.);
#10592=CIRCLE('',#28593,2.);
#10593=CIRCLE('',#28594,2.);
#10594=CIRCLE('',#28595,2.);
#10595=CIRCLE('',#28596,2.);
#10596=CIRCLE('',#28597,2.);
#10597=CIRCLE('',#28598,2.);
#10598=CIRCLE('',#28600,4.25);
#10599=CIRCLE('',#28602,2.065);
#10600=CIRCLE('',#28603,2.065);
#10601=CIRCLE('',#28605,3.);
#10602=CIRCLE('',#28606,3.);
#10603=CIRCLE('',#28624,5.);
#10604=CIRCLE('',#28625,5.);
#10605=CIRCLE('',#28627,2.5);
#10606=CIRCLE('',#28628,2.5);
#10607=CIRCLE('',#28632,4.25);
#10608=CIRCLE('',#28633,4.25);
#10609=CIRCLE('',#28635,2.5);
#10610=CIRCLE('',#28636,2.5);
#10611=CIRCLE('',#28643,4.);
#10612=CIRCLE('',#28644,4.);
#10613=CIRCLE('',#28646,4.);
#10614=CIRCLE('',#28647,4.);
#10615=CIRCLE('',#28649,3.25);
#10616=CIRCLE('',#28650,3.25);
#10617=CIRCLE('',#28652,3.25);
#10618=CIRCLE('',#28653,3.25);
#10619=CIRCLE('',#28655,3.25);
#10620=CIRCLE('',#28656,3.25);
#10621=CIRCLE('',#28658,3.25);
#10622=CIRCLE('',#28659,3.25);
#10623=CIRCLE('',#28661,3.25);
#10624=CIRCLE('',#28662,3.25);
#10625=CIRCLE('',#28664,3.25);
#10626=CIRCLE('',#28665,3.25);
#10627=CIRCLE('',#28667,3.25);
#10628=CIRCLE('',#28668,3.25);
#10629=CIRCLE('',#28670,3.25);
#10630=CIRCLE('',#28671,3.25);
#10631=CIRCLE('',#28682,5.);
#10632=CIRCLE('',#28683,5.);
#10633=CIRCLE('',#28685,4.4);
#10634=CIRCLE('',#28687,3.);
#10635=CIRCLE('',#28688,2.4585);
#10636=CIRCLE('',#28689,3.);
#10637=CIRCLE('',#28691,3.);
#10638=VERTEX_POINT('',#36178);
#10639=VERTEX_POINT('',#36180);
#10640=VERTEX_POINT('',#36184);
#10641=VERTEX_POINT('',#36186);
#10642=VERTEX_POINT('',#36190);
#10643=VERTEX_POINT('',#36192);
#10644=VERTEX_POINT('',#36196);
#10645=VERTEX_POINT('',#36198);
#10646=VERTEX_POINT('',#36202);
#10647=VERTEX_POINT('',#36203);
#10648=VERTEX_POINT('',#36205);
#10649=VERTEX_POINT('',#36207);
#10650=VERTEX_POINT('',#36211);
#10651=VERTEX_POINT('',#36213);
#10652=VERTEX_POINT('',#36217);
#10653=VERTEX_POINT('',#36219);
#10654=VERTEX_POINT('',#36226);
#10655=VERTEX_POINT('',#36227);
#10656=VERTEX_POINT('',#36229);
#10657=VERTEX_POINT('',#36231);
#10658=VERTEX_POINT('',#36234);
#10659=VERTEX_POINT('',#36235);
#10660=VERTEX_POINT('',#36237);
#10661=VERTEX_POINT('',#36239);
#10662=VERTEX_POINT('',#36243);
#10663=VERTEX_POINT('',#36244);
#10664=VERTEX_POINT('',#36246);
#10665=VERTEX_POINT('',#36248);
#10666=VERTEX_POINT('',#36251);
#10667=VERTEX_POINT('',#36252);
#10668=VERTEX_POINT('',#36254);
#10669=VERTEX_POINT('',#36256);
#10670=VERTEX_POINT('',#36278);
#10671=VERTEX_POINT('',#36280);
#10672=VERTEX_POINT('',#36284);
#10673=VERTEX_POINT('',#36286);
#10674=VERTEX_POINT('',#36290);
#10675=VERTEX_POINT('',#36292);
#10676=VERTEX_POINT('',#36296);
#10677=VERTEX_POINT('',#36298);
#10678=VERTEX_POINT('',#36302);
#10679=VERTEX_POINT('',#36303);
#10680=VERTEX_POINT('',#36305);
#10681=VERTEX_POINT('',#36307);
#10682=VERTEX_POINT('',#36311);
#10683=VERTEX_POINT('',#36313);
#10684=VERTEX_POINT('',#36315);
#10685=VERTEX_POINT('',#36317);
#10686=VERTEX_POINT('',#36321);
#10687=VERTEX_POINT('',#36322);
#10688=VERTEX_POINT('',#36325);
#10689=VERTEX_POINT('',#36329);
#10690=VERTEX_POINT('',#36330);
#10691=VERTEX_POINT('',#36332);
#10692=VERTEX_POINT('',#36335);
#10693=VERTEX_POINT('',#36339);
#10694=VERTEX_POINT('',#36341);
#10695=VERTEX_POINT('',#36346);
#10696=VERTEX_POINT('',#36351);
#10697=VERTEX_POINT('',#36357);
#10698=VERTEX_POINT('',#36365);
#10699=VERTEX_POINT('',#36367);
#10700=VERTEX_POINT('',#36371);
#10701=VERTEX_POINT('',#36373);
#10702=VERTEX_POINT('',#36377);
#10703=VERTEX_POINT('',#36379);
#10704=VERTEX_POINT('',#36383);
#10705=VERTEX_POINT('',#36385);
#10706=VERTEX_POINT('',#36389);
#10707=VERTEX_POINT('',#36391);
#10708=VERTEX_POINT('',#36395);
#10709=VERTEX_POINT('',#36397);
#10710=VERTEX_POINT('',#36401);
#10711=VERTEX_POINT('',#36403);
#10712=VERTEX_POINT('',#36407);
#10713=VERTEX_POINT('',#36409);
#10714=VERTEX_POINT('',#36413);
#10715=VERTEX_POINT('',#36415);
#10716=VERTEX_POINT('',#36419);
#10717=VERTEX_POINT('',#36421);
#10718=VERTEX_POINT('',#36425);
#10719=VERTEX_POINT('',#36427);
#10720=VERTEX_POINT('',#36431);
#10721=VERTEX_POINT('',#36433);
#10722=VERTEX_POINT('',#36437);
#10723=VERTEX_POINT('',#36438);
#10724=VERTEX_POINT('',#36440);
#10725=VERTEX_POINT('',#36442);
#10726=VERTEX_POINT('',#36446);
#10727=VERTEX_POINT('',#36448);
#10728=VERTEX_POINT('',#36452);
#10729=VERTEX_POINT('',#36456);
#10730=VERTEX_POINT('',#36468);
#10731=VERTEX_POINT('',#36470);
#10732=VERTEX_POINT('',#36474);
#10733=VERTEX_POINT('',#36476);
#10734=VERTEX_POINT('',#36480);
#10735=VERTEX_POINT('',#36482);
#10736=VERTEX_POINT('',#36486);
#10737=VERTEX_POINT('',#36488);
#10738=VERTEX_POINT('',#36492);
#10739=VERTEX_POINT('',#36494);
#10740=VERTEX_POINT('',#36498);
#10741=VERTEX_POINT('',#36500);
#10742=VERTEX_POINT('',#36504);
#10743=VERTEX_POINT('',#36506);
#10744=VERTEX_POINT('',#36510);
#10745=VERTEX_POINT('',#36511);
#10746=VERTEX_POINT('',#36513);
#10747=VERTEX_POINT('',#36515);
#10748=VERTEX_POINT('',#36517);
#10749=VERTEX_POINT('',#36519);
#10750=VERTEX_POINT('',#36523);
#10751=VERTEX_POINT('',#36524);
#10752=VERTEX_POINT('',#36529);
#10753=VERTEX_POINT('',#36530);
#10754=VERTEX_POINT('',#36533);
#10755=VERTEX_POINT('',#36535);
#10756=VERTEX_POINT('',#36549);
#10757=VERTEX_POINT('',#36551);
#10758=VERTEX_POINT('',#36555);
#10759=VERTEX_POINT('',#36557);
#10760=VERTEX_POINT('',#36561);
#10761=VERTEX_POINT('',#36563);
#10762=VERTEX_POINT('',#36567);
#10763=VERTEX_POINT('',#36569);
#10764=VERTEX_POINT('',#36573);
#10765=VERTEX_POINT('',#36575);
#10766=VERTEX_POINT('',#36579);
#10767=VERTEX_POINT('',#36581);
#10768=VERTEX_POINT('',#36585);
#10769=VERTEX_POINT('',#36586);
#10770=VERTEX_POINT('',#36588);
#10771=VERTEX_POINT('',#36590);
#10772=VERTEX_POINT('',#36594);
#10773=VERTEX_POINT('',#36596);
#10774=VERTEX_POINT('',#36600);
#10775=VERTEX_POINT('',#36602);
#10776=VERTEX_POINT('',#36614);
#10777=VERTEX_POINT('',#36616);
#10778=VERTEX_POINT('',#36620);
#10779=VERTEX_POINT('',#36622);
#10780=VERTEX_POINT('',#36626);
#10781=VERTEX_POINT('',#36628);
#10782=VERTEX_POINT('',#36632);
#10783=VERTEX_POINT('',#36634);
#10784=VERTEX_POINT('',#36638);
#10785=VERTEX_POINT('',#36640);
#10786=VERTEX_POINT('',#36644);
#10787=VERTEX_POINT('',#36646);
#10788=VERTEX_POINT('',#36650);
#10789=VERTEX_POINT('',#36651);
#10790=VERTEX_POINT('',#36653);
#10791=VERTEX_POINT('',#36655);
#10792=VERTEX_POINT('',#36659);
#10793=VERTEX_POINT('',#36661);
#10794=VERTEX_POINT('',#36665);
#10795=VERTEX_POINT('',#36667);
#10796=VERTEX_POINT('',#36678);
#10797=VERTEX_POINT('',#36680);
#10798=VERTEX_POINT('',#36684);
#10799=VERTEX_POINT('',#36685);
#10800=VERTEX_POINT('',#36687);
#10801=VERTEX_POINT('',#36689);
#10802=VERTEX_POINT('',#36691);
#10803=VERTEX_POINT('',#36693);
#10804=VERTEX_POINT('',#36695);
#10805=VERTEX_POINT('',#36698);
#10806=VERTEX_POINT('',#36700);
#10807=VERTEX_POINT('',#36702);
#10808=VERTEX_POINT('',#36706);
#10809=VERTEX_POINT('',#36708);
#10810=VERTEX_POINT('',#36712);
#10811=VERTEX_POINT('',#36713);
#10812=VERTEX_POINT('',#36715);
#10813=VERTEX_POINT('',#36717);
#10814=VERTEX_POINT('',#36719);
#10815=VERTEX_POINT('',#36721);
#10816=VERTEX_POINT('',#36723);
#10817=VERTEX_POINT('',#36726);
#10818=VERTEX_POINT('',#36728);
#10819=VERTEX_POINT('',#36730);
#10820=VERTEX_POINT('',#36734);
#10821=VERTEX_POINT('',#36736);
#10822=VERTEX_POINT('',#36740);
#10823=VERTEX_POINT('',#36741);
#10824=VERTEX_POINT('',#36743);
#10825=VERTEX_POINT('',#36745);
#10826=VERTEX_POINT('',#36747);
#10827=VERTEX_POINT('',#36749);
#10828=VERTEX_POINT('',#36751);
#10829=VERTEX_POINT('',#36754);
#10830=VERTEX_POINT('',#36756);
#10831=VERTEX_POINT('',#36758);
#10832=VERTEX_POINT('',#36762);
#10833=VERTEX_POINT('',#36764);
#10834=VERTEX_POINT('',#36768);
#10835=VERTEX_POINT('',#36769);
#10836=VERTEX_POINT('',#36771);
#10837=VERTEX_POINT('',#36773);
#10838=VERTEX_POINT('',#36775);
#10839=VERTEX_POINT('',#36777);
#10840=VERTEX_POINT('',#36779);
#10841=VERTEX_POINT('',#36782);
#10842=VERTEX_POINT('',#36784);
#10843=VERTEX_POINT('',#36786);
#10844=VERTEX_POINT('',#36790);
#10845=VERTEX_POINT('',#36792);
#10846=VERTEX_POINT('',#36796);
#10847=VERTEX_POINT('',#36797);
#10848=VERTEX_POINT('',#36799);
#10849=VERTEX_POINT('',#36801);
#10850=VERTEX_POINT('',#36803);
#10851=VERTEX_POINT('',#36805);
#10852=VERTEX_POINT('',#36807);
#10853=VERTEX_POINT('',#36810);
#10854=VERTEX_POINT('',#36812);
#10855=VERTEX_POINT('',#36814);
#10856=VERTEX_POINT('',#36818);
#10857=VERTEX_POINT('',#36820);
#10858=VERTEX_POINT('',#36824);
#10859=VERTEX_POINT('',#36825);
#10860=VERTEX_POINT('',#36827);
#10861=VERTEX_POINT('',#36829);
#10862=VERTEX_POINT('',#36831);
#10863=VERTEX_POINT('',#36833);
#10864=VERTEX_POINT('',#36835);
#10865=VERTEX_POINT('',#36838);
#10866=VERTEX_POINT('',#36840);
#10867=VERTEX_POINT('',#36842);
#10868=VERTEX_POINT('',#36846);
#10869=VERTEX_POINT('',#36848);
#10870=VERTEX_POINT('',#36852);
#10871=VERTEX_POINT('',#36853);
#10872=VERTEX_POINT('',#36855);
#10873=VERTEX_POINT('',#36857);
#10874=VERTEX_POINT('',#36859);
#10875=VERTEX_POINT('',#36861);
#10876=VERTEX_POINT('',#36863);
#10877=VERTEX_POINT('',#36866);
#10878=VERTEX_POINT('',#36868);
#10879=VERTEX_POINT('',#36870);
#10880=VERTEX_POINT('',#36874);
#10881=VERTEX_POINT('',#36876);
#10882=VERTEX_POINT('',#36880);
#10883=VERTEX_POINT('',#36881);
#10884=VERTEX_POINT('',#36883);
#10885=VERTEX_POINT('',#36885);
#10886=VERTEX_POINT('',#36887);
#10887=VERTEX_POINT('',#36889);
#10888=VERTEX_POINT('',#36891);
#10889=VERTEX_POINT('',#36894);
#10890=VERTEX_POINT('',#36896);
#10891=VERTEX_POINT('',#36898);
#10892=VERTEX_POINT('',#36902);
#10893=VERTEX_POINT('',#36904);
#10894=VERTEX_POINT('',#36908);
#10895=VERTEX_POINT('',#36909);
#10896=VERTEX_POINT('',#36911);
#10897=VERTEX_POINT('',#36913);
#10898=VERTEX_POINT('',#36915);
#10899=VERTEX_POINT('',#36917);
#10900=VERTEX_POINT('',#36919);
#10901=VERTEX_POINT('',#36922);
#10902=VERTEX_POINT('',#36924);
#10903=VERTEX_POINT('',#36926);
#10904=VERTEX_POINT('',#36930);
#10905=VERTEX_POINT('',#36932);
#10906=VERTEX_POINT('',#36936);
#10907=VERTEX_POINT('',#36937);
#10908=VERTEX_POINT('',#36939);
#10909=VERTEX_POINT('',#36941);
#10910=VERTEX_POINT('',#36943);
#10911=VERTEX_POINT('',#36945);
#10912=VERTEX_POINT('',#36947);
#10913=VERTEX_POINT('',#36950);
#10914=VERTEX_POINT('',#36952);
#10915=VERTEX_POINT('',#36954);
#10916=VERTEX_POINT('',#36958);
#10917=VERTEX_POINT('',#36960);
#10918=VERTEX_POINT('',#36964);
#10919=VERTEX_POINT('',#36965);
#10920=VERTEX_POINT('',#36967);
#10921=VERTEX_POINT('',#36969);
#10922=VERTEX_POINT('',#36971);
#10923=VERTEX_POINT('',#36973);
#10924=VERTEX_POINT('',#36975);
#10925=VERTEX_POINT('',#36978);
#10926=VERTEX_POINT('',#36980);
#10927=VERTEX_POINT('',#36982);
#10928=VERTEX_POINT('',#36986);
#10929=VERTEX_POINT('',#36988);
#10930=VERTEX_POINT('',#36992);
#10931=VERTEX_POINT('',#36993);
#10932=VERTEX_POINT('',#36995);
#10933=VERTEX_POINT('',#36997);
#10934=VERTEX_POINT('',#36999);
#10935=VERTEX_POINT('',#37001);
#10936=VERTEX_POINT('',#37003);
#10937=VERTEX_POINT('',#37006);
#10938=VERTEX_POINT('',#37008);
#10939=VERTEX_POINT('',#37010);
#10940=VERTEX_POINT('',#37014);
#10941=VERTEX_POINT('',#37016);
#10942=VERTEX_POINT('',#37020);
#10943=VERTEX_POINT('',#37021);
#10944=VERTEX_POINT('',#37023);
#10945=VERTEX_POINT('',#37025);
#10946=VERTEX_POINT('',#37027);
#10947=VERTEX_POINT('',#37029);
#10948=VERTEX_POINT('',#37031);
#10949=VERTEX_POINT('',#37034);
#10950=VERTEX_POINT('',#37036);
#10951=VERTEX_POINT('',#37038);
#10952=VERTEX_POINT('',#37042);
#10953=VERTEX_POINT('',#37044);
#10954=VERTEX_POINT('',#37048);
#10955=VERTEX_POINT('',#37049);
#10956=VERTEX_POINT('',#37051);
#10957=VERTEX_POINT('',#37053);
#10958=VERTEX_POINT('',#37055);
#10959=VERTEX_POINT('',#37057);
#10960=VERTEX_POINT('',#37059);
#10961=VERTEX_POINT('',#37062);
#10962=VERTEX_POINT('',#37064);
#10963=VERTEX_POINT('',#37066);
#10964=VERTEX_POINT('',#37070);
#10965=VERTEX_POINT('',#37072);
#10966=VERTEX_POINT('',#37076);
#10967=VERTEX_POINT('',#37077);
#10968=VERTEX_POINT('',#37079);
#10969=VERTEX_POINT('',#37081);
#10970=VERTEX_POINT('',#37083);
#10971=VERTEX_POINT('',#37085);
#10972=VERTEX_POINT('',#37087);
#10973=VERTEX_POINT('',#37090);
#10974=VERTEX_POINT('',#37092);
#10975=VERTEX_POINT('',#37094);
#10976=VERTEX_POINT('',#37098);
#10977=VERTEX_POINT('',#37100);
#10978=VERTEX_POINT('',#37121);
#10979=VERTEX_POINT('',#37123);
#10980=VERTEX_POINT('',#37125);
#10981=VERTEX_POINT('',#37131);
#10982=VERTEX_POINT('',#37133);
#10983=VERTEX_POINT('',#37135);
#10984=VERTEX_POINT('',#37137);
#10985=VERTEX_POINT('',#37219);
#10986=VERTEX_POINT('',#37221);
#10987=VERTEX_POINT('',#37228);
#10988=VERTEX_POINT('',#37230);
#10989=VERTEX_POINT('',#37232);
#10990=VERTEX_POINT('',#37234);
#10991=VERTEX_POINT('',#37236);
#10992=VERTEX_POINT('',#37238);
#10993=VERTEX_POINT('',#37240);
#10994=VERTEX_POINT('',#37242);
#10995=VERTEX_POINT('',#37244);
#10996=VERTEX_POINT('',#37246);
#10997=VERTEX_POINT('',#37248);
#10998=VERTEX_POINT('',#37250);
#10999=VERTEX_POINT('',#37252);
#11000=VERTEX_POINT('',#37254);
#11001=VERTEX_POINT('',#37256);
#11002=VERTEX_POINT('',#37258);
#11003=VERTEX_POINT('',#37260);
#11004=VERTEX_POINT('',#37262);
#11005=VERTEX_POINT('',#37264);
#11006=VERTEX_POINT('',#37266);
#11007=VERTEX_POINT('',#37268);
#11008=VERTEX_POINT('',#37270);
#11009=VERTEX_POINT('',#37272);
#11010=VERTEX_POINT('',#37274);
#11011=VERTEX_POINT('',#37276);
#11012=VERTEX_POINT('',#37278);
#11013=VERTEX_POINT('',#37280);
#11014=VERTEX_POINT('',#37282);
#11015=VERTEX_POINT('',#37284);
#11016=VERTEX_POINT('',#37286);
#11017=VERTEX_POINT('',#37288);
#11018=VERTEX_POINT('',#37290);
#11019=VERTEX_POINT('',#37292);
#11020=VERTEX_POINT('',#37294);
#11021=VERTEX_POINT('',#37296);
#11022=VERTEX_POINT('',#37298);
#11023=VERTEX_POINT('',#37300);
#11024=VERTEX_POINT('',#37302);
#11025=VERTEX_POINT('',#37304);
#11026=VERTEX_POINT('',#37306);
#11027=VERTEX_POINT('',#37309);
#11028=VERTEX_POINT('',#37314);
#11029=VERTEX_POINT('',#37316);
#11030=VERTEX_POINT('',#37318);
#11031=VERTEX_POINT('',#37320);
#11032=VERTEX_POINT('',#37322);
#11033=VERTEX_POINT('',#37324);
#11034=VERTEX_POINT('',#37326);
#11035=VERTEX_POINT('',#37328);
#11036=VERTEX_POINT('',#37330);
#11037=VERTEX_POINT('',#37332);
#11038=VERTEX_POINT('',#37334);
#11039=VERTEX_POINT('',#37336);
#11040=VERTEX_POINT('',#37338);
#11041=VERTEX_POINT('',#37340);
#11042=VERTEX_POINT('',#37342);
#11043=VERTEX_POINT('',#37344);
#11044=VERTEX_POINT('',#37346);
#11045=VERTEX_POINT('',#37348);
#11046=VERTEX_POINT('',#37350);
#11047=VERTEX_POINT('',#37352);
#11048=VERTEX_POINT('',#37354);
#11049=VERTEX_POINT('',#37356);
#11050=VERTEX_POINT('',#37358);
#11051=VERTEX_POINT('',#37360);
#11052=VERTEX_POINT('',#37362);
#11053=VERTEX_POINT('',#37364);
#11054=VERTEX_POINT('',#37366);
#11055=VERTEX_POINT('',#37368);
#11056=VERTEX_POINT('',#37370);
#11057=VERTEX_POINT('',#37372);
#11058=VERTEX_POINT('',#37374);
#11059=VERTEX_POINT('',#37376);
#11060=VERTEX_POINT('',#37378);
#11061=VERTEX_POINT('',#37380);
#11062=VERTEX_POINT('',#37382);
#11063=VERTEX_POINT('',#37384);
#11064=VERTEX_POINT('',#37386);
#11065=VERTEX_POINT('',#37388);
#11066=VERTEX_POINT('',#37390);
#11067=VERTEX_POINT('',#37392);
#11068=VERTEX_POINT('',#37497);
#11069=VERTEX_POINT('',#37499);
#11070=VERTEX_POINT('',#37503);
#11071=VERTEX_POINT('',#37505);
#11072=VERTEX_POINT('',#37509);
#11073=VERTEX_POINT('',#37511);
#11074=VERTEX_POINT('',#37515);
#11075=VERTEX_POINT('',#37518);
#11076=VERTEX_POINT('',#37521);
#11077=VERTEX_POINT('',#37523);
#11078=VERTEX_POINT('',#37527);
#11079=VERTEX_POINT('',#37529);
#11080=VERTEX_POINT('',#37533);
#11081=VERTEX_POINT('',#37535);
#11082=VERTEX_POINT('',#37539);
#11083=VERTEX_POINT('',#37541);
#11084=VERTEX_POINT('',#37545);
#11085=VERTEX_POINT('',#37547);
#11086=VERTEX_POINT('',#37551);
#11087=VERTEX_POINT('',#37553);
#11088=VERTEX_POINT('',#37557);
#11089=VERTEX_POINT('',#37559);
#11090=VERTEX_POINT('',#37563);
#11091=VERTEX_POINT('',#37565);
#11092=VERTEX_POINT('',#37567);
#11093=VERTEX_POINT('',#37569);
#11094=VERTEX_POINT('',#37571);
#11095=VERTEX_POINT('',#37575);
#11096=VERTEX_POINT('',#37578);
#11097=VERTEX_POINT('',#37581);
#11098=VERTEX_POINT('',#37583);
#11099=VERTEX_POINT('',#37585);
#11100=VERTEX_POINT('',#37587);
#11101=VERTEX_POINT('',#37589);
#11102=VERTEX_POINT('',#37619);
#11103=VERTEX_POINT('',#37620);
#11104=VERTEX_POINT('',#37631);
#11105=VERTEX_POINT('',#37642);
#11106=VERTEX_POINT('',#37653);
#11107=VERTEX_POINT('',#37657);
#11108=VERTEX_POINT('',#37660);
#11109=VERTEX_POINT('',#37671);
#11110=VERTEX_POINT('',#37693);
#11111=VERTEX_POINT('',#37697);
#11112=VERTEX_POINT('',#37699);
#11113=VERTEX_POINT('',#37703);
#11114=VERTEX_POINT('',#37704);
#11115=VERTEX_POINT('',#37706);
#11116=VERTEX_POINT('',#37708);
#11117=VERTEX_POINT('',#37712);
#11118=VERTEX_POINT('',#37714);
#11119=VERTEX_POINT('',#37716);
#11120=VERTEX_POINT('',#37720);
#11121=VERTEX_POINT('',#37721);
#11122=VERTEX_POINT('',#37723);
#11123=VERTEX_POINT('',#37725);
#11124=VERTEX_POINT('',#37729);
#11125=VERTEX_POINT('',#37731);
#11126=VERTEX_POINT('',#37733);
#11127=VERTEX_POINT('',#37737);
#11128=VERTEX_POINT('',#37738);
#11129=VERTEX_POINT('',#37740);
#11130=VERTEX_POINT('',#37742);
#11131=VERTEX_POINT('',#37746);
#11132=VERTEX_POINT('',#37747);
#11133=VERTEX_POINT('',#37749);
#11134=VERTEX_POINT('',#37751);
#11135=VERTEX_POINT('',#37755);
#11136=VERTEX_POINT('',#37756);
#11137=VERTEX_POINT('',#37758);
#11138=VERTEX_POINT('',#37760);
#11139=VERTEX_POINT('',#37764);
#11140=VERTEX_POINT('',#37765);
#11141=VERTEX_POINT('',#37767);
#11142=VERTEX_POINT('',#37769);
#11143=VERTEX_POINT('',#37773);
#11144=VERTEX_POINT('',#37774);
#11145=VERTEX_POINT('',#37776);
#11146=VERTEX_POINT('',#37778);
#11147=VERTEX_POINT('',#37782);
#11148=VERTEX_POINT('',#37783);
#11149=VERTEX_POINT('',#37785);
#11150=VERTEX_POINT('',#37787);
#11151=VERTEX_POINT('',#37791);
#11152=VERTEX_POINT('',#37792);
#11153=VERTEX_POINT('',#37794);
#11154=VERTEX_POINT('',#37796);
#11155=VERTEX_POINT('',#37800);
#11156=VERTEX_POINT('',#37801);
#11157=VERTEX_POINT('',#37803);
#11158=VERTEX_POINT('',#37805);
#11159=VERTEX_POINT('',#37809);
#11160=VERTEX_POINT('',#37810);
#11161=VERTEX_POINT('',#37812);
#11162=VERTEX_POINT('',#37814);
#11163=VERTEX_POINT('',#37818);
#11164=VERTEX_POINT('',#37820);
#11165=VERTEX_POINT('',#37824);
#11166=VERTEX_POINT('',#37825);
#11167=VERTEX_POINT('',#37827);
#11168=VERTEX_POINT('',#37829);
#11169=VERTEX_POINT('',#37833);
#11170=VERTEX_POINT('',#37835);
#11171=VERTEX_POINT('',#37839);
#11172=VERTEX_POINT('',#37840);
#11173=VERTEX_POINT('',#37842);
#11174=VERTEX_POINT('',#37844);
#11175=VERTEX_POINT('',#37848);
#11176=VERTEX_POINT('',#37849);
#11177=VERTEX_POINT('',#37851);
#11178=VERTEX_POINT('',#37853);
#11179=VERTEX_POINT('',#37857);
#11180=VERTEX_POINT('',#37858);
#11181=VERTEX_POINT('',#37860);
#11182=VERTEX_POINT('',#37862);
#11183=VERTEX_POINT('',#37866);
#11184=VERTEX_POINT('',#37867);
#11185=VERTEX_POINT('',#37869);
#11186=VERTEX_POINT('',#37871);
#11187=VERTEX_POINT('',#37878);
#11188=VERTEX_POINT('',#37879);
#11189=VERTEX_POINT('',#37881);
#11190=VERTEX_POINT('',#37883);
#11191=VERTEX_POINT('',#37887);
#11192=VERTEX_POINT('',#37888);
#11193=VERTEX_POINT('',#37890);
#11194=VERTEX_POINT('',#37892);
#11195=VERTEX_POINT('',#37896);
#11196=VERTEX_POINT('',#37897);
#11197=VERTEX_POINT('',#37899);
#11198=VERTEX_POINT('',#37901);
#11199=VERTEX_POINT('',#37905);
#11200=VERTEX_POINT('',#37906);
#11201=VERTEX_POINT('',#37908);
#11202=VERTEX_POINT('',#37910);
#11203=VERTEX_POINT('',#37963);
#11204=VERTEX_POINT('',#37964);
#11205=VERTEX_POINT('',#37966);
#11206=VERTEX_POINT('',#37968);
#11207=VERTEX_POINT('',#37972);
#11208=VERTEX_POINT('',#37974);
#11209=VERTEX_POINT('',#37977);
#11210=VERTEX_POINT('',#37979);
#11211=VERTEX_POINT('',#37983);
#11212=VERTEX_POINT('',#37987);
#11213=VERTEX_POINT('',#37993);
#11214=VERTEX_POINT('',#37997);
#11215=VERTEX_POINT('',#38003);
#11216=VERTEX_POINT('',#38005);
#11217=VERTEX_POINT('',#38009);
#11218=VERTEX_POINT('',#38013);
#11219=VERTEX_POINT('',#38017);
#11220=VERTEX_POINT('',#38021);
#11221=VERTEX_POINT('',#38028);
#11222=VERTEX_POINT('',#38029);
#11223=VERTEX_POINT('',#38031);
#11224=VERTEX_POINT('',#38033);
#11225=VERTEX_POINT('',#38035);
#11226=VERTEX_POINT('',#38037);
#11227=VERTEX_POINT('',#38039);
#11228=VERTEX_POINT('',#38041);
#11229=VERTEX_POINT('',#38043);
#11230=VERTEX_POINT('',#38045);
#11231=VERTEX_POINT('',#38047);
#11232=VERTEX_POINT('',#38049);
#11233=VERTEX_POINT('',#38051);
#11234=VERTEX_POINT('',#38053);
#11235=VERTEX_POINT('',#38055);
#11236=VERTEX_POINT('',#38057);
#11237=VERTEX_POINT('',#38059);
#11238=VERTEX_POINT('',#38061);
#11239=VERTEX_POINT('',#38063);
#11240=VERTEX_POINT('',#38065);
#11241=VERTEX_POINT('',#38067);
#11242=VERTEX_POINT('',#38069);
#11243=VERTEX_POINT('',#38071);
#11244=VERTEX_POINT('',#38073);
#11245=VERTEX_POINT('',#38075);
#11246=VERTEX_POINT('',#38077);
#11247=VERTEX_POINT('',#38079);
#11248=VERTEX_POINT('',#38081);
#11249=VERTEX_POINT('',#38083);
#11250=VERTEX_POINT('',#38085);
#11251=VERTEX_POINT('',#38087);
#11252=VERTEX_POINT('',#38089);
#11253=VERTEX_POINT('',#38091);
#11254=VERTEX_POINT('',#38093);
#11255=VERTEX_POINT('',#38095);
#11256=VERTEX_POINT('',#38097);
#11257=VERTEX_POINT('',#38099);
#11258=VERTEX_POINT('',#38101);
#11259=VERTEX_POINT('',#38103);
#11260=VERTEX_POINT('',#38105);
#11261=VERTEX_POINT('',#38107);
#11262=VERTEX_POINT('',#38109);
#11263=VERTEX_POINT('',#38111);
#11264=VERTEX_POINT('',#38113);
#11265=VERTEX_POINT('',#38117);
#11266=VERTEX_POINT('',#38118);
#11267=VERTEX_POINT('',#38123);
#11268=VERTEX_POINT('',#38127);
#11269=VERTEX_POINT('',#38131);
#11270=VERTEX_POINT('',#38135);
#11271=VERTEX_POINT('',#38139);
#11272=VERTEX_POINT('',#38143);
#11273=VERTEX_POINT('',#38147);
#11274=VERTEX_POINT('',#38151);
#11275=VERTEX_POINT('',#38155);
#11276=VERTEX_POINT('',#38159);
#11277=VERTEX_POINT('',#38163);
#11278=VERTEX_POINT('',#38167);
#11279=VERTEX_POINT('',#38171);
#11280=VERTEX_POINT('',#38175);
#11281=VERTEX_POINT('',#38179);
#11282=VERTEX_POINT('',#38183);
#11283=VERTEX_POINT('',#38187);
#11284=VERTEX_POINT('',#38191);
#11285=VERTEX_POINT('',#38195);
#11286=VERTEX_POINT('',#38199);
#11287=VERTEX_POINT('',#38203);
#11288=VERTEX_POINT('',#38207);
#11289=VERTEX_POINT('',#38211);
#11290=VERTEX_POINT('',#38215);
#11291=VERTEX_POINT('',#38219);
#11292=VERTEX_POINT('',#38223);
#11293=VERTEX_POINT('',#38227);
#11294=VERTEX_POINT('',#38231);
#11295=VERTEX_POINT('',#38235);
#11296=VERTEX_POINT('',#38239);
#11297=VERTEX_POINT('',#38243);
#11298=VERTEX_POINT('',#38247);
#11299=VERTEX_POINT('',#38251);
#11300=VERTEX_POINT('',#38255);
#11301=VERTEX_POINT('',#38259);
#11302=VERTEX_POINT('',#38263);
#11303=VERTEX_POINT('',#38267);
#11304=VERTEX_POINT('',#38271);
#11305=VERTEX_POINT('',#38275);
#11306=VERTEX_POINT('',#38279);
#11307=VERTEX_POINT('',#38283);
#11308=VERTEX_POINT('',#38287);
#11309=VERTEX_POINT('',#38294);
#11310=VERTEX_POINT('',#38296);
#11311=VERTEX_POINT('',#38300);
#11312=VERTEX_POINT('',#38301);
#11313=VERTEX_POINT('',#38303);
#11314=VERTEX_POINT('',#38305);
#11315=VERTEX_POINT('',#38307);
#11316=VERTEX_POINT('',#38309);
#11317=VERTEX_POINT('',#38311);
#11318=VERTEX_POINT('',#38313);
#11319=VERTEX_POINT('',#38315);
#11320=VERTEX_POINT('',#38317);
#11321=VERTEX_POINT('',#38319);
#11322=VERTEX_POINT('',#38321);
#11323=VERTEX_POINT('',#38323);
#11324=VERTEX_POINT('',#38325);
#11325=VERTEX_POINT('',#38327);
#11326=VERTEX_POINT('',#38329);
#11327=VERTEX_POINT('',#38331);
#11328=VERTEX_POINT('',#38333);
#11329=VERTEX_POINT('',#38335);
#11330=VERTEX_POINT('',#38337);
#11331=VERTEX_POINT('',#38339);
#11332=VERTEX_POINT('',#38341);
#11333=VERTEX_POINT('',#38343);
#11334=VERTEX_POINT('',#38345);
#11335=VERTEX_POINT('',#38347);
#11336=VERTEX_POINT('',#38349);
#11337=VERTEX_POINT('',#38351);
#11338=VERTEX_POINT('',#38353);
#11339=VERTEX_POINT('',#38355);
#11340=VERTEX_POINT('',#38357);
#11341=VERTEX_POINT('',#38359);
#11342=VERTEX_POINT('',#38361);
#11343=VERTEX_POINT('',#38363);
#11344=VERTEX_POINT('',#38365);
#11345=VERTEX_POINT('',#38367);
#11346=VERTEX_POINT('',#38369);
#11347=VERTEX_POINT('',#38371);
#11348=VERTEX_POINT('',#38373);
#11349=VERTEX_POINT('',#38375);
#11350=VERTEX_POINT('',#38377);
#11351=VERTEX_POINT('',#38379);
#11352=VERTEX_POINT('',#38381);
#11353=VERTEX_POINT('',#38383);
#11354=VERTEX_POINT('',#38385);
#11355=VERTEX_POINT('',#38387);
#11356=VERTEX_POINT('',#38389);
#11357=VERTEX_POINT('',#38391);
#11358=VERTEX_POINT('',#38393);
#11359=VERTEX_POINT('',#38397);
#11360=VERTEX_POINT('',#38401);
#11361=VERTEX_POINT('',#38408);
#11362=VERTEX_POINT('',#38410);
#11363=VERTEX_POINT('',#38414);
#11364=VERTEX_POINT('',#38415);
#11365=VERTEX_POINT('',#38420);
#11366=VERTEX_POINT('',#38424);
#11367=VERTEX_POINT('',#38428);
#11368=VERTEX_POINT('',#38432);
#11369=VERTEX_POINT('',#38433);
#11370=VERTEX_POINT('',#38436);
#11371=VERTEX_POINT('',#38441);
#11372=VERTEX_POINT('',#38445);
#11373=VERTEX_POINT('',#38449);
#11374=VERTEX_POINT('',#38453);
#11375=VERTEX_POINT('',#38457);
#11376=VERTEX_POINT('',#38461);
#11377=VERTEX_POINT('',#38465);
#11378=VERTEX_POINT('',#38469);
#11379=VERTEX_POINT('',#38473);
#11380=VERTEX_POINT('',#38477);
#11381=VERTEX_POINT('',#38481);
#11382=VERTEX_POINT('',#38485);
#11383=VERTEX_POINT('',#38489);
#11384=VERTEX_POINT('',#38493);
#11385=VERTEX_POINT('',#38497);
#11386=VERTEX_POINT('',#38501);
#11387=VERTEX_POINT('',#38505);
#11388=VERTEX_POINT('',#38509);
#11389=VERTEX_POINT('',#38513);
#11390=VERTEX_POINT('',#38517);
#11391=VERTEX_POINT('',#38521);
#11392=VERTEX_POINT('',#38525);
#11393=VERTEX_POINT('',#38529);
#11394=VERTEX_POINT('',#38533);
#11395=VERTEX_POINT('',#38537);
#11396=VERTEX_POINT('',#38541);
#11397=VERTEX_POINT('',#38545);
#11398=VERTEX_POINT('',#38549);
#11399=VERTEX_POINT('',#38553);
#11400=VERTEX_POINT('',#38557);
#11401=VERTEX_POINT('',#38561);
#11402=VERTEX_POINT('',#38565);
#11403=VERTEX_POINT('',#38569);
#11404=VERTEX_POINT('',#38573);
#11405=VERTEX_POINT('',#38577);
#11406=VERTEX_POINT('',#38581);
#11407=VERTEX_POINT('',#38585);
#11408=VERTEX_POINT('',#38589);
#11409=VERTEX_POINT('',#38596);
#11410=VERTEX_POINT('',#38597);
#11411=VERTEX_POINT('',#38599);
#11412=VERTEX_POINT('',#38601);
#11413=VERTEX_POINT('',#38605);
#11414=VERTEX_POINT('',#38606);
#11415=VERTEX_POINT('',#38608);
#11416=VERTEX_POINT('',#38610);
#11417=VERTEX_POINT('',#38614);
#11418=VERTEX_POINT('',#38618);
#11419=VERTEX_POINT('',#38624);
#11420=VERTEX_POINT('',#38626);
#11421=VERTEX_POINT('',#38630);
#11422=VERTEX_POINT('',#38632);
#11423=VERTEX_POINT('',#38634);
#11424=VERTEX_POINT('',#38638);
#11425=VERTEX_POINT('',#38640);
#11426=VERTEX_POINT('',#38644);
#11427=VERTEX_POINT('',#38645);
#11428=VERTEX_POINT('',#38647);
#11429=VERTEX_POINT('',#38649);
#11430=VERTEX_POINT('',#38653);
#11431=VERTEX_POINT('',#38656);
#11432=VERTEX_POINT('',#38660);
#11433=VERTEX_POINT('',#38664);
#11434=VERTEX_POINT('',#38665);
#11435=VERTEX_POINT('',#38667);
#11436=VERTEX_POINT('',#38669);
#11437=VERTEX_POINT('',#38671);
#11438=VERTEX_POINT('',#38673);
#11439=VERTEX_POINT('',#38675);
#11440=VERTEX_POINT('',#38677);
#11441=VERTEX_POINT('',#38679);
#11442=VERTEX_POINT('',#38681);
#11443=VERTEX_POINT('',#38683);
#11444=VERTEX_POINT('',#38685);
#11445=VERTEX_POINT('',#38687);
#11446=VERTEX_POINT('',#38689);
#11447=VERTEX_POINT('',#38691);
#11448=VERTEX_POINT('',#38693);
#11449=VERTEX_POINT('',#38695);
#11450=VERTEX_POINT('',#38697);
#11451=VERTEX_POINT('',#38699);
#11452=VERTEX_POINT('',#38701);
#11453=VERTEX_POINT('',#38703);
#11454=VERTEX_POINT('',#38705);
#11455=VERTEX_POINT('',#38707);
#11456=VERTEX_POINT('',#38709);
#11457=VERTEX_POINT('',#38711);
#11458=VERTEX_POINT('',#38713);
#11459=VERTEX_POINT('',#38715);
#11460=VERTEX_POINT('',#38717);
#11461=VERTEX_POINT('',#38719);
#11462=VERTEX_POINT('',#38721);
#11463=VERTEX_POINT('',#38723);
#11464=VERTEX_POINT('',#38725);
#11465=VERTEX_POINT('',#38727);
#11466=VERTEX_POINT('',#38729);
#11467=VERTEX_POINT('',#38731);
#11468=VERTEX_POINT('',#38733);
#11469=VERTEX_POINT('',#38735);
#11470=VERTEX_POINT('',#38737);
#11471=VERTEX_POINT('',#38739);
#11472=VERTEX_POINT('',#38741);
#11473=VERTEX_POINT('',#38743);
#11474=VERTEX_POINT('',#38745);
#11475=VERTEX_POINT('',#38747);
#11476=VERTEX_POINT('',#38749);
#11477=VERTEX_POINT('',#38753);
#11478=VERTEX_POINT('',#38757);
#11479=VERTEX_POINT('',#38761);
#11480=VERTEX_POINT('',#38762);
#11481=VERTEX_POINT('',#38767);
#11482=VERTEX_POINT('',#38769);
#11483=VERTEX_POINT('',#38773);
#11484=VERTEX_POINT('',#38775);
#11485=VERTEX_POINT('',#38779);
#11486=VERTEX_POINT('',#38781);
#11487=VERTEX_POINT('',#38789);
#11488=VERTEX_POINT('',#38791);
#11489=VERTEX_POINT('',#38793);
#11490=VERTEX_POINT('',#38797);
#11491=VERTEX_POINT('',#38798);
#11492=VERTEX_POINT('',#38803);
#11493=VERTEX_POINT('',#38805);
#11494=VERTEX_POINT('',#38809);
#11495=VERTEX_POINT('',#38810);
#11496=VERTEX_POINT('',#38815);
#11497=VERTEX_POINT('',#38820);
#11498=VERTEX_POINT('',#38822);
#11499=VERTEX_POINT('',#38829);
#11500=VERTEX_POINT('',#38830);
#11501=VERTEX_POINT('',#38835);
#11502=VERTEX_POINT('',#38839);
#11503=VERTEX_POINT('',#38843);
#11504=VERTEX_POINT('',#38847);
#11505=VERTEX_POINT('',#38851);
#11506=VERTEX_POINT('',#38855);
#11507=VERTEX_POINT('',#38859);
#11508=VERTEX_POINT('',#38863);
#11509=VERTEX_POINT('',#38867);
#11510=VERTEX_POINT('',#38871);
#11511=VERTEX_POINT('',#38875);
#11512=VERTEX_POINT('',#38879);
#11513=VERTEX_POINT('',#38883);
#11514=VERTEX_POINT('',#38887);
#11515=VERTEX_POINT('',#38891);
#11516=VERTEX_POINT('',#38895);
#11517=VERTEX_POINT('',#38899);
#11518=VERTEX_POINT('',#38903);
#11519=VERTEX_POINT('',#38907);
#11520=VERTEX_POINT('',#38911);
#11521=VERTEX_POINT('',#38915);
#11522=VERTEX_POINT('',#38919);
#11523=VERTEX_POINT('',#38923);
#11524=VERTEX_POINT('',#38927);
#11525=VERTEX_POINT('',#38931);
#11526=VERTEX_POINT('',#38935);
#11527=VERTEX_POINT('',#38939);
#11528=VERTEX_POINT('',#38943);
#11529=VERTEX_POINT('',#38947);
#11530=VERTEX_POINT('',#38951);
#11531=VERTEX_POINT('',#38955);
#11532=VERTEX_POINT('',#38959);
#11533=VERTEX_POINT('',#38963);
#11534=VERTEX_POINT('',#38967);
#11535=VERTEX_POINT('',#38971);
#11536=VERTEX_POINT('',#38975);
#11537=VERTEX_POINT('',#38979);
#11538=VERTEX_POINT('',#38983);
#11539=VERTEX_POINT('',#38987);
#11540=VERTEX_POINT('',#38991);
#11541=VERTEX_POINT('',#38995);
#11542=VERTEX_POINT('',#38999);
#11543=VERTEX_POINT('',#39005);
#11544=VERTEX_POINT('',#39006);
#11545=VERTEX_POINT('',#39008);
#11546=VERTEX_POINT('',#39010);
#11547=VERTEX_POINT('',#39014);
#11548=VERTEX_POINT('',#39016);
#11549=VERTEX_POINT('',#39020);
#11550=VERTEX_POINT('',#39022);
#11551=VERTEX_POINT('',#39026);
#11552=VERTEX_POINT('',#39028);
#11553=VERTEX_POINT('',#39032);
#11554=VERTEX_POINT('',#39034);
#11555=VERTEX_POINT('',#39038);
#11556=VERTEX_POINT('',#39039);
#11557=VERTEX_POINT('',#39041);
#11558=VERTEX_POINT('',#39043);
#11559=VERTEX_POINT('',#39047);
#11560=VERTEX_POINT('',#39049);
#11561=VERTEX_POINT('',#39053);
#11562=VERTEX_POINT('',#39055);
#11563=VERTEX_POINT('',#39062);
#11564=VERTEX_POINT('',#39064);
#11565=VERTEX_POINT('',#39066);
#11566=VERTEX_POINT('',#39070);
#11567=VERTEX_POINT('',#39072);
#11568=VERTEX_POINT('',#39076);
#11569=VERTEX_POINT('',#39077);
#11570=VERTEX_POINT('',#39082);
#11571=VERTEX_POINT('',#39083);
#11572=VERTEX_POINT('',#39088);
#11573=VERTEX_POINT('',#39089);
#11574=VERTEX_POINT('',#39094);
#11575=VERTEX_POINT('',#39095);
#11576=VERTEX_POINT('',#39100);
#11577=VERTEX_POINT('',#39102);
#11578=VERTEX_POINT('',#39106);
#11579=VERTEX_POINT('',#39107);
#11580=VERTEX_POINT('',#39112);
#11581=VERTEX_POINT('',#39113);
#11582=VERTEX_POINT('',#39118);
#11583=VERTEX_POINT('',#39119);
#11584=VERTEX_POINT('',#39124);
#11585=VERTEX_POINT('',#39126);
#11586=VERTEX_POINT('',#39130);
#11587=VERTEX_POINT('',#39132);
#11588=VERTEX_POINT('',#39136);
#11589=VERTEX_POINT('',#39138);
#11590=VERTEX_POINT('',#39142);
#11591=VERTEX_POINT('',#39144);
#11592=VERTEX_POINT('',#39148);
#11593=VERTEX_POINT('',#39153);
#11594=VERTEX_POINT('',#39155);
#11595=VERTEX_POINT('',#39159);
#11596=VERTEX_POINT('',#39160);
#11597=VERTEX_POINT('',#39165);
#11598=VERTEX_POINT('',#39167);
#11599=VERTEX_POINT('',#39171);
#11600=VERTEX_POINT('',#39173);
#11601=VERTEX_POINT('',#39177);
#11602=VERTEX_POINT('',#39178);
#11603=VERTEX_POINT('',#39187);
#11604=VERTEX_POINT('',#39191);
#11605=VERTEX_POINT('',#39193);
#11606=VERTEX_POINT('',#39197);
#11607=VERTEX_POINT('',#39199);
#11608=VERTEX_POINT('',#39204);
#11609=VERTEX_POINT('',#39211);
#11610=VERTEX_POINT('',#39213);
#11611=VERTEX_POINT('',#39215);
#11612=VERTEX_POINT('',#39217);
#11613=VERTEX_POINT('',#39219);
#11614=VERTEX_POINT('',#39221);
#11615=VERTEX_POINT('',#39223);
#11616=VERTEX_POINT('',#39225);
#11617=VERTEX_POINT('',#39227);
#11618=VERTEX_POINT('',#39229);
#11619=VERTEX_POINT('',#39231);
#11620=VERTEX_POINT('',#39233);
#11621=VERTEX_POINT('',#39235);
#11622=VERTEX_POINT('',#39237);
#11623=VERTEX_POINT('',#39239);
#11624=VERTEX_POINT('',#39241);
#11625=VERTEX_POINT('',#39243);
#11626=VERTEX_POINT('',#39245);
#11627=VERTEX_POINT('',#39247);
#11628=VERTEX_POINT('',#39249);
#11629=VERTEX_POINT('',#39251);
#11630=VERTEX_POINT('',#39253);
#11631=VERTEX_POINT('',#39255);
#11632=VERTEX_POINT('',#39257);
#11633=VERTEX_POINT('',#39259);
#11634=VERTEX_POINT('',#39261);
#11635=VERTEX_POINT('',#39263);
#11636=VERTEX_POINT('',#39265);
#11637=VERTEX_POINT('',#39267);
#11638=VERTEX_POINT('',#39269);
#11639=VERTEX_POINT('',#39271);
#11640=VERTEX_POINT('',#39273);
#11641=VERTEX_POINT('',#39275);
#11642=VERTEX_POINT('',#39277);
#11643=VERTEX_POINT('',#39279);
#11644=VERTEX_POINT('',#39281);
#11645=VERTEX_POINT('',#39285);
#11646=VERTEX_POINT('',#39287);
#11647=VERTEX_POINT('',#39289);
#11648=VERTEX_POINT('',#39291);
#11649=VERTEX_POINT('',#39293);
#11650=VERTEX_POINT('',#39295);
#11651=VERTEX_POINT('',#39297);
#11652=VERTEX_POINT('',#39299);
#11653=VERTEX_POINT('',#39301);
#11654=VERTEX_POINT('',#39303);
#11655=VERTEX_POINT('',#39305);
#11656=VERTEX_POINT('',#39307);
#11657=VERTEX_POINT('',#39311);
#11658=VERTEX_POINT('',#39312);
#11659=VERTEX_POINT('',#39317);
#11660=VERTEX_POINT('',#39318);
#11661=VERTEX_POINT('',#39323);
#11662=VERTEX_POINT('',#39327);
#11663=VERTEX_POINT('',#39331);
#11664=VERTEX_POINT('',#39335);
#11665=VERTEX_POINT('',#39337);
#11666=VERTEX_POINT('',#39341);
#11667=VERTEX_POINT('',#39343);
#11668=VERTEX_POINT('',#39349);
#11669=VERTEX_POINT('',#39355);
#11670=VERTEX_POINT('',#39356);
#11671=VERTEX_POINT('',#39361);
#11672=VERTEX_POINT('',#39362);
#11673=VERTEX_POINT('',#39369);
#11674=VERTEX_POINT('',#39370);
#11675=VERTEX_POINT('',#39375);
#11676=VERTEX_POINT('',#39376);
#11677=VERTEX_POINT('',#39385);
#11678=VERTEX_POINT('',#39386);
#11679=VERTEX_POINT('',#39391);
#11680=VERTEX_POINT('',#39392);
#11681=VERTEX_POINT('',#39399);
#11682=VERTEX_POINT('',#39401);
#11683=VERTEX_POINT('',#39407);
#11684=VERTEX_POINT('',#39408);
#11685=VERTEX_POINT('',#39413);
#11686=VERTEX_POINT('',#39414);
#11687=VERTEX_POINT('',#39421);
#11688=VERTEX_POINT('',#39422);
#11689=VERTEX_POINT('',#39427);
#11690=VERTEX_POINT('',#39428);
#11691=VERTEX_POINT('',#39439);
#11692=VERTEX_POINT('',#39440);
#11693=VERTEX_POINT('',#39445);
#11694=VERTEX_POINT('',#39446);
#11695=VERTEX_POINT('',#39453);
#11696=VERTEX_POINT('',#39455);
#11697=VERTEX_POINT('',#39459);
#11698=VERTEX_POINT('',#39461);
#11699=VERTEX_POINT('',#39465);
#11700=VERTEX_POINT('',#39466);
#11701=VERTEX_POINT('',#39471);
#11702=VERTEX_POINT('',#39475);
#11703=VERTEX_POINT('',#39481);
#11704=VERTEX_POINT('',#39497);
#11705=VERTEX_POINT('',#39504);
#11706=VERTEX_POINT('',#39508);
#11707=VERTEX_POINT('',#39520);
#11708=VERTEX_POINT('',#39522);
#11709=VERTEX_POINT('',#39552);
#11710=VERTEX_POINT('',#39556);
#11711=VERTEX_POINT('',#39560);
#11712=VERTEX_POINT('',#39563);
#11713=VERTEX_POINT('',#39564);
#11714=VERTEX_POINT('',#39566);
#11715=VERTEX_POINT('',#39574);
#11716=VERTEX_POINT('',#39575);
#11717=VERTEX_POINT('',#39577);
#11718=VERTEX_POINT('',#39585);
#11719=VERTEX_POINT('',#39586);
#11720=VERTEX_POINT('',#39588);
#11721=VERTEX_POINT('',#39599);
#11722=VERTEX_POINT('',#39613);
#11723=VERTEX_POINT('',#39615);
#11724=VERTEX_POINT('',#39618);
#11725=VERTEX_POINT('',#39620);
#11726=VERTEX_POINT('',#39622);
#11727=VERTEX_POINT('',#39624);
#11728=VERTEX_POINT('',#39626);
#11729=VERTEX_POINT('',#39628);
#11730=VERTEX_POINT('',#39632);
#11731=VERTEX_POINT('',#39635);
#11732=VERTEX_POINT('',#39637);
#11733=VERTEX_POINT('',#39639);
#11734=VERTEX_POINT('',#39641);
#11735=VERTEX_POINT('',#39645);
#11736=VERTEX_POINT('',#39647);
#11737=VERTEX_POINT('',#39649);
#11738=VERTEX_POINT('',#39651);
#11739=VERTEX_POINT('',#39655);
#11740=VERTEX_POINT('',#39659);
#11741=VERTEX_POINT('',#39663);
#11742=VERTEX_POINT('',#39667);
#11743=VERTEX_POINT('',#39671);
#11744=VERTEX_POINT('',#39675);
#11745=VERTEX_POINT('',#39679);
#11746=VERTEX_POINT('',#39680);
#11747=VERTEX_POINT('',#39685);
#11748=VERTEX_POINT('',#39689);
#11749=VERTEX_POINT('',#39693);
#11750=VERTEX_POINT('',#39697);
#11751=VERTEX_POINT('',#39704);
#11752=VERTEX_POINT('',#39712);
#11753=VERTEX_POINT('',#39720);
#11754=VERTEX_POINT('',#39728);
#11755=VERTEX_POINT('',#39736);
#11756=VERTEX_POINT('',#39744);
#11757=VERTEX_POINT('',#39752);
#11758=VERTEX_POINT('',#39760);
#11759=VERTEX_POINT('',#39768);
#11760=VERTEX_POINT('',#39776);
#11761=VERTEX_POINT('',#39809);
#11762=VERTEX_POINT('',#39811);
#11763=VERTEX_POINT('',#39813);
#11764=VERTEX_POINT('',#39815);
#11765=VERTEX_POINT('',#39817);
#11766=VERTEX_POINT('',#39836);
#11767=VERTEX_POINT('',#39840);
#11768=VERTEX_POINT('',#39844);
#11769=VERTEX_POINT('',#39846);
#11770=VERTEX_POINT('',#39850);
#11771=VERTEX_POINT('',#39854);
#11772=VERTEX_POINT('',#39858);
#11773=VERTEX_POINT('',#39860);
#11774=VERTEX_POINT('',#39864);
#11775=VERTEX_POINT('',#39865);
#11776=VERTEX_POINT('',#39870);
#11777=VERTEX_POINT('',#39874);
#11778=VERTEX_POINT('',#39876);
#11779=VERTEX_POINT('',#39880);
#11780=VERTEX_POINT('',#39884);
#11781=VERTEX_POINT('',#39886);
#11782=VERTEX_POINT('',#39890);
#11783=VERTEX_POINT('',#39891);
#11784=VERTEX_POINT('',#39894);
#11785=VERTEX_POINT('',#39898);
#11786=VERTEX_POINT('',#39907);
#11787=VERTEX_POINT('',#39911);
#11788=VERTEX_POINT('',#39917);
#11789=VERTEX_POINT('',#39919);
#11790=VERTEX_POINT('',#39924);
#11791=VERTEX_POINT('',#39928);
#11792=VERTEX_POINT('',#39936);
#11793=VERTEX_POINT('',#39971);
#11794=VERTEX_POINT('',#40008);
#11795=VERTEX_POINT('',#40010);
#11796=VERTEX_POINT('',#40014);
#11797=VERTEX_POINT('',#40016);
#11798=VERTEX_POINT('',#40020);
#11799=VERTEX_POINT('',#40022);
#11800=VERTEX_POINT('',#40026);
#11801=VERTEX_POINT('',#40028);
#11802=VERTEX_POINT('',#40032);
#11803=VERTEX_POINT('',#40034);
#11804=VERTEX_POINT('',#40038);
#11805=VERTEX_POINT('',#40040);
#11806=VERTEX_POINT('',#40044);
#11807=VERTEX_POINT('',#40046);
#11808=VERTEX_POINT('',#40050);
#11809=VERTEX_POINT('',#40052);
#11810=VERTEX_POINT('',#40056);
#11811=VERTEX_POINT('',#40058);
#11812=VERTEX_POINT('',#40062);
#11813=VERTEX_POINT('',#40064);
#11814=VERTEX_POINT('',#40068);
#11815=VERTEX_POINT('',#40070);
#11816=VERTEX_POINT('',#40074);
#11817=VERTEX_POINT('',#40076);
#11818=VERTEX_POINT('',#40080);
#11819=VERTEX_POINT('',#40084);
#11820=VERTEX_POINT('',#40085);
#11821=VERTEX_POINT('',#40087);
#11822=VERTEX_POINT('',#40089);
#11823=VERTEX_POINT('',#40093);
#11824=VERTEX_POINT('',#40104);
#11825=VERTEX_POINT('',#40117);
#11826=VERTEX_POINT('',#40128);
#11827=VERTEX_POINT('',#40141);
#11828=VERTEX_POINT('',#40143);
#11829=VERTEX_POINT('',#40147);
#11830=VERTEX_POINT('',#40149);
#11831=VERTEX_POINT('',#40153);
#11832=VERTEX_POINT('',#40164);
#11833=VERTEX_POINT('',#40177);
#11834=VERTEX_POINT('',#40188);
#11835=VERTEX_POINT('',#40215);
#11836=VERTEX_POINT('',#40217);
#11837=VERTEX_POINT('',#40221);
#11838=VERTEX_POINT('',#40223);
#11839=VERTEX_POINT('',#40227);
#11840=VERTEX_POINT('',#40229);
#11841=VERTEX_POINT('',#40233);
#11842=VERTEX_POINT('',#40235);
#11843=VERTEX_POINT('',#40239);
#11844=VERTEX_POINT('',#40241);
#11845=VERTEX_POINT('',#40245);
#11846=VERTEX_POINT('',#40247);
#11847=VERTEX_POINT('',#40251);
#11848=VERTEX_POINT('',#40253);
#11849=VERTEX_POINT('',#40257);
#11850=VERTEX_POINT('',#40258);
#11851=VERTEX_POINT('',#40260);
#11852=VERTEX_POINT('',#40262);
#11853=VERTEX_POINT('',#40266);
#11854=VERTEX_POINT('',#40268);
#11855=VERTEX_POINT('',#40272);
#11856=VERTEX_POINT('',#40274);
#11857=VERTEX_POINT('',#40278);
#11858=VERTEX_POINT('',#40280);
#11859=VERTEX_POINT('',#40284);
#11860=VERTEX_POINT('',#40286);
#11861=VERTEX_POINT('',#40290);
#11862=VERTEX_POINT('',#40292);
#11863=VERTEX_POINT('',#40296);
#11864=VERTEX_POINT('',#40298);
#11865=VERTEX_POINT('',#40302);
#11866=VERTEX_POINT('',#40304);
#11867=VERTEX_POINT('',#40308);
#11868=VERTEX_POINT('',#40310);
#11869=VERTEX_POINT('',#40314);
#11870=VERTEX_POINT('',#40316);
#11871=VERTEX_POINT('',#40320);
#11872=VERTEX_POINT('',#40322);
#11873=VERTEX_POINT('',#40336);
#11874=VERTEX_POINT('',#40338);
#11875=VERTEX_POINT('',#40342);
#11876=VERTEX_POINT('',#40344);
#11877=VERTEX_POINT('',#40348);
#11878=VERTEX_POINT('',#40349);
#11879=VERTEX_POINT('',#40351);
#11880=VERTEX_POINT('',#40353);
#11881=VERTEX_POINT('',#40357);
#11882=VERTEX_POINT('',#40358);
#11883=VERTEX_POINT('',#40360);
#11884=VERTEX_POINT('',#40362);
#11885=VERTEX_POINT('',#40366);
#11886=VERTEX_POINT('',#40367);
#11887=VERTEX_POINT('',#40369);
#11888=VERTEX_POINT('',#40371);
#11889=VERTEX_POINT('',#40374);
#11890=VERTEX_POINT('',#40376);
#11891=VERTEX_POINT('',#40378);
#11892=VERTEX_POINT('',#40380);
#11893=VERTEX_POINT('',#40385);
#11894=VERTEX_POINT('',#40386);
#11895=VERTEX_POINT('',#40389);
#11896=VERTEX_POINT('',#40391);
#11897=VERTEX_POINT('',#40393);
#11898=VERTEX_POINT('',#40395);
#11899=VERTEX_POINT('',#40398);
#11900=VERTEX_POINT('',#40400);
#11901=VERTEX_POINT('',#40426);
#11902=VERTEX_POINT('',#40428);
#11903=VERTEX_POINT('',#40432);
#11904=VERTEX_POINT('',#40434);
#11905=VERTEX_POINT('',#40438);
#11906=VERTEX_POINT('',#40440);
#11907=VERTEX_POINT('',#40444);
#11908=VERTEX_POINT('',#40446);
#11909=VERTEX_POINT('',#40450);
#11910=VERTEX_POINT('',#40452);
#11911=VERTEX_POINT('',#40456);
#11912=VERTEX_POINT('',#40458);
#11913=VERTEX_POINT('',#40462);
#11914=VERTEX_POINT('',#40464);
#11915=VERTEX_POINT('',#40468);
#11916=VERTEX_POINT('',#40470);
#11917=VERTEX_POINT('',#40474);
#11918=VERTEX_POINT('',#40476);
#11919=VERTEX_POINT('',#40480);
#11920=VERTEX_POINT('',#40482);
#11921=VERTEX_POINT('',#40486);
#11922=VERTEX_POINT('',#40488);
#11923=VERTEX_POINT('',#40492);
#11924=VERTEX_POINT('',#40494);
#11925=VERTEX_POINT('',#40498);
#11926=VERTEX_POINT('',#40500);
#11927=VERTEX_POINT('',#40504);
#11928=VERTEX_POINT('',#40506);
#11929=VERTEX_POINT('',#40510);
#11930=VERTEX_POINT('',#40512);
#11931=VERTEX_POINT('',#40516);
#11932=VERTEX_POINT('',#40518);
#11933=VERTEX_POINT('',#40522);
#11934=VERTEX_POINT('',#40524);
#11935=VERTEX_POINT('',#40528);
#11936=VERTEX_POINT('',#40530);
#11937=VERTEX_POINT('',#40534);
#11938=VERTEX_POINT('',#40536);
#11939=VERTEX_POINT('',#40540);
#11940=VERTEX_POINT('',#40542);
#11941=VERTEX_POINT('',#40546);
#11942=VERTEX_POINT('',#40548);
#11943=VERTEX_POINT('',#40556);
#11944=VERTEX_POINT('',#40557);
#11945=VERTEX_POINT('',#40559);
#11946=VERTEX_POINT('',#40561);
#11947=VERTEX_POINT('',#40563);
#11948=VERTEX_POINT('',#40565);
#11949=VERTEX_POINT('',#40567);
#11950=VERTEX_POINT('',#40569);
#11951=VERTEX_POINT('',#40571);
#11952=VERTEX_POINT('',#40573);
#11953=VERTEX_POINT('',#40575);
#11954=VERTEX_POINT('',#40577);
#11955=VERTEX_POINT('',#40580);
#11956=VERTEX_POINT('',#40581);
#11957=VERTEX_POINT('',#40583);
#11958=VERTEX_POINT('',#40585);
#11959=VERTEX_POINT('',#40587);
#11960=VERTEX_POINT('',#40589);
#11961=VERTEX_POINT('',#40591);
#11962=VERTEX_POINT('',#40593);
#11963=VERTEX_POINT('',#40597);
#11964=VERTEX_POINT('',#40598);
#11965=VERTEX_POINT('',#40603);
#11966=VERTEX_POINT('',#40607);
#11967=VERTEX_POINT('',#40611);
#11968=VERTEX_POINT('',#40615);
#11969=VERTEX_POINT('',#40619);
#11970=VERTEX_POINT('',#40623);
#11971=VERTEX_POINT('',#40627);
#11972=VERTEX_POINT('',#40631);
#11973=VERTEX_POINT('',#40635);
#11974=VERTEX_POINT('',#40639);
#11975=VERTEX_POINT('',#40650);
#11976=VERTEX_POINT('',#40651);
#11977=VERTEX_POINT('',#40653);
#11978=VERTEX_POINT('',#40655);
#11979=VERTEX_POINT('',#40657);
#11980=VERTEX_POINT('',#40659);
#11981=VERTEX_POINT('',#40661);
#11982=VERTEX_POINT('',#40663);
#11983=VERTEX_POINT('',#40683);
#11984=VERTEX_POINT('',#40684);
#11985=VERTEX_POINT('',#40686);
#11986=VERTEX_POINT('',#40688);
#11987=VERTEX_POINT('',#40690);
#11988=VERTEX_POINT('',#40692);
#11989=VERTEX_POINT('',#40696);
#11990=VERTEX_POINT('',#40697);
#11991=VERTEX_POINT('',#40699);
#11992=VERTEX_POINT('',#40701);
#11993=VERTEX_POINT('',#40703);
#11994=VERTEX_POINT('',#40705);
#11995=VERTEX_POINT('',#40709);
#11996=VERTEX_POINT('',#40710);
#11997=VERTEX_POINT('',#40712);
#11998=VERTEX_POINT('',#40714);
#11999=VERTEX_POINT('',#40716);
#12000=VERTEX_POINT('',#40718);
#12001=VERTEX_POINT('',#40722);
#12002=VERTEX_POINT('',#40723);
#12003=VERTEX_POINT('',#40725);
#12004=VERTEX_POINT('',#40727);
#12005=VERTEX_POINT('',#40729);
#12006=VERTEX_POINT('',#40731);
#12007=VERTEX_POINT('',#40735);
#12008=VERTEX_POINT('',#40737);
#12009=VERTEX_POINT('',#40741);
#12010=VERTEX_POINT('',#40745);
#12011=VERTEX_POINT('',#40749);
#12012=VERTEX_POINT('',#40753);
#12013=VERTEX_POINT('',#40760);
#12014=VERTEX_POINT('',#40762);
#12015=VERTEX_POINT('',#40766);
#12016=VERTEX_POINT('',#40770);
#12017=VERTEX_POINT('',#40774);
#12018=VERTEX_POINT('',#40778);
#12019=VERTEX_POINT('',#40785);
#12020=VERTEX_POINT('',#40787);
#12021=VERTEX_POINT('',#40791);
#12022=VERTEX_POINT('',#40795);
#12023=VERTEX_POINT('',#40799);
#12024=VERTEX_POINT('',#40803);
#12025=VERTEX_POINT('',#40810);
#12026=VERTEX_POINT('',#40812);
#12027=VERTEX_POINT('',#40816);
#12028=VERTEX_POINT('',#40820);
#12029=VERTEX_POINT('',#40824);
#12030=VERTEX_POINT('',#40828);
#12031=VERTEX_POINT('',#40840);
#12032=VERTEX_POINT('',#40841);
#12033=VERTEX_POINT('',#40843);
#12034=VERTEX_POINT('',#40845);
#12035=VERTEX_POINT('',#40847);
#12036=VERTEX_POINT('',#40849);
#12037=VERTEX_POINT('',#40851);
#12038=VERTEX_POINT('',#40855);
#12039=VERTEX_POINT('',#40856);
#12040=VERTEX_POINT('',#40875);
#12041=VERTEX_POINT('',#40898);
#12042=VERTEX_POINT('',#40900);
#12043=VERTEX_POINT('',#40939);
#12044=VERTEX_POINT('',#40940);
#12045=VERTEX_POINT('',#40942);
#12046=VERTEX_POINT('',#40947);
#12047=VERTEX_POINT('',#40949);
#12048=VERTEX_POINT('',#40988);
#12049=VERTEX_POINT('',#40989);
#12050=VERTEX_POINT('',#40991);
#12051=VERTEX_POINT('',#40996);
#12052=VERTEX_POINT('',#40998);
#12053=VERTEX_POINT('',#41002);
#12054=VERTEX_POINT('',#41003);
#12055=VERTEX_POINT('',#41005);
#12056=VERTEX_POINT('',#41007);
#12057=VERTEX_POINT('',#41011);
#12058=VERTEX_POINT('',#41013);
#12059=VERTEX_POINT('',#41019);
#12060=VERTEX_POINT('',#41020);
#12061=VERTEX_POINT('',#41022);
#12062=VERTEX_POINT('',#41024);
#12063=VERTEX_POINT('',#41026);
#12064=VERTEX_POINT('',#41028);
#12065=VERTEX_POINT('',#41032);
#12066=VERTEX_POINT('',#41033);
#12067=VERTEX_POINT('',#41035);
#12068=VERTEX_POINT('',#41037);
#12069=VERTEX_POINT('',#41041);
#12070=VERTEX_POINT('',#41042);
#12071=VERTEX_POINT('',#41044);
#12072=VERTEX_POINT('',#41046);
#12073=VERTEX_POINT('',#41050);
#12074=VERTEX_POINT('',#41051);
#12075=VERTEX_POINT('',#41053);
#12076=VERTEX_POINT('',#41055);
#12077=VERTEX_POINT('',#41075);
#12078=VERTEX_POINT('',#41078);
#12079=VERTEX_POINT('',#41083);
#12080=VERTEX_POINT('',#41088);
#12081=VERTEX_POINT('',#41093);
#12082=VERTEX_POINT('',#41098);
#12083=VERTEX_POINT('',#41112);
#12084=VERTEX_POINT('',#41114);
#12085=VERTEX_POINT('',#41118);
#12086=VERTEX_POINT('',#41120);
#12087=VERTEX_POINT('',#41131);
#12088=VERTEX_POINT('',#41133);
#12089=VERTEX_POINT('',#41137);
#12090=VERTEX_POINT('',#41139);
#12091=VERTEX_POINT('',#41143);
#12092=VERTEX_POINT('',#41145);
#12093=VERTEX_POINT('',#41149);
#12094=VERTEX_POINT('',#41151);
#12095=VERTEX_POINT('',#41155);
#12096=VERTEX_POINT('',#41157);
#12097=VERTEX_POINT('',#41161);
#12098=VERTEX_POINT('',#41163);
#12099=VERTEX_POINT('',#41167);
#12100=VERTEX_POINT('',#41168);
#12101=VERTEX_POINT('',#41170);
#12102=VERTEX_POINT('',#41172);
#12103=VERTEX_POINT('',#41176);
#12104=VERTEX_POINT('',#41178);
#12105=VERTEX_POINT('',#41180);
#12106=VERTEX_POINT('',#41182);
#12107=VERTEX_POINT('',#41186);
#12108=VERTEX_POINT('',#41187);
#12109=VERTEX_POINT('',#41190);
#12110=VERTEX_POINT('',#41194);
#12111=VERTEX_POINT('',#41195);
#12112=VERTEX_POINT('',#41197);
#12113=VERTEX_POINT('',#41200);
#12114=VERTEX_POINT('',#41204);
#12115=VERTEX_POINT('',#41206);
#12116=VERTEX_POINT('',#41211);
#12117=VERTEX_POINT('',#41216);
#12118=VERTEX_POINT('',#41222);
#12119=VERTEX_POINT('',#41232);
#12120=VERTEX_POINT('',#41235);
#12121=VERTEX_POINT('',#41239);
#12122=VERTEX_POINT('',#41242);
#12123=VERTEX_POINT('',#41285);
#12124=VERTEX_POINT('',#41286);
#12125=VERTEX_POINT('',#41288);
#12126=VERTEX_POINT('',#41314);
#12127=VERTEX_POINT('',#41425);
#12128=VERTEX_POINT('',#41499);
#12129=VERTEX_POINT('',#41598);
#12130=VERTEX_POINT('',#41599);
#12131=VERTEX_POINT('',#41601);
#12132=VERTEX_POINT('',#41671);
#12133=VERTEX_POINT('',#41838);
#12134=VERTEX_POINT('',#42017);
#12135=VERTEX_POINT('',#42181);
#12136=VERTEX_POINT('',#42377);
#12137=VERTEX_POINT('',#42378);
#12138=VERTEX_POINT('',#42536);
#12139=VERTEX_POINT('',#42667);
#12140=VERTEX_POINT('',#42668);
#12141=VERTEX_POINT('',#42727);
#12142=VERTEX_POINT('',#42750);
#12143=VERTEX_POINT('',#42857);
#12144=VERTEX_POINT('',#42946);
#12145=VERTEX_POINT('',#43007);
#12146=VERTEX_POINT('',#43350);
#12147=VERTEX_POINT('',#43551);
#12148=VERTEX_POINT('',#43552);
#12149=VERTEX_POINT('',#43584);
#12150=VERTEX_POINT('',#43607);
#12151=VERTEX_POINT('',#44128);
#12152=VERTEX_POINT('',#44129);
#12153=VERTEX_POINT('',#44188);
#12154=VERTEX_POINT('',#44211);
#12155=VERTEX_POINT('',#44322);
#12156=VERTEX_POINT('',#44396);
#12157=VERTEX_POINT('',#44495);
#12158=VERTEX_POINT('',#44496);
#12159=VERTEX_POINT('',#44498);
#12160=VERTEX_POINT('',#44568);
#12161=VERTEX_POINT('',#44735);
#12162=VERTEX_POINT('',#44914);
#12163=VERTEX_POINT('',#45070);
#12164=VERTEX_POINT('',#45190);
#12165=VERTEX_POINT('',#45191);
#12166=VERTEX_POINT('',#45346);
#12167=VERTEX_POINT('',#45477);
#12168=VERTEX_POINT('',#45478);
#12169=VERTEX_POINT('',#45537);
#12170=VERTEX_POINT('',#45563);
#12171=VERTEX_POINT('',#45673);
#12172=VERTEX_POINT('',#45762);
#12173=VERTEX_POINT('',#45823);
#12174=VERTEX_POINT('',#46166);
#12175=VERTEX_POINT('',#46363);
#12176=VERTEX_POINT('',#46364);
#12177=VERTEX_POINT('',#46396);
#12178=VERTEX_POINT('',#46422);
#12179=VERTEX_POINT('',#46907);
#12180=VERTEX_POINT('',#46908);
#12181=VERTEX_POINT('',#46967);
#12182=VERTEX_POINT('',#46993);
#12183=VERTEX_POINT('',#47106);
#12184=VERTEX_POINT('',#47180);
#12185=VERTEX_POINT('',#47279);
#12186=VERTEX_POINT('',#47280);
#12187=VERTEX_POINT('',#47282);
#12188=VERTEX_POINT('',#47352);
#12189=VERTEX_POINT('',#47519);
#12190=VERTEX_POINT('',#47698);
#12191=VERTEX_POINT('',#47862);
#12192=VERTEX_POINT('',#48057);
#12193=VERTEX_POINT('',#48058);
#12194=VERTEX_POINT('',#48197);
#12195=VERTEX_POINT('',#48328);
#12196=VERTEX_POINT('',#48329);
#12197=VERTEX_POINT('',#48388);
#12198=VERTEX_POINT('',#48414);
#12199=VERTEX_POINT('',#48526);
#12200=VERTEX_POINT('',#48615);
#12201=VERTEX_POINT('',#48676);
#12202=VERTEX_POINT('',#49052);
#12203=VERTEX_POINT('',#49249);
#12204=VERTEX_POINT('',#49250);
#12205=VERTEX_POINT('',#49282);
#12206=VERTEX_POINT('',#49308);
#12207=VERTEX_POINT('',#49806);
#12208=VERTEX_POINT('',#49807);
#12209=VERTEX_POINT('',#49809);
#12210=VERTEX_POINT('',#49835);
#12211=VERTEX_POINT('',#49946);
#12212=VERTEX_POINT('',#50020);
#12213=VERTEX_POINT('',#50119);
#12214=VERTEX_POINT('',#50120);
#12215=VERTEX_POINT('',#50122);
#12216=VERTEX_POINT('',#50192);
#12217=VERTEX_POINT('',#50359);
#12218=VERTEX_POINT('',#50538);
#12219=VERTEX_POINT('',#50702);
#12220=VERTEX_POINT('',#50895);
#12221=VERTEX_POINT('',#50896);
#12222=VERTEX_POINT('',#51054);
#12223=VERTEX_POINT('',#51193);
#12224=VERTEX_POINT('',#51194);
#12225=VERTEX_POINT('',#51196);
#12226=VERTEX_POINT('',#51222);
#12227=VERTEX_POINT('',#51329);
#12228=VERTEX_POINT('',#51418);
#12229=VERTEX_POINT('',#51479);
#12230=VERTEX_POINT('',#51852);
#12231=VERTEX_POINT('',#52053);
#12232=VERTEX_POINT('',#52054);
#12233=VERTEX_POINT('',#52086);
#12234=VERTEX_POINT('',#52112);
#12235=VERTEX_POINT('',#52618);
#12236=VERTEX_POINT('',#52619);
#12237=VERTEX_POINT('',#52678);
#12238=VERTEX_POINT('',#52701);
#12239=VERTEX_POINT('',#52812);
#12240=VERTEX_POINT('',#52886);
#12241=VERTEX_POINT('',#52985);
#12242=VERTEX_POINT('',#52986);
#12243=VERTEX_POINT('',#52988);
#12244=VERTEX_POINT('',#53058);
#12245=VERTEX_POINT('',#53225);
#12246=VERTEX_POINT('',#53404);
#12247=VERTEX_POINT('',#53560);
#12248=VERTEX_POINT('',#53680);
#12249=VERTEX_POINT('',#53681);
#12250=VERTEX_POINT('',#53836);
#12251=VERTEX_POINT('',#53971);
#12252=VERTEX_POINT('',#53972);
#12253=VERTEX_POINT('',#54031);
#12254=VERTEX_POINT('',#54057);
#12255=VERTEX_POINT('',#54190);
#12256=VERTEX_POINT('',#54279);
#12257=VERTEX_POINT('',#54340);
#12258=VERTEX_POINT('',#54713);
#12259=VERTEX_POINT('',#54914);
#12260=VERTEX_POINT('',#54915);
#12261=VERTEX_POINT('',#54947);
#12262=VERTEX_POINT('',#54973);
#12263=VERTEX_POINT('',#55553);
#12264=VERTEX_POINT('',#55554);
#12265=VERTEX_POINT('',#55613);
#12266=VERTEX_POINT('',#55620);
#12267=VERTEX_POINT('',#55733);
#12268=VERTEX_POINT('',#55807);
#12269=VERTEX_POINT('',#55906);
#12270=VERTEX_POINT('',#55907);
#12271=VERTEX_POINT('',#55909);
#12272=VERTEX_POINT('',#55979);
#12273=VERTEX_POINT('',#56146);
#12274=VERTEX_POINT('',#56325);
#12275=VERTEX_POINT('',#56489);
#12276=VERTEX_POINT('',#56681);
#12277=VERTEX_POINT('',#56682);
#12278=VERTEX_POINT('',#56821);
#12279=VERTEX_POINT('',#56952);
#12280=VERTEX_POINT('',#56953);
#12281=VERTEX_POINT('',#56955);
#12282=VERTEX_POINT('',#56978);
#12283=VERTEX_POINT('',#57085);
#12284=VERTEX_POINT('',#57174);
#12285=VERTEX_POINT('',#57235);
#12286=VERTEX_POINT('',#57605);
#12287=VERTEX_POINT('',#57806);
#12288=VERTEX_POINT('',#57807);
#12289=VERTEX_POINT('',#57839);
#12290=VERTEX_POINT('',#57862);
#12291=VERTEX_POINT('',#58358);
#12292=VERTEX_POINT('',#58359);
#12293=VERTEX_POINT('',#58433);
#12294=VERTEX_POINT('',#58435);
#12295=VERTEX_POINT('',#58603);
#12296=VERTEX_POINT('',#58662);
#12297=VERTEX_POINT('',#58745);
#12298=VERTEX_POINT('',#58746);
#12299=VERTEX_POINT('',#58992);
#12300=VERTEX_POINT('',#59242);
#12301=VERTEX_POINT('',#59244);
#12302=VERTEX_POINT('',#59438);
#12303=VERTEX_POINT('',#59439);
#12304=VERTEX_POINT('',#59463);
#12305=VERTEX_POINT('',#59759);
#12306=VERTEX_POINT('',#59761);
#12307=VERTEX_POINT('',#59958);
#12308=VERTEX_POINT('',#59959);
#12309=VERTEX_POINT('',#59991);
#12310=VERTEX_POINT('',#60014);
#12311=VERTEX_POINT('',#60296);
#12312=VERTEX_POINT('',#60449);
#12313=VERTEX_POINT('',#60569);
#12314=VERTEX_POINT('',#60592);
#12315=VERTEX_POINT('',#60703);
#12316=VERTEX_POINT('',#60819);
#12317=VERTEX_POINT('',#60864);
#12318=VERTEX_POINT('',#61056);
#12319=VERTEX_POINT('',#61153);
#12320=VERTEX_POINT('',#61154);
#12321=VERTEX_POINT('',#61156);
#12322=VERTEX_POINT('',#61173);
#12323=VERTEX_POINT('',#61284);
#12324=VERTEX_POINT('',#61358);
#12325=VERTEX_POINT('',#61457);
#12326=VERTEX_POINT('',#61458);
#12327=VERTEX_POINT('',#61460);
#12328=VERTEX_POINT('',#61530);
#12329=VERTEX_POINT('',#61697);
#12330=VERTEX_POINT('',#61876);
#12331=VERTEX_POINT('',#62036);
#12332=VERTEX_POINT('',#62163);
#12333=VERTEX_POINT('',#62164);
#12334=VERTEX_POINT('',#62316);
#12335=VERTEX_POINT('',#62451);
#12336=VERTEX_POINT('',#62452);
#12337=VERTEX_POINT('',#62511);
#12338=VERTEX_POINT('',#62528);
#12339=VERTEX_POINT('',#62638);
#12340=VERTEX_POINT('',#62727);
#12341=VERTEX_POINT('',#62788);
#12342=VERTEX_POINT('',#63161);
#12343=VERTEX_POINT('',#63362);
#12344=VERTEX_POINT('',#63363);
#12345=VERTEX_POINT('',#63395);
#12346=VERTEX_POINT('',#63412);
#12347=VERTEX_POINT('',#63966);
#12348=VERTEX_POINT('',#63969);
#12349=VERTEX_POINT('',#63973);
#12350=VERTEX_POINT('',#63976);
#12351=VERTEX_POINT('',#63980);
#12352=VERTEX_POINT('',#63983);
#12353=VERTEX_POINT('',#63987);
#12354=VERTEX_POINT('',#63990);
#12355=VERTEX_POINT('',#63994);
#12356=VERTEX_POINT('',#63997);
#12357=VERTEX_POINT('',#64001);
#12358=VERTEX_POINT('',#64004);
#12359=VERTEX_POINT('',#64008);
#12360=VERTEX_POINT('',#64011);
#12361=VERTEX_POINT('',#64017);
#12362=VERTEX_POINT('',#64019);
#12363=VERTEX_POINT('',#64020);
#12364=VERTEX_POINT('',#64022);
#12365=VERTEX_POINT('',#64024);
#12366=VERTEX_POINT('',#64026);
#12367=VERTEX_POINT('',#64028);
#12368=VERTEX_POINT('',#64032);
#12369=VERTEX_POINT('',#64037);
#12370=VERTEX_POINT('',#64038);
#12371=VERTEX_POINT('',#64040);
#12372=VERTEX_POINT('',#64042);
#12373=VERTEX_POINT('',#64044);
#12374=VERTEX_POINT('',#64046);
#12375=VERTEX_POINT('',#64063);
#12376=VERTEX_POINT('',#64065);
#12377=VERTEX_POINT('',#64068);
#12378=VERTEX_POINT('',#64072);
#12379=VERTEX_POINT('',#64076);
#12380=VERTEX_POINT('',#64077);
#12381=VERTEX_POINT('',#64079);
#12382=VERTEX_POINT('',#64081);
#12383=VERTEX_POINT('',#64083);
#12384=VERTEX_POINT('',#64085);
#12385=VERTEX_POINT('',#64089);
#12386=VERTEX_POINT('',#64090);
#12387=VERTEX_POINT('',#64092);
#12388=VERTEX_POINT('',#64094);
#12389=VERTEX_POINT('',#64096);
#12390=VERTEX_POINT('',#64098);
#12391=VERTEX_POINT('',#64114);
#12392=VERTEX_POINT('',#64117);
#12393=VERTEX_POINT('',#64124);
#12394=VERTEX_POINT('',#64126);
#12395=VERTEX_POINT('',#64129);
#12396=VERTEX_POINT('',#64133);
#12397=VERTEX_POINT('',#64137);
#12398=VERTEX_POINT('',#64138);
#12399=VERTEX_POINT('',#64140);
#12400=VERTEX_POINT('',#64142);
#12401=VERTEX_POINT('',#64144);
#12402=VERTEX_POINT('',#64146);
#12403=VERTEX_POINT('',#64150);
#12404=VERTEX_POINT('',#64151);
#12405=VERTEX_POINT('',#64153);
#12406=VERTEX_POINT('',#64155);
#12407=VERTEX_POINT('',#64157);
#12408=VERTEX_POINT('',#64159);
#12409=VERTEX_POINT('',#64175);
#12410=VERTEX_POINT('',#64178);
#12411=VERTEX_POINT('',#64185);
#12412=VERTEX_POINT('',#64186);
#12413=VERTEX_POINT('',#64188);
#12414=VERTEX_POINT('',#64190);
#12415=VERTEX_POINT('',#64194);
#12416=VERTEX_POINT('',#64195);
#12417=VERTEX_POINT('',#64200);
#12418=VERTEX_POINT('',#64201);
#12419=VERTEX_POINT('',#64203);
#12420=VERTEX_POINT('',#64205);
#12421=VERTEX_POINT('',#64209);
#12422=VERTEX_POINT('',#64210);
#12423=VERTEX_POINT('',#64212);
#12424=VERTEX_POINT('',#64214);
#12425=VERTEX_POINT('',#64218);
#12426=VERTEX_POINT('',#64219);
#12427=VERTEX_POINT('',#64224);
#12428=VERTEX_POINT('',#64226);
#12429=VERTEX_POINT('',#64230);
#12430=VERTEX_POINT('',#64234);
#12431=VERTEX_POINT('',#64238);
#12432=VERTEX_POINT('',#64242);
#12433=VERTEX_POINT('',#64247);
#12434=VERTEX_POINT('',#64250);
#12435=VERTEX_POINT('',#64253);
#12436=VERTEX_POINT('',#64254);
#12437=VERTEX_POINT('',#64298);
#12438=VERTEX_POINT('',#64299);
#12439=VERTEX_POINT('',#64332);
#12440=VERTEX_POINT('',#64334);
#12441=VERTEX_POINT('',#64341);
#12442=VERTEX_POINT('',#64346);
#12443=VERTEX_POINT('',#64349);
#12444=VERTEX_POINT('',#64353);
#12445=VERTEX_POINT('',#64356);
#12446=VERTEX_POINT('',#64363);
#12447=VERTEX_POINT('',#64364);
#12448=VERTEX_POINT('',#64397);
#12449=VERTEX_POINT('',#64398);
#12450=VERTEX_POINT('',#64400);
#12451=VERTEX_POINT('',#64402);
#12452=VERTEX_POINT('',#64404);
#12453=VERTEX_POINT('',#64407);
#12454=VERTEX_POINT('',#64410);
#12455=VERTEX_POINT('',#64411);
#12456=VERTEX_POINT('',#64454);
#12457=VERTEX_POINT('',#64456);
#12458=VERTEX_POINT('',#64460);
#12459=VERTEX_POINT('',#64463);
#12460=VERTEX_POINT('',#64469);
#12461=VERTEX_POINT('',#64470);
#12462=VERTEX_POINT('',#64472);
#12463=VERTEX_POINT('',#64474);
#12464=VERTEX_POINT('',#64476);
#12465=VERTEX_POINT('',#64480);
#12466=VERTEX_POINT('',#64482);
#12467=VERTEX_POINT('',#64484);
#12468=VERTEX_POINT('',#64486);
#12469=VERTEX_POINT('',#64493);
#12470=VERTEX_POINT('',#64495);
#12471=VERTEX_POINT('',#64497);
#12472=VERTEX_POINT('',#64499);
#12473=VERTEX_POINT('',#64501);
#12474=VERTEX_POINT('',#64503);
#12475=VERTEX_POINT('',#64505);
#12476=VERTEX_POINT('',#64507);
#12477=VERTEX_POINT('',#64510);
#12478=VERTEX_POINT('',#64512);
#12479=VERTEX_POINT('',#64514);
#12480=VERTEX_POINT('',#64516);
#12481=VERTEX_POINT('',#64520);
#12482=VERTEX_POINT('',#64522);
#12483=VERTEX_POINT('',#64531);
#12484=VERTEX_POINT('',#64533);
#12485=VERTEX_POINT('',#64543);
#12486=VERTEX_POINT('',#64544);
#12487=VERTEX_POINT('',#64546);
#12488=VERTEX_POINT('',#64565);
#12489=VERTEX_POINT('',#64569);
#12490=VERTEX_POINT('',#64570);
#12491=VERTEX_POINT('',#64572);
#12492=VERTEX_POINT('',#64574);
#12493=VERTEX_POINT('',#64593);
#12494=VERTEX_POINT('',#64665);
#12495=VERTEX_POINT('',#64668);
#12496=VERTEX_POINT('',#64670);
#12497=VERTEX_POINT('',#64685);
#12498=VERTEX_POINT('',#64686);
#12499=VERTEX_POINT('',#64691);
#12500=VERTEX_POINT('',#64692);
#12501=VERTEX_POINT('',#64697);
#12502=VERTEX_POINT('',#64699);
#12503=VERTEX_POINT('',#64703);
#12504=VERTEX_POINT('',#64709);
#12505=VERTEX_POINT('',#64717);
#12506=VERTEX_POINT('',#64718);
#12507=VERTEX_POINT('',#64735);
#12508=VERTEX_POINT('',#64737);
#12509=VERTEX_POINT('',#64739);
#12510=VERTEX_POINT('',#64741);
#12511=VERTEX_POINT('',#64743);
#12512=VERTEX_POINT('',#64745);
#12513=VERTEX_POINT('',#64747);
#12514=VERTEX_POINT('',#64750);
#12515=VERTEX_POINT('',#64751);
#12516=VERTEX_POINT('',#64753);
#12517=VERTEX_POINT('',#64755);
#12518=VERTEX_POINT('',#64757);
#12519=VERTEX_POINT('',#64759);
#12520=VERTEX_POINT('',#64761);
#12521=VERTEX_POINT('',#64763);
#12522=VERTEX_POINT('',#64766);
#12523=VERTEX_POINT('',#64767);
#12524=VERTEX_POINT('',#64769);
#12525=VERTEX_POINT('',#64771);
#12526=VERTEX_POINT('',#64773);
#12527=VERTEX_POINT('',#64775);
#12528=VERTEX_POINT('',#64778);
#12529=VERTEX_POINT('',#64779);
#12530=VERTEX_POINT('',#64781);
#12531=VERTEX_POINT('',#64783);
#12532=VERTEX_POINT('',#64785);
#12533=VERTEX_POINT('',#64787);
#12534=VERTEX_POINT('',#64789);
#12535=VERTEX_POINT('',#64791);
#12536=VERTEX_POINT('',#64793);
#12537=VERTEX_POINT('',#64795);
#12538=VERTEX_POINT('',#64797);
#12539=VERTEX_POINT('',#64800);
#12540=VERTEX_POINT('',#64801);
#12541=VERTEX_POINT('',#64803);
#12542=VERTEX_POINT('',#64805);
#12543=VERTEX_POINT('',#64807);
#12544=VERTEX_POINT('',#64809);
#12545=VERTEX_POINT('',#64813);
#12546=VERTEX_POINT('',#64814);
#12547=VERTEX_POINT('',#64816);
#12548=VERTEX_POINT('',#64818);
#12549=VERTEX_POINT('',#64820);
#12550=VERTEX_POINT('',#64822);
#12551=VERTEX_POINT('',#64824);
#12552=VERTEX_POINT('',#64826);
#12553=VERTEX_POINT('',#64846);
#12554=VERTEX_POINT('',#64848);
#12555=VERTEX_POINT('',#64852);
#12556=VERTEX_POINT('',#64856);
#12557=VERTEX_POINT('',#64860);
#12558=VERTEX_POINT('',#64862);
#12559=VERTEX_POINT('',#64866);
#12560=VERTEX_POINT('',#64870);
#12561=VERTEX_POINT('',#64874);
#12562=VERTEX_POINT('',#64878);
#12563=VERTEX_POINT('',#64882);
#12564=VERTEX_POINT('',#64891);
#12565=VERTEX_POINT('',#64892);
#12566=VERTEX_POINT('',#64894);
#12567=VERTEX_POINT('',#64896);
#12568=VERTEX_POINT('',#64898);
#12569=VERTEX_POINT('',#64900);
#12570=VERTEX_POINT('',#64916);
#12571=VERTEX_POINT('',#64918);
#12572=VERTEX_POINT('',#64922);
#12573=VERTEX_POINT('',#64926);
#12574=VERTEX_POINT('',#64930);
#12575=VERTEX_POINT('',#64934);
#12576=VERTEX_POINT('',#64941);
#12577=VERTEX_POINT('',#64943);
#12578=VERTEX_POINT('',#64947);
#12579=VERTEX_POINT('',#64951);
#12580=VERTEX_POINT('',#64955);
#12581=VERTEX_POINT('',#64974);
#12582=VERTEX_POINT('',#64978);
#12583=VERTEX_POINT('',#64980);
#12584=VERTEX_POINT('',#64984);
#12585=VERTEX_POINT('',#64988);
#12586=VERTEX_POINT('',#64992);
#12587=VERTEX_POINT('',#64996);
#12588=VERTEX_POINT('',#65002);
#12589=VERTEX_POINT('',#65027);
#12590=VERTEX_POINT('',#65029);
#12591=VERTEX_POINT('',#65030);
#12592=VERTEX_POINT('',#65032);
#12593=VERTEX_POINT('',#65034);
#12594=VERTEX_POINT('',#65036);
#12595=VERTEX_POINT('',#65038);
#12596=VERTEX_POINT('',#65042);
#12597=VERTEX_POINT('',#65047);
#12598=VERTEX_POINT('',#65048);
#12599=VERTEX_POINT('',#65050);
#12600=VERTEX_POINT('',#65052);
#12601=VERTEX_POINT('',#65054);
#12602=VERTEX_POINT('',#65056);
#12603=VERTEX_POINT('',#65073);
#12604=VERTEX_POINT('',#65075);
#12605=VERTEX_POINT('',#65078);
#12606=VERTEX_POINT('',#65082);
#12607=VERTEX_POINT('',#65086);
#12608=VERTEX_POINT('',#65087);
#12609=VERTEX_POINT('',#65089);
#12610=VERTEX_POINT('',#65091);
#12611=VERTEX_POINT('',#65093);
#12612=VERTEX_POINT('',#65095);
#12613=VERTEX_POINT('',#65099);
#12614=VERTEX_POINT('',#65100);
#12615=VERTEX_POINT('',#65102);
#12616=VERTEX_POINT('',#65104);
#12617=VERTEX_POINT('',#65106);
#12618=VERTEX_POINT('',#65108);
#12619=VERTEX_POINT('',#65124);
#12620=VERTEX_POINT('',#65127);
#12621=VERTEX_POINT('',#65134);
#12622=VERTEX_POINT('',#65136);
#12623=VERTEX_POINT('',#65139);
#12624=VERTEX_POINT('',#65143);
#12625=VERTEX_POINT('',#65147);
#12626=VERTEX_POINT('',#65148);
#12627=VERTEX_POINT('',#65150);
#12628=VERTEX_POINT('',#65152);
#12629=VERTEX_POINT('',#65154);
#12630=VERTEX_POINT('',#65156);
#12631=VERTEX_POINT('',#65160);
#12632=VERTEX_POINT('',#65161);
#12633=VERTEX_POINT('',#65163);
#12634=VERTEX_POINT('',#65165);
#12635=VERTEX_POINT('',#65167);
#12636=VERTEX_POINT('',#65169);
#12637=VERTEX_POINT('',#65185);
#12638=VERTEX_POINT('',#65188);
#12639=VERTEX_POINT('',#65195);
#12640=VERTEX_POINT('',#65196);
#12641=VERTEX_POINT('',#65198);
#12642=VERTEX_POINT('',#65200);
#12643=VERTEX_POINT('',#65204);
#12644=VERTEX_POINT('',#65205);
#12645=VERTEX_POINT('',#65210);
#12646=VERTEX_POINT('',#65211);
#12647=VERTEX_POINT('',#65213);
#12648=VERTEX_POINT('',#65215);
#12649=VERTEX_POINT('',#65219);
#12650=VERTEX_POINT('',#65220);
#12651=VERTEX_POINT('',#65222);
#12652=VERTEX_POINT('',#65224);
#12653=VERTEX_POINT('',#65228);
#12654=VERTEX_POINT('',#65229);
#12655=VERTEX_POINT('',#65234);
#12656=VERTEX_POINT('',#65236);
#12657=VERTEX_POINT('',#65240);
#12658=VERTEX_POINT('',#65244);
#12659=VERTEX_POINT('',#65248);
#12660=VERTEX_POINT('',#65252);
#12661=VERTEX_POINT('',#65257);
#12662=VERTEX_POINT('',#65260);
#12663=VERTEX_POINT('',#65263);
#12664=VERTEX_POINT('',#65264);
#12665=VERTEX_POINT('',#65308);
#12666=VERTEX_POINT('',#65309);
#12667=VERTEX_POINT('',#65342);
#12668=VERTEX_POINT('',#65344);
#12669=VERTEX_POINT('',#65351);
#12670=VERTEX_POINT('',#65356);
#12671=VERTEX_POINT('',#65359);
#12672=VERTEX_POINT('',#65363);
#12673=VERTEX_POINT('',#65366);
#12674=VERTEX_POINT('',#65373);
#12675=VERTEX_POINT('',#65374);
#12676=VERTEX_POINT('',#65407);
#12677=VERTEX_POINT('',#65408);
#12678=VERTEX_POINT('',#65410);
#12679=VERTEX_POINT('',#65412);
#12680=VERTEX_POINT('',#65414);
#12681=VERTEX_POINT('',#65417);
#12682=VERTEX_POINT('',#65420);
#12683=VERTEX_POINT('',#65421);
#12684=VERTEX_POINT('',#65464);
#12685=VERTEX_POINT('',#65466);
#12686=VERTEX_POINT('',#65470);
#12687=VERTEX_POINT('',#65473);
#12688=VERTEX_POINT('',#65479);
#12689=VERTEX_POINT('',#65480);
#12690=VERTEX_POINT('',#65482);
#12691=VERTEX_POINT('',#65484);
#12692=VERTEX_POINT('',#65486);
#12693=VERTEX_POINT('',#65490);
#12694=VERTEX_POINT('',#65492);
#12695=VERTEX_POINT('',#65494);
#12696=VERTEX_POINT('',#65496);
#12697=VERTEX_POINT('',#65503);
#12698=VERTEX_POINT('',#65505);
#12699=VERTEX_POINT('',#65507);
#12700=VERTEX_POINT('',#65509);
#12701=VERTEX_POINT('',#65511);
#12702=VERTEX_POINT('',#65513);
#12703=VERTEX_POINT('',#65515);
#12704=VERTEX_POINT('',#65517);
#12705=VERTEX_POINT('',#65520);
#12706=VERTEX_POINT('',#65522);
#12707=VERTEX_POINT('',#65524);
#12708=VERTEX_POINT('',#65526);
#12709=VERTEX_POINT('',#65534);
#12710=VERTEX_POINT('',#65535);
#12711=VERTEX_POINT('',#65537);
#12712=VERTEX_POINT('',#65556);
#12713=VERTEX_POINT('',#65560);
#12714=VERTEX_POINT('',#65562);
#12715=VERTEX_POINT('',#65564);
#12716=VERTEX_POINT('',#65583);
#12717=VERTEX_POINT('',#65661);
#12718=VERTEX_POINT('',#65662);
#12719=VERTEX_POINT('',#65667);
#12720=VERTEX_POINT('',#65668);
#12721=VERTEX_POINT('',#65673);
#12722=VERTEX_POINT('',#65675);
#12723=VERTEX_POINT('',#65679);
#12724=VERTEX_POINT('',#65685);
#12725=VERTEX_POINT('',#65693);
#12726=VERTEX_POINT('',#65694);
#12727=VERTEX_POINT('',#65711);
#12728=VERTEX_POINT('',#65713);
#12729=VERTEX_POINT('',#65715);
#12730=VERTEX_POINT('',#65717);
#12731=VERTEX_POINT('',#65719);
#12732=VERTEX_POINT('',#65721);
#12733=VERTEX_POINT('',#65723);
#12734=VERTEX_POINT('',#65726);
#12735=VERTEX_POINT('',#65727);
#12736=VERTEX_POINT('',#65729);
#12737=VERTEX_POINT('',#65731);
#12738=VERTEX_POINT('',#65733);
#12739=VERTEX_POINT('',#65735);
#12740=VERTEX_POINT('',#65737);
#12741=VERTEX_POINT('',#65739);
#12742=VERTEX_POINT('',#65742);
#12743=VERTEX_POINT('',#65743);
#12744=VERTEX_POINT('',#65745);
#12745=VERTEX_POINT('',#65747);
#12746=VERTEX_POINT('',#65749);
#12747=VERTEX_POINT('',#65751);
#12748=VERTEX_POINT('',#65754);
#12749=VERTEX_POINT('',#65755);
#12750=VERTEX_POINT('',#65757);
#12751=VERTEX_POINT('',#65759);
#12752=VERTEX_POINT('',#65761);
#12753=VERTEX_POINT('',#65763);
#12754=VERTEX_POINT('',#65765);
#12755=VERTEX_POINT('',#65767);
#12756=VERTEX_POINT('',#65769);
#12757=VERTEX_POINT('',#65771);
#12758=VERTEX_POINT('',#65773);
#12759=VERTEX_POINT('',#65776);
#12760=VERTEX_POINT('',#65777);
#12761=VERTEX_POINT('',#65779);
#12762=VERTEX_POINT('',#65781);
#12763=VERTEX_POINT('',#65783);
#12764=VERTEX_POINT('',#65785);
#12765=VERTEX_POINT('',#65789);
#12766=VERTEX_POINT('',#65790);
#12767=VERTEX_POINT('',#65792);
#12768=VERTEX_POINT('',#65794);
#12769=VERTEX_POINT('',#65796);
#12770=VERTEX_POINT('',#65798);
#12771=VERTEX_POINT('',#65800);
#12772=VERTEX_POINT('',#65802);
#12773=VERTEX_POINT('',#65822);
#12774=VERTEX_POINT('',#65824);
#12775=VERTEX_POINT('',#65828);
#12776=VERTEX_POINT('',#65832);
#12777=VERTEX_POINT('',#65836);
#12778=VERTEX_POINT('',#65838);
#12779=VERTEX_POINT('',#65842);
#12780=VERTEX_POINT('',#65846);
#12781=VERTEX_POINT('',#65850);
#12782=VERTEX_POINT('',#65854);
#12783=VERTEX_POINT('',#65858);
#12784=VERTEX_POINT('',#65867);
#12785=VERTEX_POINT('',#65868);
#12786=VERTEX_POINT('',#65870);
#12787=VERTEX_POINT('',#65872);
#12788=VERTEX_POINT('',#65874);
#12789=VERTEX_POINT('',#65876);
#12790=VERTEX_POINT('',#65892);
#12791=VERTEX_POINT('',#65894);
#12792=VERTEX_POINT('',#65898);
#12793=VERTEX_POINT('',#65902);
#12794=VERTEX_POINT('',#65906);
#12795=VERTEX_POINT('',#65910);
#12796=VERTEX_POINT('',#65917);
#12797=VERTEX_POINT('',#65919);
#12798=VERTEX_POINT('',#65923);
#12799=VERTEX_POINT('',#65927);
#12800=VERTEX_POINT('',#65931);
#12801=VERTEX_POINT('',#65950);
#12802=VERTEX_POINT('',#65954);
#12803=VERTEX_POINT('',#65956);
#12804=VERTEX_POINT('',#65960);
#12805=VERTEX_POINT('',#65964);
#12806=VERTEX_POINT('',#65968);
#12807=VERTEX_POINT('',#65972);
#12808=VERTEX_POINT('',#65978);
#12809=VERTEX_POINT('',#66013);
#12810=VERTEX_POINT('',#66015);
#12811=VERTEX_POINT('',#66019);
#12812=VERTEX_POINT('',#66022);
#12813=VERTEX_POINT('',#66024);
#12814=VERTEX_POINT('',#66028);
#12815=VERTEX_POINT('',#66031);
#12816=VERTEX_POINT('',#66033);
#12817=VERTEX_POINT('',#66037);
#12818=VERTEX_POINT('',#66040);
#12819=VERTEX_POINT('',#66042);
#12820=VERTEX_POINT('',#66046);
#12821=VERTEX_POINT('',#66049);
#12822=VERTEX_POINT('',#66051);
#12823=VERTEX_POINT('',#66055);
#12824=VERTEX_POINT('',#66058);
#12825=VERTEX_POINT('',#66060);
#12826=VERTEX_POINT('',#66064);
#12827=VERTEX_POINT('',#66067);
#12828=VERTEX_POINT('',#66069);
#12829=VERTEX_POINT('',#66073);
#12830=VERTEX_POINT('',#66076);
#12831=VERTEX_POINT('',#66078);
#12832=VERTEX_POINT('',#66082);
#12833=VERTEX_POINT('',#66085);
#12834=VERTEX_POINT('',#66087);
#12835=VERTEX_POINT('',#66091);
#12836=VERTEX_POINT('',#66094);
#12837=VERTEX_POINT('',#66096);
#12838=VERTEX_POINT('',#66100);
#12839=VERTEX_POINT('',#66103);
#12840=VERTEX_POINT('',#66105);
#12841=VERTEX_POINT('',#66109);
#12842=VERTEX_POINT('',#66112);
#12843=VERTEX_POINT('',#66114);
#12844=VERTEX_POINT('',#66118);
#12845=VERTEX_POINT('',#66121);
#12846=VERTEX_POINT('',#66123);
#12847=VERTEX_POINT('',#66127);
#12848=VERTEX_POINT('',#66130);
#12849=VERTEX_POINT('',#66132);
#12850=VERTEX_POINT('',#66136);
#12851=VERTEX_POINT('',#66139);
#12852=VERTEX_POINT('',#66141);
#12853=VERTEX_POINT('',#66145);
#12854=VERTEX_POINT('',#66148);
#12855=VERTEX_POINT('',#66150);
#12856=VERTEX_POINT('',#66154);
#12857=VERTEX_POINT('',#66157);
#12858=VERTEX_POINT('',#66159);
#12859=VERTEX_POINT('',#66163);
#12860=VERTEX_POINT('',#66166);
#12861=VERTEX_POINT('',#66167);
#12862=VERTEX_POINT('',#66169);
#12863=VERTEX_POINT('',#66171);
#12864=VERTEX_POINT('',#66175);
#12865=VERTEX_POINT('',#66177);
#12866=VERTEX_POINT('',#66179);
#12867=VERTEX_POINT('',#66181);
#12868=VERTEX_POINT('',#66183);
#12869=VERTEX_POINT('',#66185);
#12870=VERTEX_POINT('',#66187);
#12871=VERTEX_POINT('',#66189);
#12872=VERTEX_POINT('',#66193);
#12873=VERTEX_POINT('',#66195);
#12874=VERTEX_POINT('',#66199);
#12875=VERTEX_POINT('',#66200);
#12876=VERTEX_POINT('',#66202);
#12877=VERTEX_POINT('',#66204);
#12878=VERTEX_POINT('',#66206);
#12879=VERTEX_POINT('',#66210);
#12880=VERTEX_POINT('',#66229);
#12881=VERTEX_POINT('',#66231);
#12882=VERTEX_POINT('',#66235);
#12883=VERTEX_POINT('',#66239);
#12884=VERTEX_POINT('',#66240);
#12885=VERTEX_POINT('',#66242);
#12886=VERTEX_POINT('',#66247);
#12887=VERTEX_POINT('',#66252);
#12888=VERTEX_POINT('',#66253);
#12889=VERTEX_POINT('',#66255);
#12890=VERTEX_POINT('',#66257);
#12891=VERTEX_POINT('',#66259);
#12892=VERTEX_POINT('',#66261);
#12893=VERTEX_POINT('',#66266);
#12894=VERTEX_POINT('',#66268);
#12895=VERTEX_POINT('',#66272);
#12896=VERTEX_POINT('',#66276);
#12897=VERTEX_POINT('',#66280);
#12898=VERTEX_POINT('',#66284);
#12899=VERTEX_POINT('',#66292);
#12900=VERTEX_POINT('',#66293);
#12901=VERTEX_POINT('',#66296);
#12902=VERTEX_POINT('',#66300);
#12903=VERTEX_POINT('',#66301);
#12904=VERTEX_POINT('',#66303);
#12905=VERTEX_POINT('',#66305);
#12906=VERTEX_POINT('',#66307);
#12907=VERTEX_POINT('',#66309);
#12908=VERTEX_POINT('',#66311);
#12909=VERTEX_POINT('',#66313);
#12910=VERTEX_POINT('',#66317);
#12911=VERTEX_POINT('',#66321);
#12912=VERTEX_POINT('',#66323);
#12913=VERTEX_POINT('',#66327);
#12914=VERTEX_POINT('',#66329);
#12915=VERTEX_POINT('',#66333);
#12916=VERTEX_POINT('',#66334);
#12917=VERTEX_POINT('',#66336);
#12918=VERTEX_POINT('',#66338);
#12919=VERTEX_POINT('',#66340);
#12920=VERTEX_POINT('',#66342);
#12921=VERTEX_POINT('',#66349);
#12922=VERTEX_POINT('',#66352);
#12923=VERTEX_POINT('',#66356);
#12924=VERTEX_POINT('',#66361);
#12925=VERTEX_POINT('',#66366);
#12926=VERTEX_POINT('',#66371);
#12927=VERTEX_POINT('',#66385);
#12928=VERTEX_POINT('',#66387);
#12929=VERTEX_POINT('',#66391);
#12930=VERTEX_POINT('',#66393);
#12931=VERTEX_POINT('',#66399);
#12932=VERTEX_POINT('',#66400);
#12933=VERTEX_POINT('',#66402);
#12934=VERTEX_POINT('',#66404);
#12935=VERTEX_POINT('',#66408);
#12936=VERTEX_POINT('',#66409);
#12937=VERTEX_POINT('',#66411);
#12938=VERTEX_POINT('',#66413);
#12939=VERTEX_POINT('',#66426);
#12940=VERTEX_POINT('',#66428);
#12941=VERTEX_POINT('',#66432);
#12942=VERTEX_POINT('',#66434);
#12943=VERTEX_POINT('',#66438);
#12944=VERTEX_POINT('',#66440);
#12945=VERTEX_POINT('',#66444);
#12946=VERTEX_POINT('',#66446);
#12947=VERTEX_POINT('',#66450);
#12948=VERTEX_POINT('',#66452);
#12949=VERTEX_POINT('',#66456);
#12950=VERTEX_POINT('',#66458);
#12951=VERTEX_POINT('',#66462);
#12952=VERTEX_POINT('',#66464);
#12953=VERTEX_POINT('',#66468);
#12954=VERTEX_POINT('',#66470);
#12955=VERTEX_POINT('',#66474);
#12956=VERTEX_POINT('',#66476);
#12957=VERTEX_POINT('',#66480);
#12958=VERTEX_POINT('',#66482);
#12959=VERTEX_POINT('',#66486);
#12960=VERTEX_POINT('',#66487);
#12961=VERTEX_POINT('',#66489);
#12962=VERTEX_POINT('',#66491);
#12963=VERTEX_POINT('',#66495);
#12964=VERTEX_POINT('',#66497);
#12965=VERTEX_POINT('',#66501);
#12966=VERTEX_POINT('',#66503);
#12967=VERTEX_POINT('',#66505);
#12968=VERTEX_POINT('',#66509);
#12969=VERTEX_POINT('',#66511);
#12970=VERTEX_POINT('',#66515);
#12971=VERTEX_POINT('',#66525);
#12972=VERTEX_POINT('',#66527);
#12973=VERTEX_POINT('',#66531);
#12974=VERTEX_POINT('',#66535);
#12975=VERTEX_POINT('',#66536);
#12976=VERTEX_POINT('',#66538);
#12977=VERTEX_POINT('',#66543);
#12978=VERTEX_POINT('',#66548);
#12979=VERTEX_POINT('',#66549);
#12980=VERTEX_POINT('',#66551);
#12981=VERTEX_POINT('',#66553);
#12982=VERTEX_POINT('',#66555);
#12983=VERTEX_POINT('',#66557);
#12984=VERTEX_POINT('',#66562);
#12985=VERTEX_POINT('',#66564);
#12986=VERTEX_POINT('',#66568);
#12987=VERTEX_POINT('',#66572);
#12988=VERTEX_POINT('',#66576);
#12989=VERTEX_POINT('',#66580);
#12990=EDGE_CURVE('',#10638,#10638,#9461,.T.);
#12991=EDGE_CURVE('',#10638,#10639,#5483,.T.);
#12992=EDGE_CURVE('',#10639,#10639,#9462,.T.);
#12993=EDGE_CURVE('',#10640,#10640,#9463,.T.);
#12994=EDGE_CURVE('',#10640,#10641,#5484,.T.);
#12995=EDGE_CURVE('',#10641,#10641,#9464,.T.);
#12996=EDGE_CURVE('',#10642,#10642,#9465,.T.);
#12997=EDGE_CURVE('',#10642,#10643,#5485,.T.);
#12998=EDGE_CURVE('',#10643,#10643,#9466,.T.);
#12999=EDGE_CURVE('',#10644,#10644,#9467,.T.);
#13000=EDGE_CURVE('',#10644,#10645,#5486,.T.);
#13001=EDGE_CURVE('',#10645,#10645,#9468,.T.);
#13002=EDGE_CURVE('',#10646,#10647,#5487,.T.);
#13003=EDGE_CURVE('',#10648,#10647,#5488,.T.);
#13004=EDGE_CURVE('',#10649,#10648,#5489,.T.);
#13005=EDGE_CURVE('',#10649,#10646,#5490,.T.);
#13006=EDGE_CURVE('',#10647,#10650,#5491,.T.);
#13007=EDGE_CURVE('',#10651,#10650,#5492,.T.);
#13008=EDGE_CURVE('',#10648,#10651,#5493,.T.);
#13009=EDGE_CURVE('',#10650,#10652,#5494,.T.);
#13010=EDGE_CURVE('',#10653,#10652,#5495,.T.);
#13011=EDGE_CURVE('',#10651,#10653,#5496,.T.);
#13012=EDGE_CURVE('',#10652,#10646,#5497,.T.);
#13013=EDGE_CURVE('',#10653,#10649,#5498,.T.);
#13014=EDGE_CURVE('',#10654,#10655,#5499,.T.);
#13015=EDGE_CURVE('',#10656,#10654,#5500,.T.);
#13016=EDGE_CURVE('',#10657,#10656,#5501,.T.);
#13017=EDGE_CURVE('',#10655,#10657,#5502,.T.);
#13018=EDGE_CURVE('',#10658,#10659,#5503,.T.);
#13019=EDGE_CURVE('',#10660,#10658,#5504,.T.);
#13020=EDGE_CURVE('',#10661,#10660,#5505,.T.);
#13021=EDGE_CURVE('',#10659,#10661,#5506,.T.);
#13022=EDGE_CURVE('',#10662,#10663,#5507,.T.);
#13023=EDGE_CURVE('',#10663,#10664,#5508,.T.);
#13024=EDGE_CURVE('',#10664,#10665,#5509,.T.);
#13025=EDGE_CURVE('',#10665,#10662,#5510,.T.);
#13026=EDGE_CURVE('',#10666,#10667,#5511,.T.);
#13027=EDGE_CURVE('',#10667,#10668,#5512,.T.);
#13028=EDGE_CURVE('',#10668,#10669,#5513,.T.);
#13029=EDGE_CURVE('',#10669,#10666,#5514,.T.);
#13030=EDGE_CURVE('',#10667,#10658,#5515,.T.);
#13031=EDGE_CURVE('',#10666,#10660,#5516,.T.);
#13032=EDGE_CURVE('',#10669,#10661,#5517,.T.);
#13033=EDGE_CURVE('',#10668,#10659,#5518,.T.);
#13034=EDGE_CURVE('',#10663,#10654,#5519,.T.);
#13035=EDGE_CURVE('',#10662,#10656,#5520,.T.);
#13036=EDGE_CURVE('',#10665,#10657,#5521,.T.);
#13037=EDGE_CURVE('',#10664,#10655,#5522,.T.);
#13038=EDGE_CURVE('',#10670,#10670,#9469,.T.);
#13039=EDGE_CURVE('',#10670,#10671,#5523,.T.);
#13040=EDGE_CURVE('',#10671,#10671,#9470,.T.);
#13041=EDGE_CURVE('',#10672,#10672,#9471,.T.);
#13042=EDGE_CURVE('',#10672,#10673,#5524,.T.);
#13043=EDGE_CURVE('',#10673,#10673,#9472,.T.);
#13044=EDGE_CURVE('',#10674,#10674,#9473,.T.);
#13045=EDGE_CURVE('',#10674,#10675,#5525,.T.);
#13046=EDGE_CURVE('',#10675,#10675,#9474,.T.);
#13047=EDGE_CURVE('',#10676,#10676,#9475,.T.);
#13048=EDGE_CURVE('',#10676,#10677,#5526,.T.);
#13049=EDGE_CURVE('',#10677,#10677,#9476,.T.);
#13050=EDGE_CURVE('',#10678,#10679,#5527,.T.);
#13051=EDGE_CURVE('',#10680,#10678,#5528,.T.);
#13052=EDGE_CURVE('',#10680,#10681,#5529,.T.);
#13053=EDGE_CURVE('',#10681,#10679,#5530,.T.);
#13054=EDGE_CURVE('',#10682,#10680,#5531,.T.);
#13055=EDGE_CURVE('',#10683,#10682,#5532,.T.);
#13056=EDGE_CURVE('',#10683,#10684,#5533,.T.);
#13057=EDGE_CURVE('',#10684,#10685,#5534,.T.);
#13058=EDGE_CURVE('',#10681,#10685,#5535,.T.);
#13059=EDGE_CURVE('',#10686,#10687,#5536,.T.);
#13060=EDGE_CURVE('',#10686,#10679,#5537,.T.);
#13061=EDGE_CURVE('',#10685,#10688,#5538,.T.);
#13062=EDGE_CURVE('',#10687,#10688,#5539,.T.);
#13063=EDGE_CURVE('',#10689,#10690,#5540,.T.);
#13064=EDGE_CURVE('',#10691,#10689,#5541,.T.);
#13065=EDGE_CURVE('',#10687,#10691,#5542,.T.);
#13066=EDGE_CURVE('',#10688,#10692,#5543,.T.);
#13067=EDGE_CURVE('',#10690,#10692,#5544,.T.);
#13068=EDGE_CURVE('',#10693,#10683,#5545,.T.);
#13069=EDGE_CURVE('',#10693,#10694,#5546,.T.);
#13070=EDGE_CURVE('',#10690,#10694,#5547,.T.);
#13071=EDGE_CURVE('',#10692,#10684,#5548,.T.);
#13072=EDGE_CURVE('',#10695,#10694,#5549,.T.);
#13073=EDGE_CURVE('',#10689,#10695,#5550,.T.);
#13074=EDGE_CURVE('',#10696,#10686,#5551,.T.);
#13075=EDGE_CURVE('',#10696,#10678,#5552,.T.);
#13076=EDGE_CURVE('',#10682,#10696,#5553,.T.);
#13077=EDGE_CURVE('',#10697,#10693,#5554,.T.);
#13078=EDGE_CURVE('',#10697,#10695,#5555,.T.);
#13079=EDGE_CURVE('',#10691,#10697,#5556,.T.);
#13080=EDGE_CURVE('',#10698,#10698,#9477,.T.);
#13081=EDGE_CURVE('',#10698,#10699,#5557,.T.);
#13082=EDGE_CURVE('',#10699,#10699,#9478,.T.);
#13083=EDGE_CURVE('',#10700,#10700,#9479,.T.);
#13084=EDGE_CURVE('',#10700,#10701,#5558,.T.);
#13085=EDGE_CURVE('',#10701,#10701,#9480,.T.);
#13086=EDGE_CURVE('',#10702,#10702,#9481,.T.);
#13087=EDGE_CURVE('',#10702,#10703,#5559,.T.);
#13088=EDGE_CURVE('',#10703,#10703,#9482,.T.);
#13089=EDGE_CURVE('',#10704,#10704,#9483,.T.);
#13090=EDGE_CURVE('',#10704,#10705,#5560,.T.);
#13091=EDGE_CURVE('',#10705,#10705,#9484,.T.);
#13092=EDGE_CURVE('',#10706,#10706,#9485,.T.);
#13093=EDGE_CURVE('',#10706,#10707,#5561,.T.);
#13094=EDGE_CURVE('',#10707,#10707,#9486,.T.);
#13095=EDGE_CURVE('',#10708,#10708,#9487,.T.);
#13096=EDGE_CURVE('',#10708,#10709,#5562,.T.);
#13097=EDGE_CURVE('',#10709,#10709,#9488,.T.);
#13098=EDGE_CURVE('',#10710,#10710,#9489,.T.);
#13099=EDGE_CURVE('',#10710,#10711,#5563,.T.);
#13100=EDGE_CURVE('',#10711,#10711,#9490,.T.);
#13101=EDGE_CURVE('',#10712,#10712,#9491,.T.);
#13102=EDGE_CURVE('',#10712,#10713,#5564,.T.);
#13103=EDGE_CURVE('',#10713,#10713,#9492,.T.);
#13104=EDGE_CURVE('',#10714,#10714,#9493,.T.);
#13105=EDGE_CURVE('',#10714,#10715,#5565,.T.);
#13106=EDGE_CURVE('',#10715,#10715,#9494,.T.);
#13107=EDGE_CURVE('',#10716,#10716,#9495,.T.);
#13108=EDGE_CURVE('',#10716,#10717,#5566,.T.);
#13109=EDGE_CURVE('',#10717,#10717,#9496,.T.);
#13110=EDGE_CURVE('',#10718,#10718,#9497,.T.);
#13111=EDGE_CURVE('',#10718,#10719,#5567,.T.);
#13112=EDGE_CURVE('',#10719,#10719,#9498,.T.);
#13113=EDGE_CURVE('',#10720,#10720,#9499,.T.);
#13114=EDGE_CURVE('',#10720,#10721,#5568,.T.);
#13115=EDGE_CURVE('',#10721,#10721,#9500,.T.);
#13116=EDGE_CURVE('',#10722,#10723,#5569,.T.);
#13117=EDGE_CURVE('',#10724,#10722,#5570,.T.);
#13118=EDGE_CURVE('',#10725,#10724,#5571,.T.);
#13119=EDGE_CURVE('',#10723,#10725,#5572,.T.);
#13120=EDGE_CURVE('',#10726,#10723,#5573,.T.);
#13121=EDGE_CURVE('',#10727,#10726,#5574,.T.);
#13122=EDGE_CURVE('',#10727,#10722,#5575,.T.);
#13123=EDGE_CURVE('',#10728,#10725,#5576,.T.);
#13124=EDGE_CURVE('',#10726,#10728,#5577,.T.);
#13125=EDGE_CURVE('',#10729,#10724,#5578,.T.);
#13126=EDGE_CURVE('',#10728,#10729,#5579,.T.);
#13127=EDGE_CURVE('',#10729,#10727,#5580,.T.);
#13128=EDGE_CURVE('',#10730,#10730,#9501,.T.);
#13129=EDGE_CURVE('',#10730,#10731,#5581,.T.);
#13130=EDGE_CURVE('',#10731,#10731,#9502,.T.);
#13131=EDGE_CURVE('',#10732,#10732,#9503,.T.);
#13132=EDGE_CURVE('',#10732,#10733,#5582,.T.);
#13133=EDGE_CURVE('',#10733,#10733,#9504,.T.);
#13134=EDGE_CURVE('',#10734,#10734,#9505,.T.);
#13135=EDGE_CURVE('',#10734,#10735,#5583,.T.);
#13136=EDGE_CURVE('',#10735,#10735,#9506,.T.);
#13137=EDGE_CURVE('',#10736,#10736,#9507,.T.);
#13138=EDGE_CURVE('',#10736,#10737,#5584,.T.);
#13139=EDGE_CURVE('',#10737,#10737,#9508,.T.);
#13140=EDGE_CURVE('',#10738,#10738,#9509,.T.);
#13141=EDGE_CURVE('',#10738,#10739,#5585,.T.);
#13142=EDGE_CURVE('',#10739,#10739,#9510,.T.);
#13143=EDGE_CURVE('',#10740,#10740,#9511,.T.);
#13144=EDGE_CURVE('',#10740,#10741,#5586,.T.);
#13145=EDGE_CURVE('',#10741,#10741,#9512,.T.);
#13146=EDGE_CURVE('',#10742,#10742,#9513,.T.);
#13147=EDGE_CURVE('',#10742,#10743,#5587,.T.);
#13148=EDGE_CURVE('',#10743,#10743,#9514,.T.);
#13149=EDGE_CURVE('',#10744,#10745,#5588,.T.);
#13150=EDGE_CURVE('',#10744,#10746,#9515,.T.);
#13151=EDGE_CURVE('',#10747,#10746,#5589,.T.);
#13152=EDGE_CURVE('',#10747,#10748,#5590,.T.);
#13153=EDGE_CURVE('',#10748,#10749,#5591,.T.);
#13154=EDGE_CURVE('',#10749,#10745,#9516,.T.);
#13155=EDGE_CURVE('',#10750,#10751,#5592,.T.);
#13156=EDGE_CURVE('',#10750,#10744,#5593,.T.);
#13157=EDGE_CURVE('',#10745,#10751,#5594,.T.);
#13158=EDGE_CURVE('',#10752,#10753,#5595,.T.);
#13159=EDGE_CURVE('',#10752,#10750,#9517,.T.);
#13160=EDGE_CURVE('',#10751,#10754,#9518,.T.);
#13161=EDGE_CURVE('',#10754,#10755,#5596,.T.);
#13162=EDGE_CURVE('',#10753,#10755,#5597,.T.);
#13163=EDGE_CURVE('',#10755,#10748,#5598,.T.);
#13164=EDGE_CURVE('',#10753,#10747,#5599,.T.);
#13165=EDGE_CURVE('',#10746,#10752,#5600,.T.);
#13166=EDGE_CURVE('',#10754,#10749,#5601,.T.);
#13167=EDGE_CURVE('',#10756,#10756,#9519,.T.);
#13168=EDGE_CURVE('',#10756,#10757,#5602,.T.);
#13169=EDGE_CURVE('',#10757,#10757,#9520,.T.);
#13170=EDGE_CURVE('',#10758,#10758,#9521,.T.);
#13171=EDGE_CURVE('',#10758,#10759,#5603,.T.);
#13172=EDGE_CURVE('',#10759,#10759,#9522,.T.);
#13173=EDGE_CURVE('',#10760,#10760,#9523,.T.);
#13174=EDGE_CURVE('',#10760,#10761,#5604,.T.);
#13175=EDGE_CURVE('',#10761,#10761,#9524,.T.);
#13176=EDGE_CURVE('',#10762,#10762,#9525,.T.);
#13177=EDGE_CURVE('',#10762,#10763,#5605,.T.);
#13178=EDGE_CURVE('',#10763,#10763,#9526,.T.);
#13179=EDGE_CURVE('',#10764,#10764,#9527,.T.);
#13180=EDGE_CURVE('',#10764,#10765,#5606,.T.);
#13181=EDGE_CURVE('',#10765,#10765,#9528,.T.);
#13182=EDGE_CURVE('',#10766,#10766,#9529,.T.);
#13183=EDGE_CURVE('',#10766,#10767,#5607,.T.);
#13184=EDGE_CURVE('',#10767,#10767,#9530,.T.);
#13185=EDGE_CURVE('',#10768,#10769,#5608,.T.);
#13186=EDGE_CURVE('',#10770,#10769,#5609,.T.);
#13187=EDGE_CURVE('',#10771,#10770,#5610,.T.);
#13188=EDGE_CURVE('',#10771,#10768,#5611,.T.);
#13189=EDGE_CURVE('',#10769,#10772,#5612,.T.);
#13190=EDGE_CURVE('',#10773,#10772,#5613,.T.);
#13191=EDGE_CURVE('',#10770,#10773,#5614,.T.);
#13192=EDGE_CURVE('',#10772,#10774,#5615,.T.);
#13193=EDGE_CURVE('',#10775,#10774,#5616,.T.);
#13194=EDGE_CURVE('',#10773,#10775,#5617,.T.);
#13195=EDGE_CURVE('',#10774,#10768,#5618,.T.);
#13196=EDGE_CURVE('',#10775,#10771,#5619,.T.);
#13197=EDGE_CURVE('',#10776,#10776,#9531,.T.);
#13198=EDGE_CURVE('',#10776,#10777,#5620,.T.);
#13199=EDGE_CURVE('',#10777,#10777,#9532,.T.);
#13200=EDGE_CURVE('',#10778,#10778,#9533,.T.);
#13201=EDGE_CURVE('',#10778,#10779,#5621,.T.);
#13202=EDGE_CURVE('',#10779,#10779,#9534,.T.);
#13203=EDGE_CURVE('',#10780,#10780,#9535,.T.);
#13204=EDGE_CURVE('',#10780,#10781,#5622,.T.);
#13205=EDGE_CURVE('',#10781,#10781,#9536,.T.);
#13206=EDGE_CURVE('',#10782,#10782,#9537,.T.);
#13207=EDGE_CURVE('',#10782,#10783,#5623,.T.);
#13208=EDGE_CURVE('',#10783,#10783,#9538,.T.);
#13209=EDGE_CURVE('',#10784,#10784,#9539,.T.);
#13210=EDGE_CURVE('',#10784,#10785,#5624,.T.);
#13211=EDGE_CURVE('',#10785,#10785,#9540,.T.);
#13212=EDGE_CURVE('',#10786,#10786,#9541,.T.);
#13213=EDGE_CURVE('',#10786,#10787,#5625,.T.);
#13214=EDGE_CURVE('',#10787,#10787,#9542,.T.);
#13215=EDGE_CURVE('',#10788,#10789,#5626,.T.);
#13216=EDGE_CURVE('',#10790,#10789,#5627,.T.);
#13217=EDGE_CURVE('',#10791,#10790,#5628,.T.);
#13218=EDGE_CURVE('',#10791,#10788,#5629,.T.);
#13219=EDGE_CURVE('',#10789,#10792,#5630,.T.);
#13220=EDGE_CURVE('',#10793,#10792,#5631,.T.);
#13221=EDGE_CURVE('',#10790,#10793,#5632,.T.);
#13222=EDGE_CURVE('',#10792,#10794,#5633,.T.);
#13223=EDGE_CURVE('',#10795,#10794,#5634,.T.);
#13224=EDGE_CURVE('',#10793,#10795,#5635,.T.);
#13225=EDGE_CURVE('',#10794,#10788,#5636,.T.);
#13226=EDGE_CURVE('',#10795,#10791,#5637,.T.);
#13227=EDGE_CURVE('',#10796,#10796,#9543,.T.);
#13228=EDGE_CURVE('',#10796,#10797,#5638,.T.);
#13229=EDGE_CURVE('',#10797,#10797,#9544,.T.);
#13230=EDGE_CURVE('',#10798,#10799,#9545,.T.);
#13231=EDGE_CURVE('',#10800,#10798,#582,.T.);
#13232=EDGE_CURVE('',#10801,#10800,#9546,.T.);
#13233=EDGE_CURVE('',#10802,#10801,#583,.T.);
#13234=EDGE_CURVE('',#10803,#10802,#9547,.T.);
#13235=EDGE_CURVE('',#10803,#10804,#5639,.T.);
#13236=EDGE_CURVE('',#10804,#10804,#9548,.T.);
#13237=EDGE_CURVE('',#10805,#10803,#9549,.T.);
#13238=EDGE_CURVE('',#10806,#10805,#584,.T.);
#13239=EDGE_CURVE('',#10807,#10806,#9550,.T.);
#13240=EDGE_CURVE('',#10799,#10807,#585,.T.);
#13241=EDGE_CURVE('',#10808,#10808,#9551,.T.);
#13242=EDGE_CURVE('',#10808,#10809,#5640,.T.);
#13243=EDGE_CURVE('',#10809,#10809,#9552,.T.);
#13244=EDGE_CURVE('',#10810,#10811,#9553,.T.);
#13245=EDGE_CURVE('',#10812,#10810,#586,.T.);
#13246=EDGE_CURVE('',#10813,#10812,#9554,.T.);
#13247=EDGE_CURVE('',#10814,#10813,#587,.T.);
#13248=EDGE_CURVE('',#10815,#10814,#9555,.T.);
#13249=EDGE_CURVE('',#10815,#10816,#5641,.T.);
#13250=EDGE_CURVE('',#10816,#10816,#9556,.T.);
#13251=EDGE_CURVE('',#10817,#10815,#9557,.T.);
#13252=EDGE_CURVE('',#10818,#10817,#588,.T.);
#13253=EDGE_CURVE('',#10819,#10818,#9558,.T.);
#13254=EDGE_CURVE('',#10811,#10819,#589,.T.);
#13255=EDGE_CURVE('',#10820,#10820,#9559,.T.);
#13256=EDGE_CURVE('',#10820,#10821,#5642,.T.);
#13257=EDGE_CURVE('',#10821,#10821,#9560,.T.);
#13258=EDGE_CURVE('',#10822,#10823,#9561,.T.);
#13259=EDGE_CURVE('',#10824,#10822,#590,.T.);
#13260=EDGE_CURVE('',#10825,#10824,#9562,.T.);
#13261=EDGE_CURVE('',#10826,#10825,#591,.T.);
#13262=EDGE_CURVE('',#10827,#10826,#9563,.T.);
#13263=EDGE_CURVE('',#10827,#10828,#5643,.T.);
#13264=EDGE_CURVE('',#10828,#10828,#9564,.T.);
#13265=EDGE_CURVE('',#10829,#10827,#9565,.T.);
#13266=EDGE_CURVE('',#10830,#10829,#592,.T.);
#13267=EDGE_CURVE('',#10831,#10830,#9566,.T.);
#13268=EDGE_CURVE('',#10823,#10831,#593,.T.);
#13269=EDGE_CURVE('',#10832,#10832,#9567,.T.);
#13270=EDGE_CURVE('',#10832,#10833,#5644,.T.);
#13271=EDGE_CURVE('',#10833,#10833,#9568,.T.);
#13272=EDGE_CURVE('',#10834,#10835,#9569,.T.);
#13273=EDGE_CURVE('',#10836,#10834,#594,.T.);
#13274=EDGE_CURVE('',#10837,#10836,#9570,.T.);
#13275=EDGE_CURVE('',#10838,#10837,#595,.T.);
#13276=EDGE_CURVE('',#10839,#10838,#9571,.T.);
#13277=EDGE_CURVE('',#10839,#10840,#5645,.T.);
#13278=EDGE_CURVE('',#10840,#10840,#9572,.T.);
#13279=EDGE_CURVE('',#10841,#10839,#9573,.T.);
#13280=EDGE_CURVE('',#10842,#10841,#596,.T.);
#13281=EDGE_CURVE('',#10843,#10842,#9574,.T.);
#13282=EDGE_CURVE('',#10835,#10843,#597,.T.);
#13283=EDGE_CURVE('',#10844,#10844,#9575,.T.);
#13284=EDGE_CURVE('',#10844,#10845,#5646,.T.);
#13285=EDGE_CURVE('',#10845,#10845,#9576,.T.);
#13286=EDGE_CURVE('',#10846,#10847,#9577,.T.);
#13287=EDGE_CURVE('',#10848,#10846,#598,.T.);
#13288=EDGE_CURVE('',#10849,#10848,#9578,.T.);
#13289=EDGE_CURVE('',#10850,#10849,#599,.T.);
#13290=EDGE_CURVE('',#10851,#10850,#9579,.T.);
#13291=EDGE_CURVE('',#10851,#10852,#5647,.T.);
#13292=EDGE_CURVE('',#10852,#10852,#9580,.T.);
#13293=EDGE_CURVE('',#10853,#10851,#9581,.T.);
#13294=EDGE_CURVE('',#10854,#10853,#600,.T.);
#13295=EDGE_CURVE('',#10855,#10854,#9582,.T.);
#13296=EDGE_CURVE('',#10847,#10855,#601,.T.);
#13297=EDGE_CURVE('',#10856,#10856,#9583,.T.);
#13298=EDGE_CURVE('',#10856,#10857,#5648,.T.);
#13299=EDGE_CURVE('',#10857,#10857,#9584,.T.);
#13300=EDGE_CURVE('',#10858,#10859,#9585,.T.);
#13301=EDGE_CURVE('',#10860,#10858,#602,.T.);
#13302=EDGE_CURVE('',#10861,#10860,#9586,.T.);
#13303=EDGE_CURVE('',#10862,#10861,#603,.T.);
#13304=EDGE_CURVE('',#10863,#10862,#9587,.T.);
#13305=EDGE_CURVE('',#10863,#10864,#5649,.T.);
#13306=EDGE_CURVE('',#10864,#10864,#9588,.T.);
#13307=EDGE_CURVE('',#10865,#10863,#9589,.T.);
#13308=EDGE_CURVE('',#10866,#10865,#604,.T.);
#13309=EDGE_CURVE('',#10867,#10866,#9590,.T.);
#13310=EDGE_CURVE('',#10859,#10867,#605,.T.);
#13311=EDGE_CURVE('',#10868,#10868,#9591,.T.);
#13312=EDGE_CURVE('',#10868,#10869,#5650,.T.);
#13313=EDGE_CURVE('',#10869,#10869,#9592,.T.);
#13314=EDGE_CURVE('',#10870,#10871,#9593,.T.);
#13315=EDGE_CURVE('',#10872,#10870,#606,.T.);
#13316=EDGE_CURVE('',#10873,#10872,#9594,.T.);
#13317=EDGE_CURVE('',#10874,#10873,#607,.T.);
#13318=EDGE_CURVE('',#10875,#10874,#9595,.T.);
#13319=EDGE_CURVE('',#10875,#10876,#5651,.T.);
#13320=EDGE_CURVE('',#10876,#10876,#9596,.T.);
#13321=EDGE_CURVE('',#10877,#10875,#9597,.T.);
#13322=EDGE_CURVE('',#10878,#10877,#608,.T.);
#13323=EDGE_CURVE('',#10879,#10878,#9598,.T.);
#13324=EDGE_CURVE('',#10871,#10879,#609,.T.);
#13325=EDGE_CURVE('',#10880,#10880,#9599,.T.);
#13326=EDGE_CURVE('',#10880,#10881,#5652,.T.);
#13327=EDGE_CURVE('',#10881,#10881,#9600,.T.);
#13328=EDGE_CURVE('',#10882,#10883,#9601,.T.);
#13329=EDGE_CURVE('',#10884,#10882,#610,.T.);
#13330=EDGE_CURVE('',#10885,#10884,#9602,.T.);
#13331=EDGE_CURVE('',#10886,#10885,#611,.T.);
#13332=EDGE_CURVE('',#10887,#10886,#9603,.T.);
#13333=EDGE_CURVE('',#10887,#10888,#5653,.T.);
#13334=EDGE_CURVE('',#10888,#10888,#9604,.T.);
#13335=EDGE_CURVE('',#10889,#10887,#9605,.T.);
#13336=EDGE_CURVE('',#10890,#10889,#612,.T.);
#13337=EDGE_CURVE('',#10891,#10890,#9606,.T.);
#13338=EDGE_CURVE('',#10883,#10891,#613,.T.);
#13339=EDGE_CURVE('',#10892,#10892,#9607,.T.);
#13340=EDGE_CURVE('',#10892,#10893,#5654,.T.);
#13341=EDGE_CURVE('',#10893,#10893,#9608,.T.);
#13342=EDGE_CURVE('',#10894,#10895,#9609,.T.);
#13343=EDGE_CURVE('',#10896,#10894,#614,.T.);
#13344=EDGE_CURVE('',#10897,#10896,#9610,.T.);
#13345=EDGE_CURVE('',#10898,#10897,#615,.T.);
#13346=EDGE_CURVE('',#10899,#10898,#9611,.T.);
#13347=EDGE_CURVE('',#10899,#10900,#5655,.T.);
#13348=EDGE_CURVE('',#10900,#10900,#9612,.T.);
#13349=EDGE_CURVE('',#10901,#10899,#9613,.T.);
#13350=EDGE_CURVE('',#10902,#10901,#616,.T.);
#13351=EDGE_CURVE('',#10903,#10902,#9614,.T.);
#13352=EDGE_CURVE('',#10895,#10903,#617,.T.);
#13353=EDGE_CURVE('',#10904,#10904,#9615,.T.);
#13354=EDGE_CURVE('',#10904,#10905,#5656,.T.);
#13355=EDGE_CURVE('',#10905,#10905,#9616,.T.);
#13356=EDGE_CURVE('',#10906,#10907,#9617,.T.);
#13357=EDGE_CURVE('',#10908,#10906,#618,.T.);
#13358=EDGE_CURVE('',#10909,#10908,#9618,.T.);
#13359=EDGE_CURVE('',#10910,#10909,#619,.T.);
#13360=EDGE_CURVE('',#10911,#10910,#9619,.T.);
#13361=EDGE_CURVE('',#10911,#10912,#5657,.T.);
#13362=EDGE_CURVE('',#10912,#10912,#9620,.T.);
#13363=EDGE_CURVE('',#10913,#10911,#9621,.T.);
#13364=EDGE_CURVE('',#10914,#10913,#620,.T.);
#13365=EDGE_CURVE('',#10915,#10914,#9622,.T.);
#13366=EDGE_CURVE('',#10907,#10915,#621,.T.);
#13367=EDGE_CURVE('',#10916,#10916,#9623,.T.);
#13368=EDGE_CURVE('',#10916,#10917,#5658,.T.);
#13369=EDGE_CURVE('',#10917,#10917,#9624,.T.);
#13370=EDGE_CURVE('',#10918,#10919,#9625,.T.);
#13371=EDGE_CURVE('',#10920,#10918,#622,.T.);
#13372=EDGE_CURVE('',#10921,#10920,#9626,.T.);
#13373=EDGE_CURVE('',#10922,#10921,#623,.T.);
#13374=EDGE_CURVE('',#10923,#10922,#9627,.T.);
#13375=EDGE_CURVE('',#10923,#10924,#5659,.T.);
#13376=EDGE_CURVE('',#10924,#10924,#9628,.T.);
#13377=EDGE_CURVE('',#10925,#10923,#9629,.T.);
#13378=EDGE_CURVE('',#10926,#10925,#624,.T.);
#13379=EDGE_CURVE('',#10927,#10926,#9630,.T.);
#13380=EDGE_CURVE('',#10919,#10927,#625,.T.);
#13381=EDGE_CURVE('',#10928,#10928,#9631,.T.);
#13382=EDGE_CURVE('',#10928,#10929,#5660,.T.);
#13383=EDGE_CURVE('',#10929,#10929,#9632,.T.);
#13384=EDGE_CURVE('',#10930,#10931,#9633,.T.);
#13385=EDGE_CURVE('',#10932,#10930,#626,.T.);
#13386=EDGE_CURVE('',#10933,#10932,#9634,.T.);
#13387=EDGE_CURVE('',#10934,#10933,#627,.T.);
#13388=EDGE_CURVE('',#10935,#10934,#9635,.T.);
#13389=EDGE_CURVE('',#10935,#10936,#5661,.T.);
#13390=EDGE_CURVE('',#10936,#10936,#9636,.T.);
#13391=EDGE_CURVE('',#10937,#10935,#9637,.T.);
#13392=EDGE_CURVE('',#10938,#10937,#628,.T.);
#13393=EDGE_CURVE('',#10939,#10938,#9638,.T.);
#13394=EDGE_CURVE('',#10931,#10939,#629,.T.);
#13395=EDGE_CURVE('',#10940,#10940,#9639,.T.);
#13396=EDGE_CURVE('',#10940,#10941,#5662,.T.);
#13397=EDGE_CURVE('',#10941,#10941,#9640,.T.);
#13398=EDGE_CURVE('',#10942,#10943,#9641,.T.);
#13399=EDGE_CURVE('',#10944,#10942,#630,.T.);
#13400=EDGE_CURVE('',#10945,#10944,#9642,.T.);
#13401=EDGE_CURVE('',#10946,#10945,#631,.T.);
#13402=EDGE_CURVE('',#10947,#10946,#9643,.T.);
#13403=EDGE_CURVE('',#10947,#10948,#5663,.T.);
#13404=EDGE_CURVE('',#10948,#10948,#9644,.T.);
#13405=EDGE_CURVE('',#10949,#10947,#9645,.T.);
#13406=EDGE_CURVE('',#10950,#10949,#632,.T.);
#13407=EDGE_CURVE('',#10951,#10950,#9646,.T.);
#13408=EDGE_CURVE('',#10943,#10951,#633,.T.);
#13409=EDGE_CURVE('',#10952,#10952,#9647,.T.);
#13410=EDGE_CURVE('',#10952,#10953,#5664,.T.);
#13411=EDGE_CURVE('',#10953,#10953,#9648,.T.);
#13412=EDGE_CURVE('',#10954,#10955,#9649,.T.);
#13413=EDGE_CURVE('',#10956,#10954,#634,.T.);
#13414=EDGE_CURVE('',#10957,#10956,#9650,.T.);
#13415=EDGE_CURVE('',#10958,#10957,#635,.T.);
#13416=EDGE_CURVE('',#10959,#10958,#9651,.T.);
#13417=EDGE_CURVE('',#10959,#10960,#5665,.T.);
#13418=EDGE_CURVE('',#10960,#10960,#9652,.T.);
#13419=EDGE_CURVE('',#10961,#10959,#9653,.T.);
#13420=EDGE_CURVE('',#10962,#10961,#636,.T.);
#13421=EDGE_CURVE('',#10963,#10962,#9654,.T.);
#13422=EDGE_CURVE('',#10955,#10963,#637,.T.);
#13423=EDGE_CURVE('',#10964,#10964,#9655,.T.);
#13424=EDGE_CURVE('',#10964,#10965,#5666,.T.);
#13425=EDGE_CURVE('',#10965,#10965,#9656,.T.);
#13426=EDGE_CURVE('',#10966,#10967,#9657,.T.);
#13427=EDGE_CURVE('',#10968,#10966,#638,.T.);
#13428=EDGE_CURVE('',#10969,#10968,#9658,.T.);
#13429=EDGE_CURVE('',#10970,#10969,#639,.T.);
#13430=EDGE_CURVE('',#10971,#10970,#9659,.T.);
#13431=EDGE_CURVE('',#10971,#10972,#5667,.T.);
#13432=EDGE_CURVE('',#10972,#10972,#9660,.T.);
#13433=EDGE_CURVE('',#10973,#10971,#9661,.T.);
#13434=EDGE_CURVE('',#10974,#10973,#640,.T.);
#13435=EDGE_CURVE('',#10975,#10974,#9662,.T.);
#13436=EDGE_CURVE('',#10967,#10975,#641,.T.);
#13437=EDGE_CURVE('',#10976,#10802,#5668,.T.);
#13438=EDGE_CURVE('',#10977,#10801,#5669,.T.);
#13439=EDGE_CURVE('',#10976,#10977,#5670,.T.);
#13440=EDGE_CURVE('',#10799,#10817,#5671,.T.);
#13441=EDGE_CURVE('',#10807,#10818,#5672,.T.);
#13442=EDGE_CURVE('',#10800,#10813,#5673,.T.);
#13443=EDGE_CURVE('',#10812,#10825,#5674,.T.);
#13444=EDGE_CURVE('',#10824,#10837,#5675,.T.);
#13445=EDGE_CURVE('',#10836,#10849,#5676,.T.);
#13446=EDGE_CURVE('',#10848,#10861,#5677,.T.);
#13447=EDGE_CURVE('',#10860,#10873,#5678,.T.);
#13448=EDGE_CURVE('',#10872,#10885,#5679,.T.);
#13449=EDGE_CURVE('',#10884,#10897,#5680,.T.);
#13450=EDGE_CURVE('',#10896,#10909,#5681,.T.);
#13451=EDGE_CURVE('',#10908,#10921,#5682,.T.);
#13452=EDGE_CURVE('',#10920,#10933,#5683,.T.);
#13453=EDGE_CURVE('',#10932,#10945,#5684,.T.);
#13454=EDGE_CURVE('',#10944,#10957,#5685,.T.);
#13455=EDGE_CURVE('',#10956,#10969,#5686,.T.);
#13456=EDGE_CURVE('',#10968,#10978,#5687,.T.);
#13457=EDGE_CURVE('',#10979,#10978,#5688,.T.);
#13458=EDGE_CURVE('',#10980,#10979,#5689,.T.);
#13459=EDGE_CURVE('',#10980,#10977,#5690,.T.);
#13460=EDGE_CURVE('',#10798,#10814,#5691,.T.);
#13461=EDGE_CURVE('',#10981,#10806,#5692,.T.);
#13462=EDGE_CURVE('',#10981,#10982,#5693,.T.);
#13463=EDGE_CURVE('',#10982,#10983,#5694,.T.);
#13464=EDGE_CURVE('',#10984,#10983,#5695,.T.);
#13465=EDGE_CURVE('',#10975,#10984,#5696,.T.);
#13466=EDGE_CURVE('',#10963,#10974,#5697,.T.);
#13467=EDGE_CURVE('',#10951,#10962,#5698,.T.);
#13468=EDGE_CURVE('',#10939,#10950,#5699,.T.);
#13469=EDGE_CURVE('',#10927,#10938,#5700,.T.);
#13470=EDGE_CURVE('',#10915,#10926,#5701,.T.);
#13471=EDGE_CURVE('',#10903,#10914,#5702,.T.);
#13472=EDGE_CURVE('',#10891,#10902,#5703,.T.);
#13473=EDGE_CURVE('',#10879,#10890,#5704,.T.);
#13474=EDGE_CURVE('',#10867,#10878,#5705,.T.);
#13475=EDGE_CURVE('',#10855,#10866,#5706,.T.);
#13476=EDGE_CURVE('',#10843,#10854,#5707,.T.);
#13477=EDGE_CURVE('',#10831,#10842,#5708,.T.);
#13478=EDGE_CURVE('',#10819,#10830,#5709,.T.);
#13479=EDGE_CURVE('',#10810,#10826,#5710,.T.);
#13480=EDGE_CURVE('',#10811,#10829,#5711,.T.);
#13481=EDGE_CURVE('',#10822,#10838,#5712,.T.);
#13482=EDGE_CURVE('',#10823,#10841,#5713,.T.);
#13483=EDGE_CURVE('',#10834,#10850,#5714,.T.);
#13484=EDGE_CURVE('',#10835,#10853,#5715,.T.);
#13485=EDGE_CURVE('',#10846,#10862,#5716,.T.);
#13486=EDGE_CURVE('',#10847,#10865,#5717,.T.);
#13487=EDGE_CURVE('',#10858,#10874,#5718,.T.);
#13488=EDGE_CURVE('',#10859,#10877,#5719,.T.);
#13489=EDGE_CURVE('',#10870,#10886,#5720,.T.);
#13490=EDGE_CURVE('',#10871,#10889,#5721,.T.);
#13491=EDGE_CURVE('',#10882,#10898,#5722,.T.);
#13492=EDGE_CURVE('',#10883,#10901,#5723,.T.);
#13493=EDGE_CURVE('',#10894,#10910,#5724,.T.);
#13494=EDGE_CURVE('',#10895,#10913,#5725,.T.);
#13495=EDGE_CURVE('',#10906,#10922,#5726,.T.);
#13496=EDGE_CURVE('',#10907,#10925,#5727,.T.);
#13497=EDGE_CURVE('',#10918,#10934,#5728,.T.);
#13498=EDGE_CURVE('',#10919,#10937,#5729,.T.);
#13499=EDGE_CURVE('',#10930,#10946,#5730,.T.);
#13500=EDGE_CURVE('',#10931,#10949,#5731,.T.);
#13501=EDGE_CURVE('',#10942,#10958,#5732,.T.);
#13502=EDGE_CURVE('',#10943,#10961,#5733,.T.);
#13503=EDGE_CURVE('',#10954,#10970,#5734,.T.);
#13504=EDGE_CURVE('',#10955,#10973,#5735,.T.);
#13505=EDGE_CURVE('',#10966,#10985,#5736,.T.);
#13506=EDGE_CURVE('',#10967,#10986,#5737,.T.);
#13507=EDGE_CURVE('',#10986,#10985,#5738,.T.);
#13508=EDGE_CURVE('',#10984,#10986,#5739,.T.);
#13509=EDGE_CURVE('',#10987,#10980,#5740,.T.);
#13510=EDGE_CURVE('',#10988,#10987,#5741,.T.);
#13511=EDGE_CURVE('',#10988,#10989,#9663,.T.);
#13512=EDGE_CURVE('',#10990,#10989,#5742,.T.);
#13513=EDGE_CURVE('',#10990,#10991,#9664,.T.);
#13514=EDGE_CURVE('',#10992,#10991,#5743,.T.);
#13515=EDGE_CURVE('',#10992,#10993,#9665,.T.);
#13516=EDGE_CURVE('',#10994,#10993,#5744,.T.);
#13517=EDGE_CURVE('',#10994,#10995,#9666,.T.);
#13518=EDGE_CURVE('',#10995,#10996,#9667,.T.);
#13519=EDGE_CURVE('',#10996,#10997,#9668,.T.);
#13520=EDGE_CURVE('',#10998,#10997,#5745,.T.);
#13521=EDGE_CURVE('',#10998,#10999,#9669,.T.);
#13522=EDGE_CURVE('',#11000,#10999,#5746,.T.);
#13523=EDGE_CURVE('',#11000,#11001,#9670,.T.);
#13524=EDGE_CURVE('',#11002,#11001,#5747,.T.);
#13525=EDGE_CURVE('',#11002,#11003,#9671,.T.);
#13526=EDGE_CURVE('',#11003,#11004,#9672,.T.);
#13527=EDGE_CURVE('',#11004,#11005,#9673,.T.);
#13528=EDGE_CURVE('',#11006,#11005,#5748,.T.);
#13529=EDGE_CURVE('',#11007,#11006,#5749,.T.);
#13530=EDGE_CURVE('',#11007,#11008,#5750,.T.);
#13531=EDGE_CURVE('',#11008,#11009,#9674,.T.);
#13532=EDGE_CURVE('',#11010,#11009,#9675,.T.);
#13533=EDGE_CURVE('',#11010,#11011,#9676,.T.);
#13534=EDGE_CURVE('',#11011,#11012,#5751,.T.);
#13535=EDGE_CURVE('',#11012,#11013,#9677,.T.);
#13536=EDGE_CURVE('',#11013,#11014,#5752,.T.);
#13537=EDGE_CURVE('',#11014,#11015,#9678,.T.);
#13538=EDGE_CURVE('',#11015,#11016,#5753,.T.);
#13539=EDGE_CURVE('',#11016,#11017,#9679,.T.);
#13540=EDGE_CURVE('',#11018,#11017,#9680,.T.);
#13541=EDGE_CURVE('',#11018,#11019,#9681,.T.);
#13542=EDGE_CURVE('',#11019,#11020,#5754,.T.);
#13543=EDGE_CURVE('',#11020,#11021,#9682,.T.);
#13544=EDGE_CURVE('',#11021,#11022,#5755,.T.);
#13545=EDGE_CURVE('',#11022,#11023,#9683,.T.);
#13546=EDGE_CURVE('',#11023,#11024,#5756,.T.);
#13547=EDGE_CURVE('',#11024,#11025,#9684,.T.);
#13548=EDGE_CURVE('',#11025,#11026,#5757,.T.);
#13549=EDGE_CURVE('',#11026,#10982,#5758,.T.);
#13550=EDGE_CURVE('',#10981,#11027,#5759,.T.);
#13551=EDGE_CURVE('',#11027,#10976,#5760,.T.);
#13552=EDGE_CURVE('',#10985,#10978,#5761,.T.);
#13553=EDGE_CURVE('',#11028,#10983,#5762,.T.);
#13554=EDGE_CURVE('',#11029,#11028,#5763,.T.);
#13555=EDGE_CURVE('',#11029,#11030,#9685,.T.);
#13556=EDGE_CURVE('',#11031,#11030,#5764,.T.);
#13557=EDGE_CURVE('',#11031,#11032,#9686,.T.);
#13558=EDGE_CURVE('',#11033,#11032,#5765,.T.);
#13559=EDGE_CURVE('',#11033,#11034,#9687,.T.);
#13560=EDGE_CURVE('',#11035,#11034,#5766,.T.);
#13561=EDGE_CURVE('',#11035,#11036,#9688,.T.);
#13562=EDGE_CURVE('',#11036,#11037,#9689,.T.);
#13563=EDGE_CURVE('',#11037,#11038,#9690,.T.);
#13564=EDGE_CURVE('',#11039,#11038,#5767,.T.);
#13565=EDGE_CURVE('',#11039,#11040,#9691,.T.);
#13566=EDGE_CURVE('',#11041,#11040,#5768,.T.);
#13567=EDGE_CURVE('',#11041,#11042,#9692,.T.);
#13568=EDGE_CURVE('',#11043,#11042,#5769,.T.);
#13569=EDGE_CURVE('',#11043,#11044,#9693,.T.);
#13570=EDGE_CURVE('',#11044,#11045,#9694,.T.);
#13571=EDGE_CURVE('',#11045,#11046,#9695,.T.);
#13572=EDGE_CURVE('',#11047,#11046,#5770,.T.);
#13573=EDGE_CURVE('',#11047,#11048,#5771,.T.);
#13574=EDGE_CURVE('',#11048,#11049,#5772,.T.);
#13575=EDGE_CURVE('',#11049,#11050,#9696,.T.);
#13576=EDGE_CURVE('',#11051,#11050,#9697,.T.);
#13577=EDGE_CURVE('',#11051,#11052,#9698,.T.);
#13578=EDGE_CURVE('',#11052,#11053,#5773,.T.);
#13579=EDGE_CURVE('',#11053,#11054,#9699,.T.);
#13580=EDGE_CURVE('',#11054,#11055,#5774,.T.);
#13581=EDGE_CURVE('',#11055,#11056,#9700,.T.);
#13582=EDGE_CURVE('',#11056,#11057,#5775,.T.);
#13583=EDGE_CURVE('',#11057,#11058,#9701,.T.);
#13584=EDGE_CURVE('',#11059,#11058,#9702,.T.);
#13585=EDGE_CURVE('',#11059,#11060,#9703,.T.);
#13586=EDGE_CURVE('',#11060,#11061,#5776,.T.);
#13587=EDGE_CURVE('',#11061,#11062,#9704,.T.);
#13588=EDGE_CURVE('',#11062,#11063,#5777,.T.);
#13589=EDGE_CURVE('',#11063,#11064,#9705,.T.);
#13590=EDGE_CURVE('',#11064,#11065,#5778,.T.);
#13591=EDGE_CURVE('',#11065,#11066,#9706,.T.);
#13592=EDGE_CURVE('',#11066,#11067,#5779,.T.);
#13593=EDGE_CURVE('',#11067,#10979,#5780,.T.);
#13594=EDGE_CURVE('',#11034,#11020,#5781,.T.);
#13595=EDGE_CURVE('',#11019,#11035,#5782,.T.);
#13596=EDGE_CURVE('',#11015,#11039,#5783,.T.);
#13597=EDGE_CURVE('',#11038,#11016,#5784,.T.);
#13598=EDGE_CURVE('',#11011,#11043,#5785,.T.);
#13599=EDGE_CURVE('',#11042,#11012,#5786,.T.);
#13600=EDGE_CURVE('',#11046,#11008,#5787,.T.);
#13601=EDGE_CURVE('',#11007,#11047,#5788,.T.);
#13602=EDGE_CURVE('',#10993,#11061,#5789,.T.);
#13603=EDGE_CURVE('',#11060,#10994,#5790,.T.);
#13604=EDGE_CURVE('',#11052,#11002,#5791,.T.);
#13605=EDGE_CURVE('',#11001,#11053,#5792,.T.);
#13606=EDGE_CURVE('',#11006,#11048,#5793,.T.);
#13607=EDGE_CURVE('',#10987,#11067,#5794,.T.);
#13608=EDGE_CURVE('',#11066,#10988,#5795,.T.);
#13609=EDGE_CURVE('',#10989,#11065,#5796,.T.);
#13610=EDGE_CURVE('',#11064,#10990,#5797,.T.);
#13611=EDGE_CURVE('',#10991,#11063,#5798,.T.);
#13612=EDGE_CURVE('',#11062,#10992,#5799,.T.);
#13613=EDGE_CURVE('',#11056,#10998,#5800,.T.);
#13614=EDGE_CURVE('',#10997,#11057,#5801,.T.);
#13615=EDGE_CURVE('',#11054,#11000,#5802,.T.);
#13616=EDGE_CURVE('',#10999,#11055,#5803,.T.);
#13617=EDGE_CURVE('',#11005,#11049,#5804,.T.);
#13618=EDGE_CURVE('',#11003,#11051,#5805,.T.);
#13619=EDGE_CURVE('',#11050,#11004,#5806,.T.);
#13620=EDGE_CURVE('',#11058,#10996,#5807,.T.);
#13621=EDGE_CURVE('',#10995,#11059,#5808,.T.);
#13622=EDGE_CURVE('',#11013,#11041,#5809,.T.);
#13623=EDGE_CURVE('',#11040,#11014,#5810,.T.);
#13624=EDGE_CURVE('',#11032,#11022,#5811,.T.);
#13625=EDGE_CURVE('',#11021,#11033,#5812,.T.);
#13626=EDGE_CURVE('',#11030,#11024,#5813,.T.);
#13627=EDGE_CURVE('',#11023,#11031,#5814,.T.);
#13628=EDGE_CURVE('',#11025,#11029,#5815,.T.);
#13629=EDGE_CURVE('',#11026,#11028,#5816,.T.);
#13630=EDGE_CURVE('',#11044,#11010,#5817,.T.);
#13631=EDGE_CURVE('',#11009,#11045,#5818,.T.);
#13632=EDGE_CURVE('',#11017,#11037,#5819,.T.);
#13633=EDGE_CURVE('',#11036,#11018,#5820,.T.);
#13634=EDGE_CURVE('',#11027,#10805,#5821,.T.);
#13635=EDGE_CURVE('',#11068,#11068,#9707,.T.);
#13636=EDGE_CURVE('',#11068,#11069,#5822,.T.);
#13637=EDGE_CURVE('',#11069,#11069,#9708,.T.);
#13638=EDGE_CURVE('',#11070,#11070,#9709,.T.);
#13639=EDGE_CURVE('',#11070,#11071,#5823,.T.);
#13640=EDGE_CURVE('',#11071,#11071,#9710,.T.);
#13641=EDGE_CURVE('',#11072,#11072,#9711,.T.);
#13642=EDGE_CURVE('',#11072,#11073,#5824,.T.);
#13643=EDGE_CURVE('',#11073,#11073,#9712,.T.);
#13644=EDGE_CURVE('',#11074,#11068,#5825,.T.);
#13645=EDGE_CURVE('',#11075,#11070,#5826,.T.);
#13646=EDGE_CURVE('',#11076,#11076,#9713,.T.);
#13647=EDGE_CURVE('',#11076,#11077,#5827,.T.);
#13648=EDGE_CURVE('',#11077,#11077,#9714,.T.);
#13649=EDGE_CURVE('',#11078,#11078,#9715,.T.);
#13650=EDGE_CURVE('',#11078,#11079,#5828,.T.);
#13651=EDGE_CURVE('',#11079,#11079,#9716,.T.);
#13652=EDGE_CURVE('',#11080,#11080,#9717,.T.);
#13653=EDGE_CURVE('',#11080,#11081,#5829,.T.);
#13654=EDGE_CURVE('',#11081,#11081,#9718,.T.);
#13655=EDGE_CURVE('',#11082,#11082,#9719,.T.);
#13656=EDGE_CURVE('',#11082,#11083,#5830,.T.);
#13657=EDGE_CURVE('',#11083,#11083,#9720,.T.);
#13658=EDGE_CURVE('',#11084,#11084,#9721,.T.);
#13659=EDGE_CURVE('',#11084,#11085,#5831,.T.);
#13660=EDGE_CURVE('',#11085,#11085,#9722,.T.);
#13661=EDGE_CURVE('',#11086,#11086,#9723,.T.);
#13662=EDGE_CURVE('',#11086,#11087,#5832,.T.);
#13663=EDGE_CURVE('',#11087,#11087,#9724,.T.);
#13664=EDGE_CURVE('',#11088,#11088,#9725,.T.);
#13665=EDGE_CURVE('',#11088,#11089,#5833,.T.);
#13666=EDGE_CURVE('',#11089,#11089,#9726,.T.);
#13667=EDGE_CURVE('',#11090,#11090,#9727,.T.);
#13668=EDGE_CURVE('',#11090,#11091,#5834,.T.);
#13669=EDGE_CURVE('',#11091,#11092,#9728,.T.);
#13670=EDGE_CURVE('',#11092,#11093,#5835,.T.);
#13671=EDGE_CURVE('',#11093,#11094,#9729,.T.);
#13672=EDGE_CURVE('',#11091,#11094,#5836,.T.);
#13673=EDGE_CURVE('',#11095,#11084,#5837,.T.);
#13674=EDGE_CURVE('',#11096,#11086,#5838,.T.);
#13675=EDGE_CURVE('',#11097,#11097,#9730,.T.);
#13676=EDGE_CURVE('',#11097,#11098,#5839,.T.);
#13677=EDGE_CURVE('',#11098,#11099,#5840,.T.);
#13678=EDGE_CURVE('',#11099,#11100,#9731,.T.);
#13679=EDGE_CURVE('',#11101,#11100,#5841,.T.);
#13680=EDGE_CURVE('',#11101,#11098,#9732,.T.);
#13681=EDGE_CURVE('',#11102,#11103,#109,.T.);
#13682=EDGE_CURVE('',#11104,#11102,#110,.T.);
#13683=EDGE_CURVE('',#11105,#11104,#111,.T.);
#13684=EDGE_CURVE('',#11105,#11106,#82,.T.);
#13685=EDGE_CURVE('',#11107,#11106,#9733,.T.);
#13686=EDGE_CURVE('',#11106,#11107,#9734,.T.);
#13687=EDGE_CURVE('',#11108,#11105,#112,.T.);
#13688=EDGE_CURVE('',#11109,#11108,#113,.T.);
#13689=EDGE_CURVE('',#11103,#11109,#114,.T.);
#13690=EDGE_CURVE('',#11110,#11110,#9735,.T.);
#13691=EDGE_CURVE('',#11110,#11107,#5842,.T.);
#13692=EDGE_CURVE('',#11111,#11111,#9736,.T.);
#13693=EDGE_CURVE('',#11111,#11112,#5843,.T.);
#13694=EDGE_CURVE('',#11112,#11112,#9737,.T.);
#13695=EDGE_CURVE('',#11113,#11114,#642,.T.);
#13696=EDGE_CURVE('',#11115,#11113,#5844,.T.);
#13697=EDGE_CURVE('',#11115,#11116,#5845,.T.);
#13698=EDGE_CURVE('',#11116,#11114,#5846,.T.);
#13699=EDGE_CURVE('',#11117,#11113,#643,.T.);
#13700=EDGE_CURVE('',#11117,#11118,#5847,.T.);
#13701=EDGE_CURVE('',#11119,#11118,#644,.T.);
#13702=EDGE_CURVE('',#11113,#11119,#5848,.T.);
#13703=EDGE_CURVE('',#11120,#11121,#645,.T.);
#13704=EDGE_CURVE('',#11120,#11122,#5849,.T.);
#13705=EDGE_CURVE('',#11123,#11122,#646,.T.);
#13706=EDGE_CURVE('',#11121,#11123,#5850,.T.);
#13707=EDGE_CURVE('',#11122,#11124,#647,.T.);
#13708=EDGE_CURVE('',#11122,#11125,#5851,.T.);
#13709=EDGE_CURVE('',#11126,#11125,#5852,.T.);
#13710=EDGE_CURVE('',#11124,#11126,#5853,.T.);
#13711=EDGE_CURVE('',#11127,#11128,#5854,.T.);
#13712=EDGE_CURVE('',#11127,#11129,#5855,.T.);
#13713=EDGE_CURVE('',#11129,#11130,#5856,.T.);
#13714=EDGE_CURVE('',#11130,#11128,#5857,.T.);
#13715=EDGE_CURVE('',#11131,#11132,#5858,.T.);
#13716=EDGE_CURVE('',#11131,#11133,#5859,.T.);
#13717=EDGE_CURVE('',#11133,#11134,#5860,.T.);
#13718=EDGE_CURVE('',#11134,#11132,#5861,.T.);
#13719=EDGE_CURVE('',#11135,#11136,#5862,.T.);
#13720=EDGE_CURVE('',#11135,#11137,#5863,.T.);
#13721=EDGE_CURVE('',#11137,#11138,#5864,.T.);
#13722=EDGE_CURVE('',#11138,#11136,#5865,.T.);
#13723=EDGE_CURVE('',#11139,#11140,#5866,.T.);
#13724=EDGE_CURVE('',#11139,#11141,#5867,.T.);
#13725=EDGE_CURVE('',#11141,#11142,#5868,.T.);
#13726=EDGE_CURVE('',#11142,#11140,#5869,.T.);
#13727=EDGE_CURVE('',#11143,#11144,#5870,.T.);
#13728=EDGE_CURVE('',#11143,#11145,#5871,.T.);
#13729=EDGE_CURVE('',#11145,#11146,#5872,.T.);
#13730=EDGE_CURVE('',#11146,#11144,#5873,.T.);
#13731=EDGE_CURVE('',#11147,#11148,#5874,.T.);
#13732=EDGE_CURVE('',#11147,#11149,#5875,.T.);
#13733=EDGE_CURVE('',#11149,#11150,#5876,.T.);
#13734=EDGE_CURVE('',#11150,#11148,#5877,.T.);
#13735=EDGE_CURVE('',#11151,#11152,#5878,.T.);
#13736=EDGE_CURVE('',#11151,#11153,#5879,.T.);
#13737=EDGE_CURVE('',#11153,#11154,#5880,.T.);
#13738=EDGE_CURVE('',#11154,#11152,#5881,.T.);
#13739=EDGE_CURVE('',#11155,#11156,#5882,.T.);
#13740=EDGE_CURVE('',#11155,#11157,#5883,.T.);
#13741=EDGE_CURVE('',#11157,#11158,#5884,.T.);
#13742=EDGE_CURVE('',#11158,#11156,#5885,.T.);
#13743=EDGE_CURVE('',#11159,#11160,#5886,.T.);
#13744=EDGE_CURVE('',#11161,#11159,#5887,.T.);
#13745=EDGE_CURVE('',#11161,#11162,#5888,.T.);
#13746=EDGE_CURVE('',#11162,#11160,#5889,.T.);
#13747=EDGE_CURVE('',#11163,#11159,#5890,.T.);
#13748=EDGE_CURVE('',#11164,#11163,#5891,.T.);
#13749=EDGE_CURVE('',#11164,#11161,#5892,.T.);
#13750=EDGE_CURVE('',#11165,#11166,#5893,.T.);
#13751=EDGE_CURVE('',#11167,#11165,#5894,.T.);
#13752=EDGE_CURVE('',#11167,#11168,#5895,.T.);
#13753=EDGE_CURVE('',#11168,#11166,#5896,.T.);
#13754=EDGE_CURVE('',#11169,#11165,#5897,.T.);
#13755=EDGE_CURVE('',#11169,#11170,#5898,.T.);
#13756=EDGE_CURVE('',#11170,#11167,#5899,.T.);
#13757=EDGE_CURVE('',#11171,#11172,#5900,.T.);
#13758=EDGE_CURVE('',#11171,#11173,#5901,.T.);
#13759=EDGE_CURVE('',#11173,#11174,#5902,.T.);
#13760=EDGE_CURVE('',#11174,#11172,#5903,.T.);
#13761=EDGE_CURVE('',#11175,#11176,#5904,.T.);
#13762=EDGE_CURVE('',#11175,#11177,#5905,.T.);
#13763=EDGE_CURVE('',#11177,#11178,#5906,.T.);
#13764=EDGE_CURVE('',#11178,#11176,#5907,.T.);
#13765=EDGE_CURVE('',#11179,#11180,#5908,.T.);
#13766=EDGE_CURVE('',#11179,#11181,#5909,.T.);
#13767=EDGE_CURVE('',#11181,#11182,#5910,.T.);
#13768=EDGE_CURVE('',#11182,#11180,#5911,.T.);
#13769=EDGE_CURVE('',#11183,#11184,#5912,.T.);
#13770=EDGE_CURVE('',#11185,#11183,#5913,.T.);
#13771=EDGE_CURVE('',#11185,#11186,#5914,.T.);
#13772=EDGE_CURVE('',#11186,#11184,#5915,.T.);
#13773=EDGE_CURVE('',#11140,#11183,#5916,.T.);
#13774=EDGE_CURVE('',#11142,#11185,#5917,.T.);
#13775=EDGE_CURVE('',#11187,#11188,#9738,.T.);
#13776=EDGE_CURVE('',#11187,#11189,#5918,.T.);
#13777=EDGE_CURVE('',#11189,#11190,#9739,.T.);
#13778=EDGE_CURVE('',#11190,#11188,#5919,.T.);
#13779=EDGE_CURVE('',#11191,#11192,#9740,.T.);
#13780=EDGE_CURVE('',#11191,#11193,#5920,.T.);
#13781=EDGE_CURVE('',#11193,#11194,#9741,.T.);
#13782=EDGE_CURVE('',#11194,#11192,#5921,.T.);
#13783=EDGE_CURVE('',#11195,#11196,#9742,.T.);
#13784=EDGE_CURVE('',#11195,#11197,#5922,.T.);
#13785=EDGE_CURVE('',#11197,#11198,#9743,.T.);
#13786=EDGE_CURVE('',#11198,#11196,#5923,.T.);
#13787=EDGE_CURVE('',#11199,#11200,#9744,.T.);
#13788=EDGE_CURVE('',#11199,#11201,#5924,.T.);
#13789=EDGE_CURVE('',#11201,#11202,#9745,.T.);
#13790=EDGE_CURVE('',#11202,#11200,#5925,.T.);
#13791=EDGE_CURVE('',#11172,#11169,#9746,.T.);
#13792=EDGE_CURVE('',#11170,#11174,#9747,.T.);
#13793=EDGE_CURVE('',#11160,#11155,#9748,.T.);
#13794=EDGE_CURVE('',#11157,#11162,#9749,.T.);
#13795=EDGE_CURVE('',#11180,#11175,#9750,.T.);
#13796=EDGE_CURVE('',#11177,#11182,#9751,.T.);
#13797=EDGE_CURVE('',#11132,#11179,#9752,.T.);
#13798=EDGE_CURVE('',#11181,#11134,#9753,.T.);
#13799=EDGE_CURVE('',#11196,#11131,#9754,.T.);
#13800=EDGE_CURVE('',#11133,#11198,#9755,.T.);
#13801=EDGE_CURVE('',#11184,#11195,#9756,.T.);
#13802=EDGE_CURVE('',#11197,#11186,#9757,.T.);
#13803=EDGE_CURVE('',#11176,#11199,#9758,.T.);
#13804=EDGE_CURVE('',#11201,#11178,#9759,.T.);
#13805=EDGE_CURVE('',#11200,#11127,#9760,.T.);
#13806=EDGE_CURVE('',#11129,#11202,#9761,.T.);
#13807=EDGE_CURVE('',#11128,#11171,#9762,.T.);
#13808=EDGE_CURVE('',#11173,#11130,#9763,.T.);
#13809=EDGE_CURVE('',#11156,#11151,#9764,.T.);
#13810=EDGE_CURVE('',#11153,#11158,#9765,.T.);
#13811=EDGE_CURVE('',#11152,#11191,#9766,.T.);
#13812=EDGE_CURVE('',#11193,#11154,#9767,.T.);
#13813=EDGE_CURVE('',#11192,#11135,#9768,.T.);
#13814=EDGE_CURVE('',#11137,#11194,#9769,.T.);
#13815=EDGE_CURVE('',#11136,#11147,#9770,.T.);
#13816=EDGE_CURVE('',#11149,#11138,#9771,.T.);
#13817=EDGE_CURVE('',#11148,#11143,#9772,.T.);
#13818=EDGE_CURVE('',#11145,#11150,#9773,.T.);
#13819=EDGE_CURVE('',#11144,#11187,#9774,.T.);
#13820=EDGE_CURVE('',#11189,#11146,#9775,.T.);
#13821=EDGE_CURVE('',#11188,#11139,#9776,.T.);
#13822=EDGE_CURVE('',#11141,#11190,#9777,.T.);
#13823=EDGE_CURVE('',#11203,#11204,#5926,.T.);
#13824=EDGE_CURVE('',#11205,#11204,#5927,.T.);
#13825=EDGE_CURVE('',#11206,#11205,#5928,.T.);
#13826=EDGE_CURVE('',#11203,#11206,#5929,.T.);
#13827=EDGE_CURVE('',#11164,#11207,#5930,.T.);
#13828=EDGE_CURVE('',#11207,#11208,#5931,.T.);
#13829=EDGE_CURVE('',#11208,#11203,#5932,.T.);
#13830=EDGE_CURVE('',#11206,#11209,#5933,.T.);
#13831=EDGE_CURVE('',#11209,#11210,#5934,.T.);
#13832=EDGE_CURVE('',#11210,#11168,#5935,.T.);
#13833=EDGE_CURVE('',#11208,#11211,#5936,.T.);
#13834=EDGE_CURVE('',#11204,#11211,#5937,.T.);
#13835=EDGE_CURVE('',#11207,#11212,#5938,.T.);
#13836=EDGE_CURVE('',#11211,#11212,#5939,.T.);
#13837=EDGE_CURVE('',#11212,#11163,#5940,.T.);
#13838=EDGE_CURVE('',#11210,#11213,#5941,.T.);
#13839=EDGE_CURVE('',#11166,#11213,#5942,.T.);
#13840=EDGE_CURVE('',#11209,#11214,#5943,.T.);
#13841=EDGE_CURVE('',#11213,#11214,#5944,.T.);
#13842=EDGE_CURVE('',#11214,#11205,#5945,.T.);
#13843=EDGE_CURVE('',#11215,#11103,#5946,.T.);
#13844=EDGE_CURVE('',#11216,#11109,#5947,.T.);
#13845=EDGE_CURVE('',#11215,#11216,#5948,.T.);
#13846=EDGE_CURVE('',#11217,#11215,#5949,.T.);
#13847=EDGE_CURVE('',#11217,#11102,#5950,.T.);
#13848=EDGE_CURVE('',#11218,#11104,#5951,.T.);
#13849=EDGE_CURVE('',#11218,#11217,#5952,.T.);
#13850=EDGE_CURVE('',#11219,#11105,#5953,.T.);
#13851=EDGE_CURVE('',#11219,#11218,#5954,.T.);
#13852=EDGE_CURVE('',#11220,#11108,#5955,.T.);
#13853=EDGE_CURVE('',#11220,#11219,#5956,.T.);
#13854=EDGE_CURVE('',#11216,#11220,#5957,.T.);
#13855=EDGE_CURVE('',#11221,#11222,#5958,.T.);
#13856=EDGE_CURVE('',#11223,#11221,#9778,.T.);
#13857=EDGE_CURVE('',#11224,#11223,#5959,.T.);
#13858=EDGE_CURVE('',#11225,#11224,#9779,.T.);
#13859=EDGE_CURVE('',#11226,#11225,#5960,.T.);
#13860=EDGE_CURVE('',#11227,#11226,#9780,.T.);
#13861=EDGE_CURVE('',#11228,#11227,#9781,.T.);
#13862=EDGE_CURVE('',#11229,#11228,#9782,.T.);
#13863=EDGE_CURVE('',#11230,#11229,#5961,.T.);
#13864=EDGE_CURVE('',#11231,#11230,#9783,.T.);
#13865=EDGE_CURVE('',#11232,#11231,#5962,.T.);
#13866=EDGE_CURVE('',#11233,#11232,#9784,.T.);
#13867=EDGE_CURVE('',#11234,#11233,#5963,.T.);
#13868=EDGE_CURVE('',#11235,#11234,#9785,.T.);
#13869=EDGE_CURVE('',#11236,#11235,#9786,.T.);
#13870=EDGE_CURVE('',#11237,#11236,#9787,.T.);
#13871=EDGE_CURVE('',#11238,#11237,#5964,.T.);
#13872=EDGE_CURVE('',#11239,#11238,#5965,.T.);
#13873=EDGE_CURVE('',#11240,#11239,#5966,.T.);
#13874=EDGE_CURVE('',#11241,#11240,#9788,.T.);
#13875=EDGE_CURVE('',#11242,#11241,#9789,.T.);
#13876=EDGE_CURVE('',#11243,#11242,#9790,.T.);
#13877=EDGE_CURVE('',#11244,#11243,#5967,.T.);
#13878=EDGE_CURVE('',#11245,#11244,#9791,.T.);
#13879=EDGE_CURVE('',#11246,#11245,#5968,.T.);
#13880=EDGE_CURVE('',#11247,#11246,#9792,.T.);
#13881=EDGE_CURVE('',#11248,#11247,#5969,.T.);
#13882=EDGE_CURVE('',#11249,#11248,#9793,.T.);
#13883=EDGE_CURVE('',#11250,#11249,#9794,.T.);
#13884=EDGE_CURVE('',#11251,#11250,#9795,.T.);
#13885=EDGE_CURVE('',#11252,#11251,#5970,.T.);
#13886=EDGE_CURVE('',#11253,#11252,#9796,.T.);
#13887=EDGE_CURVE('',#11254,#11253,#5971,.T.);
#13888=EDGE_CURVE('',#11255,#11254,#9797,.T.);
#13889=EDGE_CURVE('',#11256,#11255,#5972,.T.);
#13890=EDGE_CURVE('',#11257,#11256,#5973,.T.);
#13891=EDGE_CURVE('',#11258,#11257,#5974,.T.);
#13892=EDGE_CURVE('',#11259,#11258,#5975,.T.);
#13893=EDGE_CURVE('',#11260,#11259,#5976,.T.);
#13894=EDGE_CURVE('',#11261,#11260,#5977,.T.);
#13895=EDGE_CURVE('',#11262,#11261,#5978,.T.);
#13896=EDGE_CURVE('',#11263,#11262,#5979,.T.);
#13897=EDGE_CURVE('',#11264,#11263,#5980,.T.);
#13898=EDGE_CURVE('',#11222,#11264,#5981,.T.);
#13899=EDGE_CURVE('',#11265,#11266,#5982,.T.);
#13900=EDGE_CURVE('',#11221,#11265,#5983,.T.);
#13901=EDGE_CURVE('',#11222,#11266,#5984,.T.);
#13902=EDGE_CURVE('',#11267,#11265,#9798,.T.);
#13903=EDGE_CURVE('',#11223,#11267,#5985,.T.);
#13904=EDGE_CURVE('',#11268,#11267,#5986,.T.);
#13905=EDGE_CURVE('',#11224,#11268,#5987,.T.);
#13906=EDGE_CURVE('',#11269,#11268,#9799,.T.);
#13907=EDGE_CURVE('',#11225,#11269,#5988,.T.);
#13908=EDGE_CURVE('',#11270,#11269,#5989,.T.);
#13909=EDGE_CURVE('',#11226,#11270,#5990,.T.);
#13910=EDGE_CURVE('',#11271,#11270,#9800,.T.);
#13911=EDGE_CURVE('',#11227,#11271,#5991,.T.);
#13912=EDGE_CURVE('',#11272,#11271,#9801,.T.);
#13913=EDGE_CURVE('',#11228,#11272,#5992,.T.);
#13914=EDGE_CURVE('',#11273,#11272,#9802,.T.);
#13915=EDGE_CURVE('',#11229,#11273,#5993,.T.);
#13916=EDGE_CURVE('',#11274,#11273,#5994,.T.);
#13917=EDGE_CURVE('',#11230,#11274,#5995,.T.);
#13918=EDGE_CURVE('',#11275,#11274,#9803,.T.);
#13919=EDGE_CURVE('',#11231,#11275,#5996,.T.);
#13920=EDGE_CURVE('',#11276,#11275,#5997,.T.);
#13921=EDGE_CURVE('',#11232,#11276,#5998,.T.);
#13922=EDGE_CURVE('',#11277,#11276,#9804,.T.);
#13923=EDGE_CURVE('',#11233,#11277,#5999,.T.);
#13924=EDGE_CURVE('',#11278,#11277,#6000,.T.);
#13925=EDGE_CURVE('',#11234,#11278,#6001,.T.);
#13926=EDGE_CURVE('',#11279,#11278,#9805,.T.);
#13927=EDGE_CURVE('',#11235,#11279,#6002,.T.);
#13928=EDGE_CURVE('',#11280,#11279,#9806,.T.);
#13929=EDGE_CURVE('',#11236,#11280,#6003,.T.);
#13930=EDGE_CURVE('',#11281,#11280,#9807,.T.);
#13931=EDGE_CURVE('',#11237,#11281,#6004,.T.);
#13932=EDGE_CURVE('',#11282,#11281,#6005,.T.);
#13933=EDGE_CURVE('',#11238,#11282,#6006,.T.);
#13934=EDGE_CURVE('',#11283,#11282,#6007,.T.);
#13935=EDGE_CURVE('',#11239,#11283,#6008,.T.);
#13936=EDGE_CURVE('',#11284,#11283,#6009,.T.);
#13937=EDGE_CURVE('',#11240,#11284,#6010,.T.);
#13938=EDGE_CURVE('',#11285,#11284,#9808,.T.);
#13939=EDGE_CURVE('',#11241,#11285,#6011,.T.);
#13940=EDGE_CURVE('',#11286,#11285,#9809,.T.);
#13941=EDGE_CURVE('',#11242,#11286,#6012,.T.);
#13942=EDGE_CURVE('',#11287,#11286,#9810,.T.);
#13943=EDGE_CURVE('',#11243,#11287,#6013,.T.);
#13944=EDGE_CURVE('',#11288,#11287,#6014,.T.);
#13945=EDGE_CURVE('',#11244,#11288,#6015,.T.);
#13946=EDGE_CURVE('',#11289,#11288,#9811,.T.);
#13947=EDGE_CURVE('',#11245,#11289,#6016,.T.);
#13948=EDGE_CURVE('',#11290,#11289,#6017,.T.);
#13949=EDGE_CURVE('',#11246,#11290,#6018,.T.);
#13950=EDGE_CURVE('',#11291,#11290,#9812,.T.);
#13951=EDGE_CURVE('',#11247,#11291,#6019,.T.);
#13952=EDGE_CURVE('',#11292,#11291,#6020,.T.);
#13953=EDGE_CURVE('',#11248,#11292,#6021,.T.);
#13954=EDGE_CURVE('',#11293,#11292,#9813,.T.);
#13955=EDGE_CURVE('',#11249,#11293,#6022,.T.);
#13956=EDGE_CURVE('',#11294,#11293,#9814,.T.);
#13957=EDGE_CURVE('',#11250,#11294,#6023,.T.);
#13958=EDGE_CURVE('',#11295,#11294,#9815,.T.);
#13959=EDGE_CURVE('',#11251,#11295,#6024,.T.);
#13960=EDGE_CURVE('',#11296,#11295,#6025,.T.);
#13961=EDGE_CURVE('',#11252,#11296,#6026,.T.);
#13962=EDGE_CURVE('',#11297,#11296,#9816,.T.);
#13963=EDGE_CURVE('',#11253,#11297,#6027,.T.);
#13964=EDGE_CURVE('',#11298,#11297,#6028,.T.);
#13965=EDGE_CURVE('',#11254,#11298,#6029,.T.);
#13966=EDGE_CURVE('',#11299,#11298,#9817,.T.);
#13967=EDGE_CURVE('',#11255,#11299,#6030,.T.);
#13968=EDGE_CURVE('',#11300,#11299,#6031,.T.);
#13969=EDGE_CURVE('',#11256,#11300,#6032,.T.);
#13970=EDGE_CURVE('',#11301,#11300,#6033,.T.);
#13971=EDGE_CURVE('',#11257,#11301,#6034,.T.);
#13972=EDGE_CURVE('',#11302,#11301,#6035,.T.);
#13973=EDGE_CURVE('',#11258,#11302,#6036,.T.);
#13974=EDGE_CURVE('',#11303,#11302,#6037,.T.);
#13975=EDGE_CURVE('',#11259,#11303,#6038,.T.);
#13976=EDGE_CURVE('',#11304,#11303,#6039,.T.);
#13977=EDGE_CURVE('',#11260,#11304,#6040,.T.);
#13978=EDGE_CURVE('',#11305,#11304,#6041,.T.);
#13979=EDGE_CURVE('',#11261,#11305,#6042,.T.);
#13980=EDGE_CURVE('',#11306,#11305,#6043,.T.);
#13981=EDGE_CURVE('',#11262,#11306,#6044,.T.);
#13982=EDGE_CURVE('',#11307,#11306,#6045,.T.);
#13983=EDGE_CURVE('',#11263,#11307,#6046,.T.);
#13984=EDGE_CURVE('',#11308,#11307,#6047,.T.);
#13985=EDGE_CURVE('',#11264,#11308,#6048,.T.);
#13986=EDGE_CURVE('',#11266,#11308,#6049,.T.);
#13987=EDGE_CURVE('',#11101,#11309,#6050,.T.);
#13988=EDGE_CURVE('',#11309,#11310,#9818,.T.);
#13989=EDGE_CURVE('',#11310,#11098,#6051,.T.);
#13990=EDGE_CURVE('',#11311,#11312,#6052,.T.);
#13991=EDGE_CURVE('',#11313,#11311,#6053,.T.);
#13992=EDGE_CURVE('',#11314,#11313,#9819,.T.);
#13993=EDGE_CURVE('',#11315,#11314,#6054,.T.);
#13994=EDGE_CURVE('',#11316,#11315,#6055,.T.);
#13995=EDGE_CURVE('',#11317,#11316,#6056,.T.);
#13996=EDGE_CURVE('',#11318,#11317,#6057,.T.);
#13997=EDGE_CURVE('',#11319,#11318,#6058,.T.);
#13998=EDGE_CURVE('',#11319,#11320,#6059,.T.);
#13999=EDGE_CURVE('',#11320,#11321,#6060,.T.);
#14000=EDGE_CURVE('',#11321,#11322,#9820,.T.);
#14001=EDGE_CURVE('',#11322,#11323,#6061,.T.);
#14002=EDGE_CURVE('',#11323,#11324,#9821,.T.);
#14003=EDGE_CURVE('',#11324,#11325,#6062,.T.);
#14004=EDGE_CURVE('',#11325,#11326,#9822,.T.);
#14005=EDGE_CURVE('',#11326,#11327,#9823,.T.);
#14006=EDGE_CURVE('',#11327,#11328,#9824,.T.);
#14007=EDGE_CURVE('',#11328,#11329,#6063,.T.);
#14008=EDGE_CURVE('',#11329,#11330,#9825,.T.);
#14009=EDGE_CURVE('',#11330,#11331,#6064,.T.);
#14010=EDGE_CURVE('',#11331,#11332,#9826,.T.);
#14011=EDGE_CURVE('',#11332,#11333,#6065,.T.);
#14012=EDGE_CURVE('',#11333,#11334,#9827,.T.);
#14013=EDGE_CURVE('',#11334,#11335,#9828,.T.);
#14014=EDGE_CURVE('',#11335,#11336,#9829,.T.);
#14015=EDGE_CURVE('',#11336,#11337,#6066,.T.);
#14016=EDGE_CURVE('',#11337,#11338,#6067,.T.);
#14017=EDGE_CURVE('',#11338,#11339,#6068,.T.);
#14018=EDGE_CURVE('',#11339,#11340,#9830,.T.);
#14019=EDGE_CURVE('',#11340,#11341,#9831,.T.);
#14020=EDGE_CURVE('',#11341,#11342,#9832,.T.);
#14021=EDGE_CURVE('',#11342,#11343,#6069,.T.);
#14022=EDGE_CURVE('',#11343,#11344,#9833,.T.);
#14023=EDGE_CURVE('',#11344,#11345,#6070,.T.);
#14024=EDGE_CURVE('',#11345,#11346,#9834,.T.);
#14025=EDGE_CURVE('',#11346,#11347,#6071,.T.);
#14026=EDGE_CURVE('',#11347,#11348,#9835,.T.);
#14027=EDGE_CURVE('',#11348,#11349,#9836,.T.);
#14028=EDGE_CURVE('',#11349,#11350,#9837,.T.);
#14029=EDGE_CURVE('',#11350,#11351,#6072,.T.);
#14030=EDGE_CURVE('',#11351,#11352,#9838,.T.);
#14031=EDGE_CURVE('',#11352,#11353,#6073,.T.);
#14032=EDGE_CURVE('',#11353,#11354,#9839,.T.);
#14033=EDGE_CURVE('',#11354,#11355,#6074,.T.);
#14034=EDGE_CURVE('',#11355,#11356,#6075,.T.);
#14035=EDGE_CURVE('',#11357,#11356,#6076,.T.);
#14036=EDGE_CURVE('',#11358,#11357,#6077,.T.);
#14037=EDGE_CURVE('',#11312,#11358,#6078,.T.);
#14038=EDGE_CURVE('',#11359,#11099,#6079,.T.);
#14039=EDGE_CURVE('',#11310,#11359,#6080,.T.);
#14040=EDGE_CURVE('',#11100,#11360,#6081,.T.);
#14041=EDGE_CURVE('',#11309,#11360,#6082,.T.);
#14042=EDGE_CURVE('',#11360,#11359,#9840,.T.);
#14043=EDGE_CURVE('',#11091,#11361,#6083,.T.);
#14044=EDGE_CURVE('',#11361,#11362,#9841,.T.);
#14045=EDGE_CURVE('',#11362,#11092,#6084,.T.);
#14046=EDGE_CURVE('',#11363,#11364,#6085,.T.);
#14047=EDGE_CURVE('',#11364,#11356,#6086,.T.);
#14048=EDGE_CURVE('',#11363,#11355,#6087,.T.);
#14049=EDGE_CURVE('',#11364,#11365,#6088,.T.);
#14050=EDGE_CURVE('',#11365,#11357,#6089,.T.);
#14051=EDGE_CURVE('',#11365,#11366,#6090,.T.);
#14052=EDGE_CURVE('',#11366,#11358,#6091,.T.);
#14053=EDGE_CURVE('',#11366,#11367,#6092,.T.);
#14054=EDGE_CURVE('',#11367,#11312,#6093,.T.);
#14055=EDGE_CURVE('',#11368,#11369,#6094,.T.);
#14056=EDGE_CURVE('',#11368,#11311,#6095,.T.);
#14057=EDGE_CURVE('',#11367,#11370,#6096,.T.);
#14058=EDGE_CURVE('',#11370,#11316,#6097,.T.);
#14059=EDGE_CURVE('',#11369,#11315,#6098,.T.);
#14060=EDGE_CURVE('',#11370,#11371,#6099,.T.);
#14061=EDGE_CURVE('',#11371,#11317,#6100,.T.);
#14062=EDGE_CURVE('',#11371,#11372,#6101,.T.);
#14063=EDGE_CURVE('',#11372,#11318,#6102,.T.);
#14064=EDGE_CURVE('',#11372,#11373,#6103,.T.);
#14065=EDGE_CURVE('',#11373,#11319,#6104,.T.);
#14066=EDGE_CURVE('',#11373,#11374,#6105,.T.);
#14067=EDGE_CURVE('',#11374,#11320,#6106,.T.);
#14068=EDGE_CURVE('',#11374,#11375,#6107,.T.);
#14069=EDGE_CURVE('',#11375,#11321,#6108,.T.);
#14070=EDGE_CURVE('',#11375,#11376,#9842,.T.);
#14071=EDGE_CURVE('',#11322,#11376,#6109,.T.);
#14072=EDGE_CURVE('',#11376,#11377,#6110,.T.);
#14073=EDGE_CURVE('',#11377,#11323,#6111,.T.);
#14074=EDGE_CURVE('',#11377,#11378,#9843,.T.);
#14075=EDGE_CURVE('',#11324,#11378,#6112,.T.);
#14076=EDGE_CURVE('',#11378,#11379,#6113,.T.);
#14077=EDGE_CURVE('',#11379,#11325,#6114,.T.);
#14078=EDGE_CURVE('',#11379,#11380,#9844,.T.);
#14079=EDGE_CURVE('',#11326,#11380,#6115,.T.);
#14080=EDGE_CURVE('',#11380,#11381,#9845,.T.);
#14081=EDGE_CURVE('',#11381,#11327,#6116,.T.);
#14082=EDGE_CURVE('',#11381,#11382,#9846,.T.);
#14083=EDGE_CURVE('',#11328,#11382,#6117,.T.);
#14084=EDGE_CURVE('',#11382,#11383,#6118,.T.);
#14085=EDGE_CURVE('',#11383,#11329,#6119,.T.);
#14086=EDGE_CURVE('',#11383,#11384,#9847,.T.);
#14087=EDGE_CURVE('',#11330,#11384,#6120,.T.);
#14088=EDGE_CURVE('',#11384,#11385,#6121,.T.);
#14089=EDGE_CURVE('',#11385,#11331,#6122,.T.);
#14090=EDGE_CURVE('',#11385,#11386,#9848,.T.);
#14091=EDGE_CURVE('',#11332,#11386,#6123,.T.);
#14092=EDGE_CURVE('',#11386,#11387,#6124,.T.);
#14093=EDGE_CURVE('',#11387,#11333,#6125,.T.);
#14094=EDGE_CURVE('',#11387,#11388,#9849,.T.);
#14095=EDGE_CURVE('',#11334,#11388,#6126,.T.);
#14096=EDGE_CURVE('',#11388,#11389,#9850,.T.);
#14097=EDGE_CURVE('',#11389,#11335,#6127,.T.);
#14098=EDGE_CURVE('',#11389,#11390,#9851,.T.);
#14099=EDGE_CURVE('',#11336,#11390,#6128,.T.);
#14100=EDGE_CURVE('',#11390,#11391,#6129,.T.);
#14101=EDGE_CURVE('',#11391,#11337,#6130,.T.);
#14102=EDGE_CURVE('',#11391,#11392,#6131,.T.);
#14103=EDGE_CURVE('',#11392,#11338,#6132,.T.);
#14104=EDGE_CURVE('',#11392,#11393,#6133,.T.);
#14105=EDGE_CURVE('',#11393,#11339,#6134,.T.);
#14106=EDGE_CURVE('',#11393,#11394,#9852,.T.);
#14107=EDGE_CURVE('',#11340,#11394,#6135,.T.);
#14108=EDGE_CURVE('',#11394,#11395,#9853,.T.);
#14109=EDGE_CURVE('',#11395,#11341,#6136,.T.);
#14110=EDGE_CURVE('',#11395,#11396,#9854,.T.);
#14111=EDGE_CURVE('',#11342,#11396,#6137,.T.);
#14112=EDGE_CURVE('',#11396,#11397,#6138,.T.);
#14113=EDGE_CURVE('',#11397,#11343,#6139,.T.);
#14114=EDGE_CURVE('',#11397,#11398,#9855,.T.);
#14115=EDGE_CURVE('',#11344,#11398,#6140,.T.);
#14116=EDGE_CURVE('',#11398,#11399,#6141,.T.);
#14117=EDGE_CURVE('',#11399,#11345,#6142,.T.);
#14118=EDGE_CURVE('',#11399,#11400,#9856,.T.);
#14119=EDGE_CURVE('',#11346,#11400,#6143,.T.);
#14120=EDGE_CURVE('',#11400,#11401,#6144,.T.);
#14121=EDGE_CURVE('',#11401,#11347,#6145,.T.);
#14122=EDGE_CURVE('',#11401,#11402,#9857,.T.);
#14123=EDGE_CURVE('',#11348,#11402,#6146,.T.);
#14124=EDGE_CURVE('',#11402,#11403,#9858,.T.);
#14125=EDGE_CURVE('',#11403,#11349,#6147,.T.);
#14126=EDGE_CURVE('',#11403,#11404,#9859,.T.);
#14127=EDGE_CURVE('',#11350,#11404,#6148,.T.);
#14128=EDGE_CURVE('',#11404,#11405,#6149,.T.);
#14129=EDGE_CURVE('',#11405,#11351,#6150,.T.);
#14130=EDGE_CURVE('',#11405,#11406,#9860,.T.);
#14131=EDGE_CURVE('',#11352,#11406,#6151,.T.);
#14132=EDGE_CURVE('',#11406,#11407,#6152,.T.);
#14133=EDGE_CURVE('',#11407,#11353,#6153,.T.);
#14134=EDGE_CURVE('',#11407,#11408,#9861,.T.);
#14135=EDGE_CURVE('',#11354,#11408,#6154,.T.);
#14136=EDGE_CURVE('',#11408,#11363,#6155,.T.);
#14137=EDGE_CURVE('',#11409,#11410,#6156,.T.);
#14138=EDGE_CURVE('',#11410,#11411,#6157,.T.);
#14139=EDGE_CURVE('',#11411,#11412,#6158,.T.);
#14140=EDGE_CURVE('',#11412,#11409,#6159,.T.);
#14141=EDGE_CURVE('',#11413,#11414,#6160,.T.);
#14142=EDGE_CURVE('',#11414,#11415,#6161,.T.);
#14143=EDGE_CURVE('',#11415,#11416,#6162,.T.);
#14144=EDGE_CURVE('',#11413,#11416,#6163,.T.);
#14145=EDGE_CURVE('',#11417,#11093,#6164,.T.);
#14146=EDGE_CURVE('',#11362,#11417,#6165,.T.);
#14147=EDGE_CURVE('',#11094,#11418,#6166,.T.);
#14148=EDGE_CURVE('',#11361,#11418,#6167,.T.);
#14149=EDGE_CURVE('',#11418,#11417,#9862,.T.);
#14150=EDGE_CURVE('',#11410,#11419,#9863,.T.);
#14151=EDGE_CURVE('',#11420,#11409,#9864,.T.);
#14152=EDGE_CURVE('',#11419,#11420,#6168,.T.);
#14153=EDGE_CURVE('',#11421,#11419,#6169,.T.);
#14154=EDGE_CURVE('',#11421,#11422,#6170,.T.);
#14155=EDGE_CURVE('',#11422,#11423,#6171,.T.);
#14156=EDGE_CURVE('',#11411,#11423,#6172,.T.);
#14157=EDGE_CURVE('',#11421,#11424,#6173,.T.);
#14158=EDGE_CURVE('',#11424,#11425,#6174,.T.);
#14159=EDGE_CURVE('',#11422,#11425,#6175,.T.);
#14160=EDGE_CURVE('',#11426,#11427,#6176,.T.);
#14161=EDGE_CURVE('',#11427,#11428,#6177,.T.);
#14162=EDGE_CURVE('',#11428,#11429,#6178,.T.);
#14163=EDGE_CURVE('',#11426,#11429,#6179,.T.);
#14164=EDGE_CURVE('',#11430,#11429,#6180,.T.);
#14165=EDGE_CURVE('',#11430,#11415,#9865,.T.);
#14166=EDGE_CURVE('',#11431,#11414,#6181,.T.);
#14167=EDGE_CURVE('',#11431,#11426,#6182,.T.);
#14168=EDGE_CURVE('',#11432,#11430,#6183,.T.);
#14169=EDGE_CURVE('',#11432,#11416,#9866,.T.);
#14170=EDGE_CURVE('',#11433,#11434,#6184,.T.);
#14171=EDGE_CURVE('',#11434,#11435,#6185,.T.);
#14172=EDGE_CURVE('',#11435,#11436,#6186,.T.);
#14173=EDGE_CURVE('',#11436,#11437,#6187,.T.);
#14174=EDGE_CURVE('',#11437,#11438,#6188,.T.);
#14175=EDGE_CURVE('',#11438,#11439,#6189,.T.);
#14176=EDGE_CURVE('',#11439,#11440,#6190,.T.);
#14177=EDGE_CURVE('',#11440,#11441,#6191,.T.);
#14178=EDGE_CURVE('',#11441,#11442,#6192,.T.);
#14179=EDGE_CURVE('',#11442,#11443,#6193,.T.);
#14180=EDGE_CURVE('',#11443,#11444,#9867,.T.);
#14181=EDGE_CURVE('',#11444,#11445,#6194,.T.);
#14182=EDGE_CURVE('',#11445,#11446,#9868,.T.);
#14183=EDGE_CURVE('',#11446,#11447,#6195,.T.);
#14184=EDGE_CURVE('',#11447,#11448,#9869,.T.);
#14185=EDGE_CURVE('',#11448,#11449,#9870,.T.);
#14186=EDGE_CURVE('',#11449,#11450,#9871,.T.);
#14187=EDGE_CURVE('',#11450,#11451,#6196,.T.);
#14188=EDGE_CURVE('',#11451,#11452,#9872,.T.);
#14189=EDGE_CURVE('',#11452,#11453,#6197,.T.);
#14190=EDGE_CURVE('',#11453,#11454,#9873,.T.);
#14191=EDGE_CURVE('',#11454,#11455,#6198,.T.);
#14192=EDGE_CURVE('',#11455,#11456,#9874,.T.);
#14193=EDGE_CURVE('',#11456,#11457,#9875,.T.);
#14194=EDGE_CURVE('',#11457,#11458,#9876,.T.);
#14195=EDGE_CURVE('',#11458,#11459,#6199,.T.);
#14196=EDGE_CURVE('',#11459,#11460,#6200,.T.);
#14197=EDGE_CURVE('',#11460,#11461,#6201,.T.);
#14198=EDGE_CURVE('',#11461,#11462,#9877,.T.);
#14199=EDGE_CURVE('',#11462,#11463,#9878,.T.);
#14200=EDGE_CURVE('',#11463,#11464,#9879,.T.);
#14201=EDGE_CURVE('',#11464,#11465,#6202,.T.);
#14202=EDGE_CURVE('',#11465,#11466,#9880,.T.);
#14203=EDGE_CURVE('',#11466,#11467,#6203,.T.);
#14204=EDGE_CURVE('',#11467,#11468,#9881,.T.);
#14205=EDGE_CURVE('',#11468,#11469,#6204,.T.);
#14206=EDGE_CURVE('',#11469,#11470,#9882,.T.);
#14207=EDGE_CURVE('',#11470,#11471,#9883,.T.);
#14208=EDGE_CURVE('',#11471,#11472,#9884,.T.);
#14209=EDGE_CURVE('',#11472,#11473,#6205,.T.);
#14210=EDGE_CURVE('',#11473,#11474,#9885,.T.);
#14211=EDGE_CURVE('',#11474,#11475,#6206,.T.);
#14212=EDGE_CURVE('',#11475,#11476,#9886,.T.);
#14213=EDGE_CURVE('',#11476,#11433,#6207,.T.);
#14214=EDGE_CURVE('',#11431,#11477,#6208,.T.);
#14215=EDGE_CURVE('',#11477,#11413,#6209,.T.);
#14216=EDGE_CURVE('',#11478,#11423,#6210,.T.);
#14217=EDGE_CURVE('',#11478,#11412,#6211,.T.);
#14218=EDGE_CURVE('',#11479,#11480,#6212,.T.);
#14219=EDGE_CURVE('',#11420,#11480,#6213,.T.);
#14220=EDGE_CURVE('',#11478,#11479,#6214,.T.);
#14221=EDGE_CURVE('',#11479,#11481,#6215,.T.);
#14222=EDGE_CURVE('',#11481,#11482,#6216,.T.);
#14223=EDGE_CURVE('',#11482,#11480,#6217,.T.);
#14224=EDGE_CURVE('',#11483,#11477,#6218,.T.);
#14225=EDGE_CURVE('',#11432,#11484,#6219,.T.);
#14226=EDGE_CURVE('',#11484,#11483,#6220,.T.);
#14227=EDGE_CURVE('',#11484,#11485,#6221,.T.);
#14228=EDGE_CURVE('',#11485,#11486,#6222,.T.);
#14229=EDGE_CURVE('',#11483,#11486,#6223,.T.);
#14230=EDGE_CURVE('',#11121,#11482,#648,.T.);
#14231=EDGE_CURVE('',#11424,#11123,#649,.T.);
#14232=EDGE_CURVE('',#11487,#11427,#9887,.T.);
#14233=EDGE_CURVE('',#11488,#11431,#6224,.T.);
#14234=EDGE_CURVE('',#11488,#11489,#6225,.T.);
#14235=EDGE_CURVE('',#11487,#11489,#6226,.T.);
#14236=EDGE_CURVE('',#11490,#11491,#6227,.T.);
#14237=EDGE_CURVE('',#11491,#11487,#6228,.T.);
#14238=EDGE_CURVE('',#11489,#11490,#6229,.T.);
#14239=EDGE_CURVE('',#11124,#11492,#650,.T.);
#14240=EDGE_CURVE('',#11493,#11126,#6230,.T.);
#14241=EDGE_CURVE('',#11492,#11493,#6231,.T.);
#14242=EDGE_CURVE('',#11494,#11495,#6232,.T.);
#14243=EDGE_CURVE('',#11494,#11492,#6233,.T.);
#14244=EDGE_CURVE('',#11493,#11495,#6234,.T.);
#14245=EDGE_CURVE('',#11495,#11496,#6235,.T.);
#14246=EDGE_CURVE('',#11423,#11496,#6236,.T.);
#14247=EDGE_CURVE('',#11425,#11494,#9888,.T.);
#14248=EDGE_CURVE('',#11491,#11497,#651,.T.);
#14249=EDGE_CURVE('',#11498,#11490,#6237,.T.);
#14250=EDGE_CURVE('',#11497,#11498,#6238,.T.);
#14251=EDGE_CURVE('',#11485,#11117,#652,.T.);
#14252=EDGE_CURVE('',#11118,#11428,#653,.T.);
#14253=EDGE_CURVE('',#11499,#11500,#6239,.T.);
#14254=EDGE_CURVE('',#11434,#11500,#6240,.T.);
#14255=EDGE_CURVE('',#11433,#11499,#6241,.T.);
#14256=EDGE_CURVE('',#11500,#11501,#6242,.T.);
#14257=EDGE_CURVE('',#11435,#11501,#6243,.T.);
#14258=EDGE_CURVE('',#11501,#11502,#6244,.T.);
#14259=EDGE_CURVE('',#11436,#11502,#6245,.T.);
#14260=EDGE_CURVE('',#11502,#11503,#6246,.T.);
#14261=EDGE_CURVE('',#11437,#11503,#6247,.T.);
#14262=EDGE_CURVE('',#11503,#11504,#6248,.T.);
#14263=EDGE_CURVE('',#11438,#11504,#6249,.T.);
#14264=EDGE_CURVE('',#11504,#11505,#6250,.T.);
#14265=EDGE_CURVE('',#11439,#11505,#6251,.T.);
#14266=EDGE_CURVE('',#11505,#11506,#6252,.T.);
#14267=EDGE_CURVE('',#11440,#11506,#6253,.T.);
#14268=EDGE_CURVE('',#11506,#11507,#6254,.T.);
#14269=EDGE_CURVE('',#11441,#11507,#6255,.T.);
#14270=EDGE_CURVE('',#11507,#11508,#6256,.T.);
#14271=EDGE_CURVE('',#11442,#11508,#6257,.T.);
#14272=EDGE_CURVE('',#11508,#11509,#6258,.T.);
#14273=EDGE_CURVE('',#11443,#11509,#6259,.T.);
#14274=EDGE_CURVE('',#11509,#11510,#9889,.T.);
#14275=EDGE_CURVE('',#11444,#11510,#6260,.T.);
#14276=EDGE_CURVE('',#11510,#11511,#6261,.T.);
#14277=EDGE_CURVE('',#11445,#11511,#6262,.T.);
#14278=EDGE_CURVE('',#11511,#11512,#9890,.T.);
#14279=EDGE_CURVE('',#11446,#11512,#6263,.T.);
#14280=EDGE_CURVE('',#11512,#11513,#6264,.T.);
#14281=EDGE_CURVE('',#11447,#11513,#6265,.T.);
#14282=EDGE_CURVE('',#11513,#11514,#9891,.T.);
#14283=EDGE_CURVE('',#11448,#11514,#6266,.T.);
#14284=EDGE_CURVE('',#11514,#11515,#9892,.T.);
#14285=EDGE_CURVE('',#11449,#11515,#6267,.T.);
#14286=EDGE_CURVE('',#11515,#11516,#9893,.T.);
#14287=EDGE_CURVE('',#11450,#11516,#6268,.T.);
#14288=EDGE_CURVE('',#11516,#11517,#6269,.T.);
#14289=EDGE_CURVE('',#11451,#11517,#6270,.T.);
#14290=EDGE_CURVE('',#11517,#11518,#9894,.T.);
#14291=EDGE_CURVE('',#11452,#11518,#6271,.T.);
#14292=EDGE_CURVE('',#11518,#11519,#6272,.T.);
#14293=EDGE_CURVE('',#11453,#11519,#6273,.T.);
#14294=EDGE_CURVE('',#11519,#11520,#9895,.T.);
#14295=EDGE_CURVE('',#11454,#11520,#6274,.T.);
#14296=EDGE_CURVE('',#11520,#11521,#6275,.T.);
#14297=EDGE_CURVE('',#11455,#11521,#6276,.T.);
#14298=EDGE_CURVE('',#11521,#11522,#9896,.T.);
#14299=EDGE_CURVE('',#11456,#11522,#6277,.T.);
#14300=EDGE_CURVE('',#11522,#11523,#9897,.T.);
#14301=EDGE_CURVE('',#11457,#11523,#6278,.T.);
#14302=EDGE_CURVE('',#11523,#11524,#9898,.T.);
#14303=EDGE_CURVE('',#11458,#11524,#6279,.T.);
#14304=EDGE_CURVE('',#11524,#11525,#6280,.T.);
#14305=EDGE_CURVE('',#11459,#11525,#6281,.T.);
#14306=EDGE_CURVE('',#11525,#11526,#6282,.T.);
#14307=EDGE_CURVE('',#11460,#11526,#6283,.T.);
#14308=EDGE_CURVE('',#11526,#11527,#6284,.T.);
#14309=EDGE_CURVE('',#11461,#11527,#6285,.T.);
#14310=EDGE_CURVE('',#11527,#11528,#9899,.T.);
#14311=EDGE_CURVE('',#11462,#11528,#6286,.T.);
#14312=EDGE_CURVE('',#11528,#11529,#9900,.T.);
#14313=EDGE_CURVE('',#11463,#11529,#6287,.T.);
#14314=EDGE_CURVE('',#11529,#11530,#9901,.T.);
#14315=EDGE_CURVE('',#11464,#11530,#6288,.T.);
#14316=EDGE_CURVE('',#11530,#11531,#6289,.T.);
#14317=EDGE_CURVE('',#11465,#11531,#6290,.T.);
#14318=EDGE_CURVE('',#11531,#11532,#9902,.T.);
#14319=EDGE_CURVE('',#11466,#11532,#6291,.T.);
#14320=EDGE_CURVE('',#11532,#11533,#6292,.T.);
#14321=EDGE_CURVE('',#11467,#11533,#6293,.T.);
#14322=EDGE_CURVE('',#11533,#11534,#9903,.T.);
#14323=EDGE_CURVE('',#11468,#11534,#6294,.T.);
#14324=EDGE_CURVE('',#11534,#11535,#6295,.T.);
#14325=EDGE_CURVE('',#11469,#11535,#6296,.T.);
#14326=EDGE_CURVE('',#11535,#11536,#9904,.T.);
#14327=EDGE_CURVE('',#11470,#11536,#6297,.T.);
#14328=EDGE_CURVE('',#11536,#11537,#9905,.T.);
#14329=EDGE_CURVE('',#11471,#11537,#6298,.T.);
#14330=EDGE_CURVE('',#11537,#11538,#9906,.T.);
#14331=EDGE_CURVE('',#11472,#11538,#6299,.T.);
#14332=EDGE_CURVE('',#11538,#11539,#6300,.T.);
#14333=EDGE_CURVE('',#11473,#11539,#6301,.T.);
#14334=EDGE_CURVE('',#11539,#11540,#9907,.T.);
#14335=EDGE_CURVE('',#11474,#11540,#6302,.T.);
#14336=EDGE_CURVE('',#11540,#11541,#6303,.T.);
#14337=EDGE_CURVE('',#11475,#11541,#6304,.T.);
#14338=EDGE_CURVE('',#11541,#11542,#9908,.T.);
#14339=EDGE_CURVE('',#11476,#11542,#6305,.T.);
#14340=EDGE_CURVE('',#11542,#11499,#6306,.T.);
#14341=EDGE_CURVE('',#11543,#11544,#6307,.T.);
#14342=EDGE_CURVE('',#11544,#11545,#6308,.T.);
#14343=EDGE_CURVE('',#11545,#11546,#6309,.T.);
#14344=EDGE_CURVE('',#11546,#11543,#6310,.T.);
#14345=EDGE_CURVE('',#11547,#11544,#6311,.T.);
#14346=EDGE_CURVE('',#11547,#11548,#6312,.T.);
#14347=EDGE_CURVE('',#11545,#11548,#6313,.T.);
#14348=EDGE_CURVE('',#11549,#11547,#6314,.T.);
#14349=EDGE_CURVE('',#11550,#11549,#6315,.T.);
#14350=EDGE_CURVE('',#11548,#11550,#6316,.T.);
#14351=EDGE_CURVE('',#11551,#11549,#6317,.T.);
#14352=EDGE_CURVE('',#11552,#11551,#6318,.T.);
#14353=EDGE_CURVE('',#11550,#11552,#6319,.T.);
#14354=EDGE_CURVE('',#11553,#11551,#6320,.T.);
#14355=EDGE_CURVE('',#11554,#11553,#6321,.T.);
#14356=EDGE_CURVE('',#11552,#11554,#6322,.T.);
#14357=EDGE_CURVE('',#11555,#11556,#6323,.T.);
#14358=EDGE_CURVE('',#11557,#11555,#6324,.T.);
#14359=EDGE_CURVE('',#11558,#11557,#6325,.T.);
#14360=EDGE_CURVE('',#11558,#11556,#6326,.T.);
#14361=EDGE_CURVE('',#11559,#11555,#6327,.T.);
#14362=EDGE_CURVE('',#11560,#11559,#6328,.T.);
#14363=EDGE_CURVE('',#11557,#11560,#6329,.T.);
#14364=EDGE_CURVE('',#11561,#11559,#6330,.T.);
#14365=EDGE_CURVE('',#11562,#11561,#6331,.T.);
#14366=EDGE_CURVE('',#11560,#11562,#6332,.T.);
#14367=EDGE_CURVE('',#11562,#11546,#6333,.T.);
#14368=EDGE_CURVE('',#11543,#11561,#6334,.T.);
#14369=EDGE_CURVE('',#11488,#11563,#6335,.T.);
#14370=EDGE_CURVE('',#11477,#11564,#6336,.T.);
#14371=EDGE_CURVE('',#11564,#11565,#6337,.T.);
#14372=EDGE_CURVE('',#11565,#11563,#6338,.T.);
#14373=EDGE_CURVE('',#11565,#11566,#6339,.T.);
#14374=EDGE_CURVE('',#11566,#11567,#6340,.T.);
#14375=EDGE_CURVE('',#11563,#11567,#6341,.T.);
#14376=EDGE_CURVE('',#11568,#11569,#6342,.T.);
#14377=EDGE_CURVE('',#11567,#11569,#6343,.T.);
#14378=EDGE_CURVE('',#11566,#11568,#6344,.T.);
#14379=EDGE_CURVE('',#11570,#11571,#6345,.T.);
#14380=EDGE_CURVE('',#11571,#11569,#6346,.T.);
#14381=EDGE_CURVE('',#11570,#11568,#6347,.T.);
#14382=EDGE_CURVE('',#11572,#11573,#6348,.T.);
#14383=EDGE_CURVE('',#11573,#11571,#6349,.T.);
#14384=EDGE_CURVE('',#11572,#11570,#6350,.T.);
#14385=EDGE_CURVE('',#11574,#11575,#6351,.T.);
#14386=EDGE_CURVE('',#11575,#11573,#6352,.T.);
#14387=EDGE_CURVE('',#11574,#11572,#6353,.T.);
#14388=EDGE_CURVE('',#11574,#11576,#6354,.T.);
#14389=EDGE_CURVE('',#11576,#11577,#6355,.T.);
#14390=EDGE_CURVE('',#11575,#11577,#6356,.T.);
#14391=EDGE_CURVE('',#11578,#11579,#6357,.T.);
#14392=EDGE_CURVE('',#11579,#11577,#6358,.T.);
#14393=EDGE_CURVE('',#11578,#11576,#6359,.T.);
#14394=EDGE_CURVE('',#11580,#11581,#6360,.T.);
#14395=EDGE_CURVE('',#11581,#11579,#6361,.T.);
#14396=EDGE_CURVE('',#11580,#11578,#6362,.T.);
#14397=EDGE_CURVE('',#11582,#11583,#6363,.T.);
#14398=EDGE_CURVE('',#11583,#11581,#6364,.T.);
#14399=EDGE_CURVE('',#11582,#11580,#6365,.T.);
#14400=EDGE_CURVE('',#11582,#11584,#6366,.T.);
#14401=EDGE_CURVE('',#11584,#11585,#6367,.T.);
#14402=EDGE_CURVE('',#11583,#11585,#6368,.T.);
#14403=EDGE_CURVE('',#11584,#11586,#6369,.T.);
#14404=EDGE_CURVE('',#11586,#11587,#6370,.T.);
#14405=EDGE_CURVE('',#11585,#11587,#6371,.T.);
#14406=EDGE_CURVE('',#11586,#11588,#6372,.T.);
#14407=EDGE_CURVE('',#11588,#11589,#6373,.T.);
#14408=EDGE_CURVE('',#11587,#11589,#6374,.T.);
#14409=EDGE_CURVE('',#11588,#11590,#6375,.T.);
#14410=EDGE_CURVE('',#11590,#11591,#6376,.T.);
#14411=EDGE_CURVE('',#11589,#11591,#6377,.T.);
#14412=EDGE_CURVE('',#11590,#11592,#6378,.T.);
#14413=EDGE_CURVE('',#11592,#11478,#6379,.T.);
#14414=EDGE_CURVE('',#11591,#11496,#6380,.T.);
#14415=EDGE_CURVE('',#11593,#11481,#9909,.T.);
#14416=EDGE_CURVE('',#11592,#11594,#6381,.T.);
#14417=EDGE_CURVE('',#11593,#11594,#6382,.T.);
#14418=EDGE_CURVE('',#11595,#11596,#6383,.T.);
#14419=EDGE_CURVE('',#11596,#11593,#6384,.T.);
#14420=EDGE_CURVE('',#11594,#11595,#6385,.T.);
#14421=EDGE_CURVE('',#11596,#11597,#654,.T.);
#14422=EDGE_CURVE('',#11595,#11598,#6386,.T.);
#14423=EDGE_CURVE('',#11598,#11597,#6387,.T.);
#14424=EDGE_CURVE('',#11114,#11599,#655,.T.);
#14425=EDGE_CURVE('',#11116,#11600,#6388,.T.);
#14426=EDGE_CURVE('',#11599,#11600,#6389,.T.);
#14427=EDGE_CURVE('',#11601,#11602,#6390,.T.);
#14428=EDGE_CURVE('',#11601,#11599,#6391,.T.);
#14429=EDGE_CURVE('',#11600,#11602,#6392,.T.);
#14430=EDGE_CURVE('',#11602,#11564,#6393,.T.);
#14431=EDGE_CURVE('',#11486,#11601,#9910,.T.);
#14432=EDGE_CURVE('',#11597,#11120,#656,.T.);
#14433=EDGE_CURVE('',#11598,#11603,#6394,.T.);
#14434=EDGE_CURVE('',#11603,#11120,#6395,.T.);
#14435=EDGE_CURVE('',#11556,#11604,#6396,.T.);
#14436=EDGE_CURVE('',#11605,#11558,#6397,.T.);
#14437=EDGE_CURVE('',#11605,#11604,#6398,.T.);
#14438=EDGE_CURVE('',#11606,#11553,#6399,.T.);
#14439=EDGE_CURVE('',#11607,#11606,#6400,.T.);
#14440=EDGE_CURVE('',#11554,#11607,#6401,.T.);
#14441=EDGE_CURVE('',#11125,#11605,#6402,.T.);
#14442=EDGE_CURVE('',#11607,#11608,#6403,.T.);
#14443=EDGE_CURVE('',#11608,#11498,#6404,.T.);
#14444=EDGE_CURVE('',#11497,#11119,#657,.T.);
#14445=EDGE_CURVE('',#11119,#11608,#6405,.T.);
#14446=EDGE_CURVE('',#11604,#11609,#6406,.T.);
#14447=EDGE_CURVE('',#11609,#11610,#6407,.T.);
#14448=EDGE_CURVE('',#11610,#11611,#9911,.T.);
#14449=EDGE_CURVE('',#11611,#11612,#6408,.T.);
#14450=EDGE_CURVE('',#11612,#11613,#9912,.T.);
#14451=EDGE_CURVE('',#11613,#11614,#6409,.T.);
#14452=EDGE_CURVE('',#11614,#11615,#9913,.T.);
#14453=EDGE_CURVE('',#11615,#11616,#9914,.T.);
#14454=EDGE_CURVE('',#11616,#11617,#9915,.T.);
#14455=EDGE_CURVE('',#11617,#11618,#6410,.T.);
#14456=EDGE_CURVE('',#11618,#11619,#9916,.T.);
#14457=EDGE_CURVE('',#11619,#11620,#6411,.T.);
#14458=EDGE_CURVE('',#11620,#11621,#9917,.T.);
#14459=EDGE_CURVE('',#11621,#11622,#6412,.T.);
#14460=EDGE_CURVE('',#11622,#11623,#9918,.T.);
#14461=EDGE_CURVE('',#11623,#11624,#9919,.T.);
#14462=EDGE_CURVE('',#11624,#11625,#9920,.T.);
#14463=EDGE_CURVE('',#11625,#11626,#6413,.T.);
#14464=EDGE_CURVE('',#11626,#11627,#6414,.T.);
#14465=EDGE_CURVE('',#11627,#11628,#6415,.T.);
#14466=EDGE_CURVE('',#11628,#11629,#9921,.T.);
#14467=EDGE_CURVE('',#11629,#11630,#9922,.T.);
#14468=EDGE_CURVE('',#11630,#11631,#9923,.T.);
#14469=EDGE_CURVE('',#11631,#11632,#6416,.T.);
#14470=EDGE_CURVE('',#11632,#11633,#9924,.T.);
#14471=EDGE_CURVE('',#11633,#11634,#6417,.T.);
#14472=EDGE_CURVE('',#11634,#11635,#9925,.T.);
#14473=EDGE_CURVE('',#11635,#11636,#6418,.T.);
#14474=EDGE_CURVE('',#11636,#11637,#9926,.T.);
#14475=EDGE_CURVE('',#11637,#11638,#9927,.T.);
#14476=EDGE_CURVE('',#11638,#11639,#9928,.T.);
#14477=EDGE_CURVE('',#11639,#11640,#6419,.T.);
#14478=EDGE_CURVE('',#11640,#11641,#9929,.T.);
#14479=EDGE_CURVE('',#11641,#11642,#6420,.T.);
#14480=EDGE_CURVE('',#11642,#11643,#9930,.T.);
#14481=EDGE_CURVE('',#11643,#11644,#6421,.T.);
#14482=EDGE_CURVE('',#11644,#11606,#6422,.T.);
#14483=EDGE_CURVE('',#11645,#11115,#6423,.T.);
#14484=EDGE_CURVE('',#11646,#11645,#6424,.T.);
#14485=EDGE_CURVE('',#11647,#11646,#6425,.T.);
#14486=EDGE_CURVE('',#11648,#11647,#6426,.T.);
#14487=EDGE_CURVE('',#11649,#11648,#6427,.T.);
#14488=EDGE_CURVE('',#11649,#11650,#6428,.T.);
#14489=EDGE_CURVE('',#11651,#11650,#6429,.T.);
#14490=EDGE_CURVE('',#11651,#11652,#6430,.T.);
#14491=EDGE_CURVE('',#11653,#11652,#6431,.T.);
#14492=EDGE_CURVE('',#11654,#11653,#6432,.T.);
#14493=EDGE_CURVE('',#11655,#11654,#6433,.T.);
#14494=EDGE_CURVE('',#11656,#11655,#6434,.T.);
#14495=EDGE_CURVE('',#11603,#11656,#6435,.T.);
#14496=EDGE_CURVE('',#11657,#11658,#6436,.T.);
#14497=EDGE_CURVE('',#11657,#11652,#6437,.T.);
#14498=EDGE_CURVE('',#11658,#11651,#6438,.T.);
#14499=EDGE_CURVE('',#11659,#11660,#6439,.T.);
#14500=EDGE_CURVE('',#11660,#11648,#6440,.T.);
#14501=EDGE_CURVE('',#11659,#11647,#6441,.T.);
#14502=EDGE_CURVE('',#11661,#11659,#6442,.T.);
#14503=EDGE_CURVE('',#11661,#11646,#6443,.T.);
#14504=EDGE_CURVE('',#11662,#11661,#6444,.T.);
#14505=EDGE_CURVE('',#11662,#11645,#6445,.T.);
#14506=EDGE_CURVE('',#11660,#11663,#6446,.T.);
#14507=EDGE_CURVE('',#11649,#11663,#6447,.T.);
#14508=EDGE_CURVE('',#11664,#11642,#6448,.T.);
#14509=EDGE_CURVE('',#11664,#11665,#9931,.T.);
#14510=EDGE_CURVE('',#11643,#11665,#6449,.T.);
#14511=EDGE_CURVE('',#11666,#11640,#6450,.T.);
#14512=EDGE_CURVE('',#11666,#11667,#9932,.T.);
#14513=EDGE_CURVE('',#11641,#11667,#6451,.T.);
#14514=EDGE_CURVE('',#11667,#11664,#6452,.T.);
#14515=EDGE_CURVE('',#11665,#11668,#6453,.T.);
#14516=EDGE_CURVE('',#11668,#11644,#6454,.T.);
#14517=EDGE_CURVE('',#11668,#11662,#6455,.T.);
#14518=EDGE_CURVE('',#11669,#11670,#9933,.T.);
#14519=EDGE_CURVE('',#11639,#11670,#6456,.T.);
#14520=EDGE_CURVE('',#11669,#11638,#6457,.T.);
#14521=EDGE_CURVE('',#11671,#11672,#9934,.T.);
#14522=EDGE_CURVE('',#11637,#11672,#6458,.T.);
#14523=EDGE_CURVE('',#11671,#11636,#6459,.T.);
#14524=EDGE_CURVE('',#11672,#11669,#9935,.T.);
#14525=EDGE_CURVE('',#11673,#11674,#9936,.T.);
#14526=EDGE_CURVE('',#11635,#11674,#6460,.T.);
#14527=EDGE_CURVE('',#11673,#11634,#6461,.T.);
#14528=EDGE_CURVE('',#11675,#11676,#9937,.T.);
#14529=EDGE_CURVE('',#11633,#11676,#6462,.T.);
#14530=EDGE_CURVE('',#11675,#11632,#6463,.T.);
#14531=EDGE_CURVE('',#11676,#11673,#6464,.T.);
#14532=EDGE_CURVE('',#11674,#11671,#6465,.T.);
#14533=EDGE_CURVE('',#11677,#11678,#9938,.T.);
#14534=EDGE_CURVE('',#11631,#11678,#6466,.T.);
#14535=EDGE_CURVE('',#11677,#11630,#6467,.T.);
#14536=EDGE_CURVE('',#11679,#11680,#9939,.T.);
#14537=EDGE_CURVE('',#11629,#11680,#6468,.T.);
#14538=EDGE_CURVE('',#11679,#11628,#6469,.T.);
#14539=EDGE_CURVE('',#11680,#11677,#9940,.T.);
#14540=EDGE_CURVE('',#11681,#11626,#6470,.T.);
#14541=EDGE_CURVE('',#11681,#11682,#6471,.T.);
#14542=EDGE_CURVE('',#11682,#11627,#6472,.T.);
#14543=EDGE_CURVE('',#11682,#11679,#6473,.T.);
#14544=EDGE_CURVE('',#11683,#11684,#9941,.T.);
#14545=EDGE_CURVE('',#11625,#11684,#6474,.T.);
#14546=EDGE_CURVE('',#11683,#11624,#6475,.T.);
#14547=EDGE_CURVE('',#11685,#11686,#9942,.T.);
#14548=EDGE_CURVE('',#11623,#11686,#6476,.T.);
#14549=EDGE_CURVE('',#11685,#11622,#6477,.T.);
#14550=EDGE_CURVE('',#11686,#11683,#9943,.T.);
#14551=EDGE_CURVE('',#11687,#11688,#9944,.T.);
#14552=EDGE_CURVE('',#11621,#11688,#6478,.T.);
#14553=EDGE_CURVE('',#11687,#11620,#6479,.T.);
#14554=EDGE_CURVE('',#11689,#11690,#9945,.T.);
#14555=EDGE_CURVE('',#11619,#11690,#6480,.T.);
#14556=EDGE_CURVE('',#11689,#11618,#6481,.T.);
#14557=EDGE_CURVE('',#11690,#11687,#6482,.T.);
#14558=EDGE_CURVE('',#11688,#11685,#6483,.T.);
#14559=EDGE_CURVE('',#11684,#11681,#6484,.T.);
#14560=EDGE_CURVE('',#11691,#11692,#9946,.T.);
#14561=EDGE_CURVE('',#11617,#11692,#6485,.T.);
#14562=EDGE_CURVE('',#11691,#11616,#6486,.T.);
#14563=EDGE_CURVE('',#11693,#11694,#9947,.T.);
#14564=EDGE_CURVE('',#11615,#11694,#6487,.T.);
#14565=EDGE_CURVE('',#11693,#11614,#6488,.T.);
#14566=EDGE_CURVE('',#11694,#11691,#9948,.T.);
#14567=EDGE_CURVE('',#11695,#11612,#6489,.T.);
#14568=EDGE_CURVE('',#11695,#11696,#9949,.T.);
#14569=EDGE_CURVE('',#11613,#11696,#6490,.T.);
#14570=EDGE_CURVE('',#11697,#11610,#6491,.T.);
#14571=EDGE_CURVE('',#11697,#11698,#9950,.T.);
#14572=EDGE_CURVE('',#11611,#11698,#6492,.T.);
#14573=EDGE_CURVE('',#11699,#11700,#6493,.T.);
#14574=EDGE_CURVE('',#11700,#11656,#6494,.T.);
#14575=EDGE_CURVE('',#11699,#11655,#6495,.T.);
#14576=EDGE_CURVE('',#11701,#11699,#6496,.T.);
#14577=EDGE_CURVE('',#11701,#11654,#6497,.T.);
#14578=EDGE_CURVE('',#11702,#11701,#6498,.T.);
#14579=EDGE_CURVE('',#11702,#11653,#6499,.T.);
#14580=EDGE_CURVE('',#11657,#11702,#6500,.T.);
#14581=EDGE_CURVE('',#11700,#11703,#6501,.T.);
#14582=EDGE_CURVE('',#11703,#11609,#6502,.T.);
#14583=EDGE_CURVE('',#11703,#11697,#6503,.T.);
#14584=EDGE_CURVE('',#11698,#11695,#6504,.T.);
#14585=EDGE_CURVE('',#11696,#11693,#6505,.T.);
#14586=EDGE_CURVE('',#11692,#11689,#6506,.T.);
#14587=EDGE_CURVE('',#11678,#11675,#6507,.T.);
#14588=EDGE_CURVE('',#11670,#11666,#6508,.T.);
#14589=EDGE_CURVE('',#11704,#11663,#6509,.T.);
#14590=EDGE_CURVE('',#11650,#11704,#6510,.T.);
#14591=EDGE_CURVE('',#11704,#11658,#6511,.T.);
#14592=EDGE_CURVE('',#11705,#11368,#6512,.T.);
#14593=EDGE_CURVE('',#11705,#11313,#6513,.T.);
#14594=EDGE_CURVE('',#11706,#11705,#9951,.T.);
#14595=EDGE_CURVE('',#11706,#11314,#6514,.T.);
#14596=EDGE_CURVE('',#11369,#11706,#6515,.T.);
#14597=EDGE_CURVE('',#11707,#11707,#9952,.T.);
#14598=EDGE_CURVE('',#11707,#11708,#9953,.T.);
#14599=EDGE_CURVE('',#11708,#11708,#9954,.T.);
#14600=EDGE_CURVE('',#11708,#11709,#9955,.T.);
#14601=EDGE_CURVE('',#11709,#11709,#9956,.T.);
#14602=EDGE_CURVE('',#11709,#11710,#6516,.T.);
#14603=EDGE_CURVE('',#11710,#11710,#9957,.T.);
#14604=EDGE_CURVE('',#11711,#11711,#9958,.T.);
#14605=EDGE_CURVE('',#11712,#11713,#9959,.T.);
#14606=EDGE_CURVE('',#11714,#11713,#83,.T.);
#14607=EDGE_CURVE('',#11712,#11714,#84,.T.);
#14608=EDGE_CURVE('',#11715,#11716,#9960,.T.);
#14609=EDGE_CURVE('',#11717,#11716,#85,.T.);
#14610=EDGE_CURVE('',#11715,#11717,#86,.T.);
#14611=EDGE_CURVE('',#11718,#11719,#9961,.T.);
#14612=EDGE_CURVE('',#11720,#11718,#115,.F.);
#14613=EDGE_CURVE('',#11720,#11721,#6517,.T.);
#14614=EDGE_CURVE('',#11721,#11721,#9962,.T.);
#14615=EDGE_CURVE('',#11719,#11720,#116,.F.);
#14616=EDGE_CURVE('',#11719,#11722,#9963,.T.);
#14617=EDGE_CURVE('',#11723,#11718,#9964,.T.);
#14618=EDGE_CURVE('',#11722,#11723,#9965,.T.);
#14619=EDGE_CURVE('',#11722,#11724,#6518,.T.);
#14620=EDGE_CURVE('',#11724,#11725,#9966,.T.);
#14621=EDGE_CURVE('',#11725,#11726,#9967,.T.);
#14622=EDGE_CURVE('',#11726,#11727,#9968,.T.);
#14623=EDGE_CURVE('',#11727,#11728,#9969,.T.);
#14624=EDGE_CURVE('',#11728,#11729,#9970,.T.);
#14625=EDGE_CURVE('',#11729,#11724,#9971,.T.);
#14626=EDGE_CURVE('',#11723,#11730,#9972,.T.);
#14627=EDGE_CURVE('',#11713,#11731,#9973,.T.);
#14628=EDGE_CURVE('',#11732,#11712,#9974,.T.);
#14629=EDGE_CURVE('',#11733,#11732,#9975,.T.);
#14630=EDGE_CURVE('',#11734,#11733,#9976,.T.);
#14631=EDGE_CURVE('',#11731,#11734,#9977,.T.);
#14632=EDGE_CURVE('',#11716,#11735,#9978,.T.);
#14633=EDGE_CURVE('',#11736,#11715,#9979,.T.);
#14634=EDGE_CURVE('',#11737,#11736,#9980,.T.);
#14635=EDGE_CURVE('',#11738,#11737,#9981,.T.);
#14636=EDGE_CURVE('',#11738,#11735,#9982,.T.);
#14637=EDGE_CURVE('',#11739,#11727,#6519,.T.);
#14638=EDGE_CURVE('',#11728,#11739,#6520,.T.);
#14639=EDGE_CURVE('',#11740,#11728,#6521,.T.);
#14640=EDGE_CURVE('',#11729,#11740,#6522,.T.);
#14641=EDGE_CURVE('',#11741,#11729,#6523,.T.);
#14642=EDGE_CURVE('',#11724,#11741,#6524,.T.);
#14643=EDGE_CURVE('',#11742,#11724,#6525,.T.);
#14644=EDGE_CURVE('',#11725,#11742,#6526,.T.);
#14645=EDGE_CURVE('',#11743,#11725,#6527,.T.);
#14646=EDGE_CURVE('',#11726,#11743,#6528,.T.);
#14647=EDGE_CURVE('',#11744,#11726,#6529,.T.);
#14648=EDGE_CURVE('',#11727,#11744,#6530,.T.);
#14649=EDGE_CURVE('',#11745,#11746,#6531,.T.);
#14650=EDGE_CURVE('',#11741,#11745,#6532,.T.);
#14651=EDGE_CURVE('',#11740,#11746,#6533,.T.);
#14652=EDGE_CURVE('',#11747,#11745,#6534,.T.);
#14653=EDGE_CURVE('',#11742,#11747,#6535,.T.);
#14654=EDGE_CURVE('',#11748,#11747,#6536,.T.);
#14655=EDGE_CURVE('',#11743,#11748,#6537,.T.);
#14656=EDGE_CURVE('',#11749,#11748,#6538,.T.);
#14657=EDGE_CURVE('',#11744,#11749,#6539,.T.);
#14658=EDGE_CURVE('',#11750,#11749,#6540,.T.);
#14659=EDGE_CURVE('',#11739,#11750,#6541,.T.);
#14660=EDGE_CURVE('',#11746,#11750,#6542,.T.);
#14661=EDGE_CURVE('',#11736,#11751,#87,.T.);
#14662=EDGE_CURVE('',#11751,#11715,#88,.T.);
#14663=EDGE_CURVE('',#11737,#11752,#89,.T.);
#14664=EDGE_CURVE('',#11752,#11736,#90,.T.);
#14665=EDGE_CURVE('',#11753,#11737,#91,.T.);
#14666=EDGE_CURVE('',#11738,#11753,#92,.T.);
#14667=EDGE_CURVE('',#11754,#11738,#93,.T.);
#14668=EDGE_CURVE('',#11735,#11754,#94,.T.);
#14669=EDGE_CURVE('',#11755,#11735,#95,.T.);
#14670=EDGE_CURVE('',#11716,#11755,#96,.T.);
#14671=EDGE_CURVE('',#11756,#11731,#97,.T.);
#14672=EDGE_CURVE('',#11713,#11756,#98,.T.);
#14673=EDGE_CURVE('',#11757,#11734,#99,.T.);
#14674=EDGE_CURVE('',#11731,#11757,#100,.T.);
#14675=EDGE_CURVE('',#11758,#11733,#101,.T.);
#14676=EDGE_CURVE('',#11734,#11758,#102,.T.);
#14677=EDGE_CURVE('',#11759,#11732,#103,.T.);
#14678=EDGE_CURVE('',#11733,#11759,#104,.T.);
#14679=EDGE_CURVE('',#11760,#11712,#105,.T.);
#14680=EDGE_CURVE('',#11732,#11760,#106,.T.);
#14681=EDGE_CURVE('',#11753,#11714,#6543,.T.);
#14682=EDGE_CURVE('',#11752,#11760,#6544,.T.);
#14683=EDGE_CURVE('',#11751,#11759,#6545,.T.);
#14684=EDGE_CURVE('',#11717,#11758,#6546,.T.);
#14685=EDGE_CURVE('',#11755,#11757,#6547,.T.);
#14686=EDGE_CURVE('',#11754,#11756,#6548,.T.);
#14687=EDGE_CURVE('',#11761,#11761,#9983,.T.);
#14688=EDGE_CURVE('',#11761,#11762,#6549,.T.);
#14689=EDGE_CURVE('',#11762,#11763,#9984,.T.);
#14690=EDGE_CURVE('',#11763,#11764,#6550,.T.);
#14691=EDGE_CURVE('',#11764,#11765,#117,.F.);
#14692=EDGE_CURVE('',#11765,#11766,#6551,.T.);
#14693=EDGE_CURVE('',#11766,#11762,#9985,.T.);
#14694=EDGE_CURVE('',#11767,#11767,#9986,.T.);
#14695=EDGE_CURVE('',#11767,#11761,#9987,.T.);
#14696=EDGE_CURVE('',#11768,#11768,#9988,.T.);
#14697=EDGE_CURVE('',#11768,#11769,#6552,.T.);
#14698=EDGE_CURVE('',#11769,#11769,#9989,.T.);
#14699=EDGE_CURVE('',#11770,#11770,#9990,.T.);
#14700=EDGE_CURVE('',#11770,#11768,#6553,.T.);
#14701=EDGE_CURVE('',#11771,#11771,#9991,.T.);
#14702=EDGE_CURVE('',#11771,#11770,#9992,.T.);
#14703=EDGE_CURVE('',#11772,#11772,#9993,.T.);
#14704=EDGE_CURVE('',#11772,#11773,#6554,.T.);
#14705=EDGE_CURVE('',#11773,#11773,#9994,.T.);
#14706=EDGE_CURVE('',#11774,#11775,#9995,.T.);
#14707=EDGE_CURVE('',#11775,#11774,#9996,.T.);
#14708=EDGE_CURVE('',#11775,#11772,#6555,.T.);
#14709=EDGE_CURVE('',#11774,#11776,#6556,.T.);
#14710=EDGE_CURVE('',#11776,#11776,#9997,.T.);
#14711=EDGE_CURVE('',#11777,#11777,#9998,.T.);
#14712=EDGE_CURVE('',#11777,#11778,#9999,.T.);
#14713=EDGE_CURVE('',#11778,#11778,#10000,.T.);
#14714=EDGE_CURVE('',#11779,#11779,#10001,.T.);
#14715=EDGE_CURVE('',#11779,#11777,#6557,.T.);
#14716=EDGE_CURVE('',#11780,#11780,#10002,.T.);
#14717=EDGE_CURVE('',#11780,#11781,#6558,.T.);
#14718=EDGE_CURVE('',#11781,#11781,#10003,.T.);
#14719=EDGE_CURVE('',#11782,#11783,#10004,.T.);
#14720=EDGE_CURVE('',#11783,#11782,#10005,.T.);
#14721=EDGE_CURVE('',#11783,#11784,#6559,.T.);
#14722=EDGE_CURVE('',#11784,#11784,#10006,.T.);
#14723=EDGE_CURVE('',#11782,#11785,#6560,.T.);
#14724=EDGE_CURVE('',#11785,#11785,#10007,.T.);
#14725=EDGE_CURVE('',#11766,#11786,#107,.T.);
#14726=EDGE_CURVE('',#11786,#11787,#10008,.T.);
#14727=EDGE_CURVE('',#11787,#11763,#108,.T.);
#14728=EDGE_CURVE('',#11788,#11786,#6561,.T.);
#14729=EDGE_CURVE('',#11789,#11788,#6562,.T.);
#14730=EDGE_CURVE('',#11789,#11787,#6563,.T.);
#14731=EDGE_CURVE('',#11765,#11790,#6564,.T.);
#14732=EDGE_CURVE('',#11790,#11788,#6565,.T.);
#14733=EDGE_CURVE('',#11791,#11789,#6566,.T.);
#14734=EDGE_CURVE('',#11791,#11764,#6567,.T.);
#14735=EDGE_CURVE('',#11790,#11791,#10009,.T.);
#14736=EDGE_CURVE('',#11792,#11792,#118,.T.);
#14737=EDGE_CURVE('',#11792,#11793,#6568,.T.);
#14738=EDGE_CURVE('',#11793,#11793,#119,.T.);
#14739=EDGE_CURVE('',#11794,#11794,#10010,.T.);
#14740=EDGE_CURVE('',#11794,#11795,#6569,.T.);
#14741=EDGE_CURVE('',#11795,#11795,#10011,.T.);
#14742=EDGE_CURVE('',#11796,#11796,#10012,.T.);
#14743=EDGE_CURVE('',#11796,#11797,#6570,.T.);
#14744=EDGE_CURVE('',#11797,#11797,#10013,.T.);
#14745=EDGE_CURVE('',#11798,#11798,#10014,.T.);
#14746=EDGE_CURVE('',#11798,#11799,#6571,.T.);
#14747=EDGE_CURVE('',#11799,#11799,#10015,.T.);
#14748=EDGE_CURVE('',#11800,#11800,#10016,.T.);
#14749=EDGE_CURVE('',#11800,#11801,#6572,.T.);
#14750=EDGE_CURVE('',#11801,#11801,#10017,.T.);
#14751=EDGE_CURVE('',#11802,#11802,#10018,.T.);
#14752=EDGE_CURVE('',#11802,#11803,#6573,.T.);
#14753=EDGE_CURVE('',#11803,#11803,#10019,.T.);
#14754=EDGE_CURVE('',#11804,#11804,#10020,.T.);
#14755=EDGE_CURVE('',#11804,#11805,#6574,.T.);
#14756=EDGE_CURVE('',#11805,#11805,#10021,.T.);
#14757=EDGE_CURVE('',#11806,#11806,#10022,.T.);
#14758=EDGE_CURVE('',#11806,#11807,#6575,.T.);
#14759=EDGE_CURVE('',#11807,#11807,#10023,.T.);
#14760=EDGE_CURVE('',#11808,#11808,#10024,.T.);
#14761=EDGE_CURVE('',#11808,#11809,#6576,.T.);
#14762=EDGE_CURVE('',#11809,#11809,#10025,.T.);
#14763=EDGE_CURVE('',#11810,#11810,#10026,.T.);
#14764=EDGE_CURVE('',#11810,#11811,#6577,.T.);
#14765=EDGE_CURVE('',#11811,#11811,#10027,.T.);
#14766=EDGE_CURVE('',#11812,#11812,#10028,.T.);
#14767=EDGE_CURVE('',#11812,#11813,#6578,.T.);
#14768=EDGE_CURVE('',#11813,#11813,#10029,.T.);
#14769=EDGE_CURVE('',#11814,#11814,#10030,.T.);
#14770=EDGE_CURVE('',#11814,#11815,#6579,.T.);
#14771=EDGE_CURVE('',#11815,#11815,#10031,.T.);
#14772=EDGE_CURVE('',#11816,#11816,#10032,.T.);
#14773=EDGE_CURVE('',#11816,#11817,#6580,.T.);
#14774=EDGE_CURVE('',#11817,#11817,#10033,.T.);
#14775=EDGE_CURVE('',#11818,#11818,#10034,.T.);
#14776=EDGE_CURVE('',#11818,#11806,#10035,.T.);
#14777=EDGE_CURVE('',#11819,#11820,#6581,.T.);
#14778=EDGE_CURVE('',#11821,#11820,#10036,.T.);
#14779=EDGE_CURVE('',#11821,#11822,#6582,.T.);
#14780=EDGE_CURVE('',#11819,#11822,#10037,.T.);
#14781=EDGE_CURVE('',#11823,#11820,#120,.T.);
#14782=EDGE_CURVE('',#11824,#11823,#10038,.T.);
#14783=EDGE_CURVE('',#11821,#11824,#121,.T.);
#14784=EDGE_CURVE('',#11819,#11825,#122,.T.);
#14785=EDGE_CURVE('',#11826,#11822,#123,.T.);
#14786=EDGE_CURVE('',#11825,#11826,#10039,.T.);
#14787=EDGE_CURVE('',#11827,#11826,#6583,.T.);
#14788=EDGE_CURVE('',#11828,#11827,#10040,.T.);
#14789=EDGE_CURVE('',#11825,#11828,#6584,.T.);
#14790=EDGE_CURVE('',#11824,#11829,#6585,.T.);
#14791=EDGE_CURVE('',#11830,#11823,#6586,.T.);
#14792=EDGE_CURVE('',#11829,#11830,#10041,.T.);
#14793=EDGE_CURVE('',#11831,#11830,#124,.T.);
#14794=EDGE_CURVE('',#11832,#11831,#10042,.T.);
#14795=EDGE_CURVE('',#11829,#11832,#125,.T.);
#14796=EDGE_CURVE('',#11828,#11833,#126,.T.);
#14797=EDGE_CURVE('',#11834,#11827,#127,.T.);
#14798=EDGE_CURVE('',#11833,#11834,#10043,.T.);
#14799=EDGE_CURVE('',#11833,#11831,#6587,.T.);
#14800=EDGE_CURVE('',#11832,#11834,#6588,.T.);
#14801=EDGE_CURVE('',#11835,#11835,#10044,.T.);
#14802=EDGE_CURVE('',#11835,#11836,#6589,.T.);
#14803=EDGE_CURVE('',#11836,#11836,#10045,.T.);
#14804=EDGE_CURVE('',#11837,#11837,#10046,.T.);
#14805=EDGE_CURVE('',#11837,#11838,#6590,.T.);
#14806=EDGE_CURVE('',#11838,#11838,#10047,.T.);
#14807=EDGE_CURVE('',#11839,#11839,#10048,.T.);
#14808=EDGE_CURVE('',#11839,#11840,#6591,.T.);
#14809=EDGE_CURVE('',#11840,#11840,#10049,.T.);
#14810=EDGE_CURVE('',#11841,#11841,#10050,.T.);
#14811=EDGE_CURVE('',#11841,#11842,#6592,.T.);
#14812=EDGE_CURVE('',#11842,#11842,#10051,.T.);
#14813=EDGE_CURVE('',#11843,#11843,#10052,.T.);
#14814=EDGE_CURVE('',#11843,#11844,#6593,.T.);
#14815=EDGE_CURVE('',#11844,#11844,#10053,.T.);
#14816=EDGE_CURVE('',#11845,#11845,#10054,.T.);
#14817=EDGE_CURVE('',#11845,#11846,#6594,.T.);
#14818=EDGE_CURVE('',#11846,#11846,#10055,.T.);
#14819=EDGE_CURVE('',#11847,#11847,#10056,.T.);
#14820=EDGE_CURVE('',#11847,#11848,#6595,.T.);
#14821=EDGE_CURVE('',#11848,#11848,#10057,.T.);
#14822=EDGE_CURVE('',#11849,#11850,#6596,.T.);
#14823=EDGE_CURVE('',#11851,#11850,#6597,.T.);
#14824=EDGE_CURVE('',#11852,#11851,#6598,.T.);
#14825=EDGE_CURVE('',#11852,#11849,#6599,.T.);
#14826=EDGE_CURVE('',#11850,#11853,#6600,.T.);
#14827=EDGE_CURVE('',#11854,#11853,#6601,.T.);
#14828=EDGE_CURVE('',#11851,#11854,#6602,.T.);
#14829=EDGE_CURVE('',#11853,#11855,#6603,.T.);
#14830=EDGE_CURVE('',#11856,#11855,#6604,.T.);
#14831=EDGE_CURVE('',#11854,#11856,#6605,.T.);
#14832=EDGE_CURVE('',#11855,#11857,#6606,.T.);
#14833=EDGE_CURVE('',#11858,#11857,#6607,.T.);
#14834=EDGE_CURVE('',#11856,#11858,#6608,.T.);
#14835=EDGE_CURVE('',#11857,#11859,#6609,.T.);
#14836=EDGE_CURVE('',#11860,#11859,#6610,.T.);
#14837=EDGE_CURVE('',#11858,#11860,#6611,.T.);
#14838=EDGE_CURVE('',#11859,#11861,#6612,.T.);
#14839=EDGE_CURVE('',#11862,#11861,#6613,.T.);
#14840=EDGE_CURVE('',#11860,#11862,#6614,.T.);
#14841=EDGE_CURVE('',#11861,#11863,#6615,.T.);
#14842=EDGE_CURVE('',#11864,#11863,#6616,.T.);
#14843=EDGE_CURVE('',#11862,#11864,#6617,.T.);
#14844=EDGE_CURVE('',#11863,#11865,#6618,.T.);
#14845=EDGE_CURVE('',#11866,#11865,#6619,.T.);
#14846=EDGE_CURVE('',#11864,#11866,#6620,.T.);
#14847=EDGE_CURVE('',#11865,#11867,#6621,.T.);
#14848=EDGE_CURVE('',#11868,#11867,#6622,.T.);
#14849=EDGE_CURVE('',#11866,#11868,#6623,.T.);
#14850=EDGE_CURVE('',#11867,#11869,#6624,.T.);
#14851=EDGE_CURVE('',#11870,#11869,#6625,.T.);
#14852=EDGE_CURVE('',#11868,#11870,#6626,.T.);
#14853=EDGE_CURVE('',#11869,#11871,#6627,.T.);
#14854=EDGE_CURVE('',#11872,#11871,#6628,.T.);
#14855=EDGE_CURVE('',#11870,#11872,#6629,.T.);
#14856=EDGE_CURVE('',#11871,#11849,#6630,.T.);
#14857=EDGE_CURVE('',#11872,#11852,#6631,.T.);
#14858=EDGE_CURVE('',#11873,#11873,#10058,.T.);
#14859=EDGE_CURVE('',#11873,#11874,#6632,.T.);
#14860=EDGE_CURVE('',#11874,#11874,#10059,.T.);
#14861=EDGE_CURVE('',#11875,#11875,#10060,.T.);
#14862=EDGE_CURVE('',#11875,#11876,#6633,.T.);
#14863=EDGE_CURVE('',#11876,#11876,#10061,.T.);
#14864=EDGE_CURVE('',#11877,#11878,#10062,.T.);
#14865=EDGE_CURVE('',#11877,#11879,#6634,.T.);
#14866=EDGE_CURVE('',#11879,#11880,#10063,.T.);
#14867=EDGE_CURVE('',#11878,#11880,#6635,.T.);
#14868=EDGE_CURVE('',#11881,#11882,#10064,.T.);
#14869=EDGE_CURVE('',#11881,#11883,#6636,.T.);
#14870=EDGE_CURVE('',#11883,#11884,#10065,.T.);
#14871=EDGE_CURVE('',#11882,#11884,#6637,.T.);
#14872=EDGE_CURVE('',#11885,#11886,#6638,.T.);
#14873=EDGE_CURVE('',#11886,#11887,#10066,.T.);
#14874=EDGE_CURVE('',#11887,#11888,#6639,.T.);
#14875=EDGE_CURVE('',#11888,#11881,#10067,.T.);
#14876=EDGE_CURVE('',#11882,#11889,#10068,.T.);
#14877=EDGE_CURVE('',#11889,#11890,#6640,.T.);
#14878=EDGE_CURVE('',#11890,#11891,#10069,.T.);
#14879=EDGE_CURVE('',#11891,#11892,#6641,.T.);
#14880=EDGE_CURVE('',#11892,#11877,#6642,.T.);
#14881=EDGE_CURVE('',#11878,#11885,#6643,.T.);
#14882=EDGE_CURVE('',#11893,#11894,#6644,.T.);
#14883=EDGE_CURVE('',#11880,#11893,#6645,.T.);
#14884=EDGE_CURVE('',#11895,#11879,#6646,.T.);
#14885=EDGE_CURVE('',#11896,#11895,#6647,.T.);
#14886=EDGE_CURVE('',#11897,#11896,#10070,.T.);
#14887=EDGE_CURVE('',#11898,#11897,#6648,.T.);
#14888=EDGE_CURVE('',#11884,#11898,#10071,.T.);
#14889=EDGE_CURVE('',#11899,#11883,#10072,.T.);
#14890=EDGE_CURVE('',#11900,#11899,#6649,.T.);
#14891=EDGE_CURVE('',#11894,#11900,#10073,.T.);
#14892=EDGE_CURVE('',#11886,#11894,#6650,.T.);
#14893=EDGE_CURVE('',#11885,#11893,#6651,.T.);
#14894=EDGE_CURVE('',#11887,#11900,#6652,.T.);
#14895=EDGE_CURVE('',#11888,#11899,#6653,.T.);
#14896=EDGE_CURVE('',#11889,#11898,#6654,.T.);
#14897=EDGE_CURVE('',#11890,#11897,#6655,.T.);
#14898=EDGE_CURVE('',#11891,#11896,#6656,.T.);
#14899=EDGE_CURVE('',#11892,#11895,#6657,.T.);
#14900=EDGE_CURVE('',#11901,#11901,#10074,.T.);
#14901=EDGE_CURVE('',#11901,#11902,#6658,.T.);
#14902=EDGE_CURVE('',#11902,#11902,#10075,.T.);
#14903=EDGE_CURVE('',#11903,#11903,#10076,.T.);
#14904=EDGE_CURVE('',#11903,#11904,#6659,.T.);
#14905=EDGE_CURVE('',#11904,#11904,#10077,.T.);
#14906=EDGE_CURVE('',#11905,#11905,#10078,.T.);
#14907=EDGE_CURVE('',#11905,#11906,#6660,.T.);
#14908=EDGE_CURVE('',#11906,#11906,#10079,.T.);
#14909=EDGE_CURVE('',#11907,#11907,#10080,.T.);
#14910=EDGE_CURVE('',#11907,#11908,#6661,.T.);
#14911=EDGE_CURVE('',#11908,#11908,#10081,.T.);
#14912=EDGE_CURVE('',#11909,#11909,#10082,.T.);
#14913=EDGE_CURVE('',#11909,#11910,#6662,.T.);
#14914=EDGE_CURVE('',#11910,#11910,#10083,.T.);
#14915=EDGE_CURVE('',#11911,#11911,#10084,.T.);
#14916=EDGE_CURVE('',#11911,#11912,#6663,.T.);
#14917=EDGE_CURVE('',#11912,#11912,#10085,.T.);
#14918=EDGE_CURVE('',#11913,#11913,#10086,.T.);
#14919=EDGE_CURVE('',#11913,#11914,#6664,.T.);
#14920=EDGE_CURVE('',#11914,#11914,#10087,.T.);
#14921=EDGE_CURVE('',#11915,#11915,#10088,.T.);
#14922=EDGE_CURVE('',#11915,#11916,#6665,.T.);
#14923=EDGE_CURVE('',#11916,#11916,#10089,.T.);
#14924=EDGE_CURVE('',#11917,#11917,#10090,.T.);
#14925=EDGE_CURVE('',#11917,#11918,#6666,.T.);
#14926=EDGE_CURVE('',#11918,#11918,#10091,.T.);
#14927=EDGE_CURVE('',#11919,#11919,#10092,.T.);
#14928=EDGE_CURVE('',#11919,#11920,#6667,.T.);
#14929=EDGE_CURVE('',#11920,#11920,#10093,.T.);
#14930=EDGE_CURVE('',#11921,#11921,#10094,.T.);
#14931=EDGE_CURVE('',#11921,#11922,#6668,.T.);
#14932=EDGE_CURVE('',#11922,#11922,#10095,.T.);
#14933=EDGE_CURVE('',#11923,#11923,#10096,.T.);
#14934=EDGE_CURVE('',#11923,#11924,#6669,.T.);
#14935=EDGE_CURVE('',#11924,#11924,#10097,.T.);
#14936=EDGE_CURVE('',#11925,#11925,#10098,.T.);
#14937=EDGE_CURVE('',#11925,#11926,#6670,.T.);
#14938=EDGE_CURVE('',#11926,#11926,#10099,.T.);
#14939=EDGE_CURVE('',#11927,#11927,#10100,.T.);
#14940=EDGE_CURVE('',#11927,#11928,#6671,.T.);
#14941=EDGE_CURVE('',#11928,#11928,#10101,.T.);
#14942=EDGE_CURVE('',#11929,#11929,#10102,.T.);
#14943=EDGE_CURVE('',#11929,#11930,#6672,.T.);
#14944=EDGE_CURVE('',#11930,#11930,#10103,.T.);
#14945=EDGE_CURVE('',#11931,#11931,#10104,.T.);
#14946=EDGE_CURVE('',#11931,#11932,#6673,.T.);
#14947=EDGE_CURVE('',#11932,#11932,#10105,.T.);
#14948=EDGE_CURVE('',#11933,#11933,#10106,.T.);
#14949=EDGE_CURVE('',#11933,#11934,#6674,.T.);
#14950=EDGE_CURVE('',#11934,#11934,#10107,.T.);
#14951=EDGE_CURVE('',#11935,#11935,#10108,.T.);
#14952=EDGE_CURVE('',#11935,#11936,#6675,.T.);
#14953=EDGE_CURVE('',#11936,#11936,#10109,.T.);
#14954=EDGE_CURVE('',#11937,#11937,#10110,.T.);
#14955=EDGE_CURVE('',#11937,#11938,#6676,.T.);
#14956=EDGE_CURVE('',#11938,#11938,#10111,.T.);
#14957=EDGE_CURVE('',#11939,#11939,#10112,.T.);
#14958=EDGE_CURVE('',#11939,#11940,#6677,.T.);
#14959=EDGE_CURVE('',#11940,#11940,#10113,.T.);
#14960=EDGE_CURVE('',#11941,#11941,#10114,.T.);
#14961=EDGE_CURVE('',#11941,#11942,#6678,.T.);
#14962=EDGE_CURVE('',#11942,#11942,#10115,.T.);
#14963=EDGE_CURVE('',#11943,#11944,#6679,.T.);
#14964=EDGE_CURVE('',#11944,#11945,#6680,.T.);
#14965=EDGE_CURVE('',#11945,#11946,#6681,.T.);
#14966=EDGE_CURVE('',#11946,#11947,#6682,.T.);
#14967=EDGE_CURVE('',#11947,#11948,#6683,.T.);
#14968=EDGE_CURVE('',#11948,#11949,#6684,.T.);
#14969=EDGE_CURVE('',#11949,#11950,#6685,.T.);
#14970=EDGE_CURVE('',#11950,#11951,#6686,.T.);
#14971=EDGE_CURVE('',#11951,#11952,#6687,.T.);
#14972=EDGE_CURVE('',#11952,#11953,#6688,.T.);
#14973=EDGE_CURVE('',#11953,#11954,#6689,.T.);
#14974=EDGE_CURVE('',#11954,#11943,#6690,.T.);
#14975=EDGE_CURVE('',#11955,#11956,#6691,.T.);
#14976=EDGE_CURVE('',#11957,#11955,#6692,.T.);
#14977=EDGE_CURVE('',#11958,#11957,#6693,.T.);
#14978=EDGE_CURVE('',#11959,#11958,#6694,.T.);
#14979=EDGE_CURVE('',#11960,#11959,#6695,.T.);
#14980=EDGE_CURVE('',#11961,#11960,#6696,.T.);
#14981=EDGE_CURVE('',#11962,#11961,#6697,.T.);
#14982=EDGE_CURVE('',#11956,#11962,#6698,.T.);
#14983=EDGE_CURVE('',#11963,#11964,#6699,.T.);
#14984=EDGE_CURVE('',#11944,#11964,#6700,.T.);
#14985=EDGE_CURVE('',#11943,#11963,#6701,.T.);
#14986=EDGE_CURVE('',#11964,#11965,#6702,.T.);
#14987=EDGE_CURVE('',#11945,#11965,#6703,.T.);
#14988=EDGE_CURVE('',#11965,#11966,#6704,.T.);
#14989=EDGE_CURVE('',#11946,#11966,#6705,.T.);
#14990=EDGE_CURVE('',#11966,#11967,#6706,.T.);
#14991=EDGE_CURVE('',#11947,#11967,#6707,.T.);
#14992=EDGE_CURVE('',#11967,#11968,#6708,.T.);
#14993=EDGE_CURVE('',#11948,#11968,#6709,.T.);
#14994=EDGE_CURVE('',#11968,#11969,#6710,.T.);
#14995=EDGE_CURVE('',#11949,#11969,#6711,.T.);
#14996=EDGE_CURVE('',#11969,#11970,#6712,.T.);
#14997=EDGE_CURVE('',#11950,#11970,#6713,.T.);
#14998=EDGE_CURVE('',#11970,#11971,#6714,.T.);
#14999=EDGE_CURVE('',#11951,#11971,#6715,.T.);
#15000=EDGE_CURVE('',#11971,#11972,#6716,.T.);
#15001=EDGE_CURVE('',#11952,#11972,#6717,.T.);
#15002=EDGE_CURVE('',#11972,#11973,#6718,.T.);
#15003=EDGE_CURVE('',#11953,#11973,#6719,.T.);
#15004=EDGE_CURVE('',#11973,#11974,#6720,.T.);
#15005=EDGE_CURVE('',#11954,#11974,#6721,.T.);
#15006=EDGE_CURVE('',#11974,#11963,#6722,.T.);
#15007=EDGE_CURVE('',#11975,#11976,#6723,.T.);
#15008=EDGE_CURVE('',#11976,#11977,#6724,.T.);
#15009=EDGE_CURVE('',#11977,#11978,#6725,.T.);
#15010=EDGE_CURVE('',#11978,#11979,#6726,.T.);
#15011=EDGE_CURVE('',#11979,#11980,#6727,.T.);
#15012=EDGE_CURVE('',#11980,#11981,#6728,.T.);
#15013=EDGE_CURVE('',#11981,#11982,#6729,.T.);
#15014=EDGE_CURVE('',#11982,#11975,#6730,.T.);
#15015=EDGE_CURVE('',#11976,#11955,#6731,.T.);
#15016=EDGE_CURVE('',#11975,#11957,#6732,.T.);
#15017=EDGE_CURVE('',#11977,#11956,#6733,.T.);
#15018=EDGE_CURVE('',#11978,#11962,#6734,.T.);
#15019=EDGE_CURVE('',#11979,#11961,#6735,.T.);
#15020=EDGE_CURVE('',#11980,#11960,#6736,.T.);
#15021=EDGE_CURVE('',#11981,#11959,#6737,.T.);
#15022=EDGE_CURVE('',#11982,#11958,#6738,.T.);
#15023=EDGE_CURVE('',#11983,#11984,#6739,.T.);
#15024=EDGE_CURVE('',#11985,#11983,#6740,.T.);
#15025=EDGE_CURVE('',#11986,#11985,#6741,.T.);
#15026=EDGE_CURVE('',#11987,#11986,#6742,.T.);
#15027=EDGE_CURVE('',#11988,#11987,#6743,.T.);
#15028=EDGE_CURVE('',#11984,#11988,#6744,.T.);
#15029=EDGE_CURVE('',#11989,#11990,#6745,.T.);
#15030=EDGE_CURVE('',#11991,#11989,#6746,.T.);
#15031=EDGE_CURVE('',#11992,#11991,#6747,.T.);
#15032=EDGE_CURVE('',#11993,#11992,#6748,.T.);
#15033=EDGE_CURVE('',#11994,#11993,#6749,.T.);
#15034=EDGE_CURVE('',#11990,#11994,#6750,.T.);
#15035=EDGE_CURVE('',#11995,#11996,#6751,.T.);
#15036=EDGE_CURVE('',#11997,#11995,#6752,.T.);
#15037=EDGE_CURVE('',#11998,#11997,#6753,.T.);
#15038=EDGE_CURVE('',#11999,#11998,#6754,.T.);
#15039=EDGE_CURVE('',#12000,#11999,#6755,.T.);
#15040=EDGE_CURVE('',#11996,#12000,#6756,.T.);
#15041=EDGE_CURVE('',#12001,#12002,#6757,.T.);
#15042=EDGE_CURVE('',#12003,#12001,#6758,.T.);
#15043=EDGE_CURVE('',#12004,#12003,#6759,.T.);
#15044=EDGE_CURVE('',#12005,#12004,#6760,.T.);
#15045=EDGE_CURVE('',#12006,#12005,#6761,.T.);
#15046=EDGE_CURVE('',#12002,#12006,#6762,.T.);
#15047=EDGE_CURVE('',#12007,#11984,#6763,.T.);
#15048=EDGE_CURVE('',#12008,#12007,#6764,.T.);
#15049=EDGE_CURVE('',#12008,#11983,#6765,.T.);
#15050=EDGE_CURVE('',#12009,#12008,#6766,.T.);
#15051=EDGE_CURVE('',#12009,#11985,#6767,.T.);
#15052=EDGE_CURVE('',#12010,#12009,#6768,.T.);
#15053=EDGE_CURVE('',#12010,#11986,#6769,.T.);
#15054=EDGE_CURVE('',#12011,#12010,#6770,.T.);
#15055=EDGE_CURVE('',#12011,#11987,#6771,.T.);
#15056=EDGE_CURVE('',#12012,#12011,#6772,.T.);
#15057=EDGE_CURVE('',#12012,#11988,#6773,.T.);
#15058=EDGE_CURVE('',#12007,#12012,#6774,.T.);
#15059=EDGE_CURVE('',#12013,#11990,#6775,.T.);
#15060=EDGE_CURVE('',#12014,#12013,#6776,.T.);
#15061=EDGE_CURVE('',#12014,#11989,#6777,.T.);
#15062=EDGE_CURVE('',#12015,#12014,#6778,.T.);
#15063=EDGE_CURVE('',#12015,#11991,#6779,.T.);
#15064=EDGE_CURVE('',#12016,#12015,#6780,.T.);
#15065=EDGE_CURVE('',#12016,#11992,#6781,.T.);
#15066=EDGE_CURVE('',#12017,#12016,#6782,.T.);
#15067=EDGE_CURVE('',#12017,#11993,#6783,.T.);
#15068=EDGE_CURVE('',#12018,#12017,#6784,.T.);
#15069=EDGE_CURVE('',#12018,#11994,#6785,.T.);
#15070=EDGE_CURVE('',#12013,#12018,#6786,.T.);
#15071=EDGE_CURVE('',#12019,#12002,#6787,.T.);
#15072=EDGE_CURVE('',#12020,#12019,#6788,.T.);
#15073=EDGE_CURVE('',#12020,#12001,#6789,.T.);
#15074=EDGE_CURVE('',#12021,#12020,#6790,.T.);
#15075=EDGE_CURVE('',#12021,#12003,#6791,.T.);
#15076=EDGE_CURVE('',#12022,#12021,#6792,.T.);
#15077=EDGE_CURVE('',#12022,#12004,#6793,.T.);
#15078=EDGE_CURVE('',#12023,#12022,#6794,.T.);
#15079=EDGE_CURVE('',#12023,#12005,#6795,.T.);
#15080=EDGE_CURVE('',#12024,#12023,#6796,.T.);
#15081=EDGE_CURVE('',#12024,#12006,#6797,.T.);
#15082=EDGE_CURVE('',#12019,#12024,#6798,.T.);
#15083=EDGE_CURVE('',#12025,#11996,#6799,.T.);
#15084=EDGE_CURVE('',#12026,#12025,#6800,.T.);
#15085=EDGE_CURVE('',#12026,#11995,#6801,.T.);
#15086=EDGE_CURVE('',#12027,#12026,#6802,.T.);
#15087=EDGE_CURVE('',#12027,#11997,#6803,.T.);
#15088=EDGE_CURVE('',#12028,#12027,#6804,.T.);
#15089=EDGE_CURVE('',#12028,#11998,#6805,.T.);
#15090=EDGE_CURVE('',#12029,#12028,#6806,.T.);
#15091=EDGE_CURVE('',#12029,#11999,#6807,.T.);
#15092=EDGE_CURVE('',#12030,#12029,#6808,.T.);
#15093=EDGE_CURVE('',#12030,#12000,#6809,.T.);
#15094=EDGE_CURVE('',#12025,#12030,#6810,.T.);
#15095=EDGE_CURVE('',#12031,#12032,#6811,.T.);
#15096=EDGE_CURVE('',#12033,#12032,#10116,.T.);
#15097=EDGE_CURVE('',#12034,#12033,#10117,.T.);
#15098=EDGE_CURVE('',#12035,#12034,#10118,.T.);
#15099=EDGE_CURVE('',#12036,#12035,#10119,.T.);
#15100=EDGE_CURVE('',#12037,#12036,#10120,.T.);
#15101=EDGE_CURVE('',#12032,#12037,#10121,.T.);
#15102=EDGE_CURVE('',#12038,#12039,#128,.T.);
#15103=EDGE_CURVE('',#12039,#12040,#6812,.T.);
#15104=EDGE_CURVE('',#12040,#12040,#10122,.T.);
#15105=EDGE_CURVE('',#12039,#12038,#129,.T.);
#15106=EDGE_CURVE('',#12040,#12041,#6813,.T.);
#15107=EDGE_CURVE('',#12041,#12042,#130,.T.);
#15108=EDGE_CURVE('',#12042,#12041,#131,.T.);
#15109=EDGE_CURVE('',#12043,#12044,#10123,.T.);
#15110=EDGE_CURVE('',#12044,#12045,#6814,.T.);
#15111=EDGE_CURVE('',#12045,#12045,#10124,.T.);
#15112=EDGE_CURVE('',#12044,#12043,#10125,.T.);
#15113=EDGE_CURVE('',#12043,#12046,#6815,.T.);
#15114=EDGE_CURVE('',#12046,#12047,#132,.T.);
#15115=EDGE_CURVE('',#12047,#12046,#133,.T.);
#15116=EDGE_CURVE('',#12048,#12049,#10126,.T.);
#15117=EDGE_CURVE('',#12049,#12050,#6816,.T.);
#15118=EDGE_CURVE('',#12050,#12050,#10127,.T.);
#15119=EDGE_CURVE('',#12049,#12048,#10128,.T.);
#15120=EDGE_CURVE('',#12051,#12051,#10129,.T.);
#15121=EDGE_CURVE('',#12051,#12052,#6817,.T.);
#15122=EDGE_CURVE('',#12052,#12052,#10130,.T.);
#15123=EDGE_CURVE('',#12053,#12054,#10131,.T.);
#15124=EDGE_CURVE('',#12054,#12055,#6818,.T.);
#15125=EDGE_CURVE('',#12056,#12055,#10132,.T.);
#15126=EDGE_CURVE('',#12056,#12053,#6819,.T.);
#15127=EDGE_CURVE('',#12057,#12057,#10133,.T.);
#15128=EDGE_CURVE('',#12057,#12058,#6820,.T.);
#15129=EDGE_CURVE('',#12058,#12058,#10134,.T.);
#15130=EDGE_CURVE('',#12048,#12051,#6821,.T.);
#15131=EDGE_CURVE('',#12059,#12060,#10135,.T.);
#15132=EDGE_CURVE('',#12060,#12061,#10136,.T.);
#15133=EDGE_CURVE('',#12061,#12062,#10137,.T.);
#15134=EDGE_CURVE('',#12062,#12063,#10138,.T.);
#15135=EDGE_CURVE('',#12063,#12064,#10139,.T.);
#15136=EDGE_CURVE('',#12064,#12059,#10140,.T.);
#15137=EDGE_CURVE('',#12065,#12066,#10141,.T.);
#15138=EDGE_CURVE('',#12066,#12067,#6822,.T.);
#15139=EDGE_CURVE('',#12068,#12067,#10142,.T.);
#15140=EDGE_CURVE('',#12068,#12065,#6823,.T.);
#15141=EDGE_CURVE('',#12069,#12070,#10143,.T.);
#15142=EDGE_CURVE('',#12070,#12071,#6824,.T.);
#15143=EDGE_CURVE('',#12072,#12071,#10144,.T.);
#15144=EDGE_CURVE('',#12072,#12069,#6825,.T.);
#15145=EDGE_CURVE('',#12073,#12074,#10145,.T.);
#15146=EDGE_CURVE('',#12074,#12075,#6826,.T.);
#15147=EDGE_CURVE('',#12076,#12075,#10146,.T.);
#15148=EDGE_CURVE('',#12076,#12073,#6827,.T.);
#15149=EDGE_CURVE('',#12071,#12056,#6828,.T.);
#15150=EDGE_CURVE('',#12055,#12068,#6829,.T.);
#15151=EDGE_CURVE('',#12067,#12076,#6830,.T.);
#15152=EDGE_CURVE('',#12075,#12072,#6831,.T.);
#15153=EDGE_CURVE('',#12053,#12070,#6832,.T.);
#15154=EDGE_CURVE('',#12069,#12074,#6833,.T.);
#15155=EDGE_CURVE('',#12073,#12066,#6834,.T.);
#15156=EDGE_CURVE('',#12065,#12054,#6835,.T.);
#15157=EDGE_CURVE('',#12077,#12060,#6836,.T.);
#15158=EDGE_CURVE('',#12037,#12077,#6837,.T.);
#15159=EDGE_CURVE('',#12078,#12037,#6838,.T.);
#15160=EDGE_CURVE('',#12078,#12061,#6839,.T.);
#15161=EDGE_CURVE('',#12036,#12078,#6840,.T.);
#15162=EDGE_CURVE('',#12079,#12036,#6841,.T.);
#15163=EDGE_CURVE('',#12079,#12062,#6842,.T.);
#15164=EDGE_CURVE('',#12035,#12079,#6843,.T.);
#15165=EDGE_CURVE('',#12080,#12035,#6844,.T.);
#15166=EDGE_CURVE('',#12080,#12063,#6845,.T.);
#15167=EDGE_CURVE('',#12034,#12080,#6846,.T.);
#15168=EDGE_CURVE('',#12081,#12034,#6847,.T.);
#15169=EDGE_CURVE('',#12081,#12064,#6848,.T.);
#15170=EDGE_CURVE('',#12033,#12081,#6849,.T.);
#15171=EDGE_CURVE('',#12082,#12033,#6850,.T.);
#15172=EDGE_CURVE('',#12082,#12059,#6851,.T.);
#15173=EDGE_CURVE('',#12032,#12082,#6852,.T.);
#15174=EDGE_CURVE('',#12077,#12032,#6853,.T.);
#15175=EDGE_CURVE('',#12083,#12083,#10147,.T.);
#15176=EDGE_CURVE('',#12083,#12084,#6854,.T.);
#15177=EDGE_CURVE('',#12084,#12084,#10148,.T.);
#15178=EDGE_CURVE('',#12085,#12085,#10149,.T.);
#15179=EDGE_CURVE('',#12085,#12086,#6855,.T.);
#15180=EDGE_CURVE('',#12086,#12086,#10150,.T.);
#15181=EDGE_CURVE('',#12087,#12087,#10151,.T.);
#15182=EDGE_CURVE('',#12087,#12088,#6856,.T.);
#15183=EDGE_CURVE('',#12088,#12088,#10152,.T.);
#15184=EDGE_CURVE('',#12089,#12089,#10153,.T.);
#15185=EDGE_CURVE('',#12089,#12090,#6857,.T.);
#15186=EDGE_CURVE('',#12090,#12090,#10154,.T.);
#15187=EDGE_CURVE('',#12091,#12091,#10155,.T.);
#15188=EDGE_CURVE('',#12091,#12092,#6858,.T.);
#15189=EDGE_CURVE('',#12092,#12092,#10156,.T.);
#15190=EDGE_CURVE('',#12093,#12093,#10157,.T.);
#15191=EDGE_CURVE('',#12093,#12094,#6859,.T.);
#15192=EDGE_CURVE('',#12094,#12094,#10158,.T.);
#15193=EDGE_CURVE('',#12095,#12095,#10159,.T.);
#15194=EDGE_CURVE('',#12095,#12096,#6860,.T.);
#15195=EDGE_CURVE('',#12096,#12096,#10160,.T.);
#15196=EDGE_CURVE('',#12097,#12097,#10161,.T.);
#15197=EDGE_CURVE('',#12097,#12098,#6861,.T.);
#15198=EDGE_CURVE('',#12098,#12098,#10162,.T.);
#15199=EDGE_CURVE('',#12099,#12100,#6862,.T.);
#15200=EDGE_CURVE('',#12101,#12099,#6863,.T.);
#15201=EDGE_CURVE('',#12101,#12102,#6864,.T.);
#15202=EDGE_CURVE('',#12102,#12100,#6865,.T.);
#15203=EDGE_CURVE('',#12103,#12101,#6866,.T.);
#15204=EDGE_CURVE('',#12104,#12103,#6867,.T.);
#15205=EDGE_CURVE('',#12104,#12105,#6868,.T.);
#15206=EDGE_CURVE('',#12105,#12106,#6869,.T.);
#15207=EDGE_CURVE('',#12102,#12106,#6870,.T.);
#15208=EDGE_CURVE('',#12107,#12108,#6871,.T.);
#15209=EDGE_CURVE('',#12107,#12100,#6872,.T.);
#15210=EDGE_CURVE('',#12106,#12109,#6873,.T.);
#15211=EDGE_CURVE('',#12108,#12109,#6874,.T.);
#15212=EDGE_CURVE('',#12110,#12111,#6875,.T.);
#15213=EDGE_CURVE('',#12112,#12110,#6876,.T.);
#15214=EDGE_CURVE('',#12108,#12112,#6877,.T.);
#15215=EDGE_CURVE('',#12109,#12113,#6878,.T.);
#15216=EDGE_CURVE('',#12111,#12113,#6879,.T.);
#15217=EDGE_CURVE('',#12114,#12104,#6880,.T.);
#15218=EDGE_CURVE('',#12114,#12115,#6881,.T.);
#15219=EDGE_CURVE('',#12111,#12115,#6882,.T.);
#15220=EDGE_CURVE('',#12113,#12105,#6883,.T.);
#15221=EDGE_CURVE('',#12116,#12115,#6884,.T.);
#15222=EDGE_CURVE('',#12110,#12116,#6885,.T.);
#15223=EDGE_CURVE('',#12117,#12107,#6886,.T.);
#15224=EDGE_CURVE('',#12117,#12099,#6887,.T.);
#15225=EDGE_CURVE('',#12103,#12117,#6888,.T.);
#15226=EDGE_CURVE('',#12118,#12114,#6889,.T.);
#15227=EDGE_CURVE('',#12118,#12116,#6890,.T.);
#15228=EDGE_CURVE('',#12112,#12118,#6891,.T.);
#15229=EDGE_CURVE('',#12119,#12119,#10163,.T.);
#15230=EDGE_CURVE('',#12119,#12120,#6892,.T.);
#15231=EDGE_CURVE('',#12120,#12120,#10164,.T.);
#15232=EDGE_CURVE('',#12121,#12121,#10165,.T.);
#15233=EDGE_CURVE('',#12122,#12122,#10166,.T.);
#15234=EDGE_CURVE('',#12122,#12121,#6893,.T.);
#15235=EDGE_CURVE('',#12123,#12124,#10167,.T.);
#15236=EDGE_CURVE('',#12125,#12124,#134,.T.);
#15237=EDGE_CURVE('',#12126,#12125,#135,.T.);
#15238=EDGE_CURVE('',#12126,#12123,#136,.T.);
#15239=EDGE_CURVE('',#12127,#12126,#137,.T.);
#15240=EDGE_CURVE('',#12127,#12128,#10168,.T.);
#15241=EDGE_CURVE('',#12128,#12123,#138,.T.);
#15242=EDGE_CURVE('',#12129,#12130,#10169,.T.);
#15243=EDGE_CURVE('',#12130,#12131,#10170,.T.);
#15244=EDGE_CURVE('',#12131,#12127,#10171,.T.);
#15245=EDGE_CURVE('',#12129,#12127,#10172,.T.);
#15246=EDGE_CURVE('',#12128,#12131,#10173,.T.);
#15247=EDGE_CURVE('',#12132,#12131,#139,.T.);
#15248=EDGE_CURVE('',#12132,#12133,#10174,.T.);
#15249=EDGE_CURVE('',#12133,#12128,#140,.T.);
#15250=EDGE_CURVE('',#12133,#12134,#141,.T.);
#15251=EDGE_CURVE('',#12123,#12134,#142,.T.);
#15252=EDGE_CURVE('',#12134,#12135,#143,.T.);
#15253=EDGE_CURVE('',#12124,#12135,#144,.T.);
#15254=EDGE_CURVE('',#12136,#12137,#145,.T.);
#15255=EDGE_CURVE('',#12135,#12137,#146,.T.);
#15256=EDGE_CURVE('',#12134,#12136,#147,.T.);
#15257=EDGE_CURVE('',#12133,#12138,#10175,.T.);
#15258=EDGE_CURVE('',#12138,#12136,#148,.T.);
#15259=EDGE_CURVE('',#12138,#12132,#10176,.T.);
#15260=EDGE_CURVE('',#12139,#12140,#149,.T.);
#15261=EDGE_CURVE('',#12141,#12140,#150,.T.);
#15262=EDGE_CURVE('',#12142,#12141,#151,.T.);
#15263=EDGE_CURVE('',#12142,#12139,#152,.T.);
#15264=EDGE_CURVE('',#12142,#12143,#153,.T.);
#15265=EDGE_CURVE('',#12143,#12144,#10177,.T.);
#15266=EDGE_CURVE('',#12139,#12144,#154,.T.);
#15267=EDGE_CURVE('',#12144,#12145,#10178,.T.);
#15268=EDGE_CURVE('',#12145,#12143,#10179,.T.);
#15269=EDGE_CURVE('',#12145,#12132,#10180,.T.);
#15270=EDGE_CURVE('',#12143,#12138,#10181,.T.);
#15271=EDGE_CURVE('',#12145,#12130,#155,.T.);
#15272=EDGE_CURVE('',#12130,#12146,#10182,.T.);
#15273=EDGE_CURVE('',#12144,#12146,#156,.T.);
#15274=EDGE_CURVE('',#12146,#12129,#10183,.T.);
#15275=EDGE_CURVE('',#12147,#12148,#157,.T.);
#15276=EDGE_CURVE('',#12149,#12148,#158,.T.);
#15277=EDGE_CURVE('',#12150,#12149,#10184,.T.);
#15278=EDGE_CURVE('',#12150,#12147,#159,.T.);
#15279=EDGE_CURVE('',#12147,#12129,#160,.T.);
#15280=EDGE_CURVE('',#12150,#12146,#161,.T.);
#15281=EDGE_CURVE('',#12139,#12150,#162,.T.);
#15282=EDGE_CURVE('',#12140,#12149,#163,.T.);
#15283=EDGE_CURVE('',#12151,#12152,#164,.T.);
#15284=EDGE_CURVE('',#12153,#12152,#165,.T.);
#15285=EDGE_CURVE('',#12154,#12153,#166,.T.);
#15286=EDGE_CURVE('',#12154,#12151,#167,.T.);
#15287=EDGE_CURVE('',#12155,#12154,#168,.T.);
#15288=EDGE_CURVE('',#12155,#12156,#10185,.T.);
#15289=EDGE_CURVE('',#12156,#12151,#169,.T.);
#15290=EDGE_CURVE('',#12157,#12158,#10186,.T.);
#15291=EDGE_CURVE('',#12158,#12159,#10187,.T.);
#15292=EDGE_CURVE('',#12159,#12155,#10188,.T.);
#15293=EDGE_CURVE('',#12157,#12155,#10189,.T.);
#15294=EDGE_CURVE('',#12156,#12159,#10190,.T.);
#15295=EDGE_CURVE('',#12160,#12159,#170,.T.);
#15296=EDGE_CURVE('',#12160,#12161,#10191,.T.);
#15297=EDGE_CURVE('',#12161,#12156,#171,.T.);
#15298=EDGE_CURVE('',#12161,#12162,#172,.T.);
#15299=EDGE_CURVE('',#12151,#12162,#173,.T.);
#15300=EDGE_CURVE('',#12162,#12163,#10192,.T.);
#15301=EDGE_CURVE('',#12152,#12163,#174,.T.);
#15302=EDGE_CURVE('',#12164,#12165,#175,.T.);
#15303=EDGE_CURVE('',#12163,#12165,#176,.T.);
#15304=EDGE_CURVE('',#12162,#12164,#177,.T.);
#15305=EDGE_CURVE('',#12161,#12166,#10193,.T.);
#15306=EDGE_CURVE('',#12166,#12164,#178,.T.);
#15307=EDGE_CURVE('',#12166,#12160,#10194,.T.);
#15308=EDGE_CURVE('',#12167,#12168,#179,.T.);
#15309=EDGE_CURVE('',#12169,#12168,#180,.T.);
#15310=EDGE_CURVE('',#12170,#12169,#181,.T.);
#15311=EDGE_CURVE('',#12170,#12167,#182,.T.);
#15312=EDGE_CURVE('',#12170,#12171,#183,.T.);
#15313=EDGE_CURVE('',#12171,#12172,#10195,.T.);
#15314=EDGE_CURVE('',#12167,#12172,#184,.T.);
#15315=EDGE_CURVE('',#12172,#12173,#10196,.T.);
#15316=EDGE_CURVE('',#12173,#12171,#10197,.T.);
#15317=EDGE_CURVE('',#12173,#12160,#10198,.T.);
#15318=EDGE_CURVE('',#12171,#12166,#10199,.T.);
#15319=EDGE_CURVE('',#12173,#12158,#185,.T.);
#15320=EDGE_CURVE('',#12158,#12174,#10200,.T.);
#15321=EDGE_CURVE('',#12172,#12174,#186,.T.);
#15322=EDGE_CURVE('',#12174,#12157,#10201,.T.);
#15323=EDGE_CURVE('',#12175,#12176,#187,.T.);
#15324=EDGE_CURVE('',#12177,#12176,#188,.T.);
#15325=EDGE_CURVE('',#12178,#12177,#10202,.T.);
#15326=EDGE_CURVE('',#12178,#12175,#189,.T.);
#15327=EDGE_CURVE('',#12175,#12157,#190,.T.);
#15328=EDGE_CURVE('',#12178,#12174,#191,.T.);
#15329=EDGE_CURVE('',#12167,#12178,#192,.T.);
#15330=EDGE_CURVE('',#12168,#12177,#193,.T.);
#15331=EDGE_CURVE('',#12179,#12180,#194,.T.);
#15332=EDGE_CURVE('',#12181,#12180,#195,.T.);
#15333=EDGE_CURVE('',#12182,#12181,#196,.T.);
#15334=EDGE_CURVE('',#12182,#12179,#197,.T.);
#15335=EDGE_CURVE('',#12183,#12182,#198,.T.);
#15336=EDGE_CURVE('',#12183,#12184,#10203,.T.);
#15337=EDGE_CURVE('',#12184,#12179,#199,.T.);
#15338=EDGE_CURVE('',#12185,#12186,#10204,.T.);
#15339=EDGE_CURVE('',#12186,#12187,#10205,.T.);
#15340=EDGE_CURVE('',#12187,#12183,#10206,.T.);
#15341=EDGE_CURVE('',#12185,#12183,#10207,.T.);
#15342=EDGE_CURVE('',#12184,#12187,#10208,.T.);
#15343=EDGE_CURVE('',#12188,#12187,#200,.T.);
#15344=EDGE_CURVE('',#12188,#12189,#10209,.T.);
#15345=EDGE_CURVE('',#12189,#12184,#201,.T.);
#15346=EDGE_CURVE('',#12189,#12190,#202,.T.);
#15347=EDGE_CURVE('',#12179,#12190,#203,.T.);
#15348=EDGE_CURVE('',#12190,#12191,#204,.T.);
#15349=EDGE_CURVE('',#12180,#12191,#205,.T.);
#15350=EDGE_CURVE('',#12192,#12193,#206,.T.);
#15351=EDGE_CURVE('',#12191,#12193,#207,.T.);
#15352=EDGE_CURVE('',#12190,#12192,#208,.T.);
#15353=EDGE_CURVE('',#12189,#12194,#10210,.T.);
#15354=EDGE_CURVE('',#12194,#12192,#209,.T.);
#15355=EDGE_CURVE('',#12194,#12188,#10211,.T.);
#15356=EDGE_CURVE('',#12195,#12196,#210,.T.);
#15357=EDGE_CURVE('',#12197,#12196,#211,.T.);
#15358=EDGE_CURVE('',#12198,#12197,#212,.T.);
#15359=EDGE_CURVE('',#12198,#12195,#213,.T.);
#15360=EDGE_CURVE('',#12198,#12199,#214,.T.);
#15361=EDGE_CURVE('',#12199,#12200,#10212,.T.);
#15362=EDGE_CURVE('',#12195,#12200,#215,.T.);
#15363=EDGE_CURVE('',#12200,#12201,#10213,.T.);
#15364=EDGE_CURVE('',#12201,#12199,#10214,.T.);
#15365=EDGE_CURVE('',#12201,#12188,#10215,.T.);
#15366=EDGE_CURVE('',#12199,#12194,#10216,.T.);
#15367=EDGE_CURVE('',#12201,#12186,#216,.T.);
#15368=EDGE_CURVE('',#12186,#12202,#10217,.T.);
#15369=EDGE_CURVE('',#12200,#12202,#217,.T.);
#15370=EDGE_CURVE('',#12202,#12185,#10218,.T.);
#15371=EDGE_CURVE('',#12203,#12204,#218,.T.);
#15372=EDGE_CURVE('',#12205,#12204,#219,.T.);
#15373=EDGE_CURVE('',#12206,#12205,#10219,.T.);
#15374=EDGE_CURVE('',#12206,#12203,#220,.T.);
#15375=EDGE_CURVE('',#12203,#12185,#221,.T.);
#15376=EDGE_CURVE('',#12206,#12202,#222,.T.);
#15377=EDGE_CURVE('',#12195,#12206,#223,.T.);
#15378=EDGE_CURVE('',#12196,#12205,#224,.T.);
#15379=EDGE_CURVE('',#12207,#12208,#10220,.T.);
#15380=EDGE_CURVE('',#12209,#12208,#225,.T.);
#15381=EDGE_CURVE('',#12210,#12209,#226,.T.);
#15382=EDGE_CURVE('',#12210,#12207,#227,.T.);
#15383=EDGE_CURVE('',#12211,#12210,#228,.T.);
#15384=EDGE_CURVE('',#12211,#12212,#10221,.T.);
#15385=EDGE_CURVE('',#12212,#12207,#229,.T.);
#15386=EDGE_CURVE('',#12213,#12214,#10222,.T.);
#15387=EDGE_CURVE('',#12214,#12215,#10223,.T.);
#15388=EDGE_CURVE('',#12215,#12211,#10224,.T.);
#15389=EDGE_CURVE('',#12213,#12211,#10225,.T.);
#15390=EDGE_CURVE('',#12212,#12215,#10226,.T.);
#15391=EDGE_CURVE('',#12216,#12215,#230,.T.);
#15392=EDGE_CURVE('',#12216,#12217,#10227,.T.);
#15393=EDGE_CURVE('',#12217,#12212,#231,.T.);
#15394=EDGE_CURVE('',#12217,#12218,#232,.T.);
#15395=EDGE_CURVE('',#12207,#12218,#233,.T.);
#15396=EDGE_CURVE('',#12218,#12219,#234,.T.);
#15397=EDGE_CURVE('',#12208,#12219,#235,.T.);
#15398=EDGE_CURVE('',#12220,#12221,#236,.T.);
#15399=EDGE_CURVE('',#12219,#12221,#237,.T.);
#15400=EDGE_CURVE('',#12218,#12220,#238,.T.);
#15401=EDGE_CURVE('',#12217,#12222,#10228,.T.);
#15402=EDGE_CURVE('',#12222,#12220,#239,.T.);
#15403=EDGE_CURVE('',#12222,#12216,#10229,.T.);
#15404=EDGE_CURVE('',#12223,#12224,#10230,.T.);
#15405=EDGE_CURVE('',#12225,#12224,#240,.T.);
#15406=EDGE_CURVE('',#12226,#12225,#241,.T.);
#15407=EDGE_CURVE('',#12226,#12223,#242,.T.);
#15408=EDGE_CURVE('',#12226,#12227,#243,.T.);
#15409=EDGE_CURVE('',#12227,#12228,#10231,.T.);
#15410=EDGE_CURVE('',#12223,#12228,#244,.T.);
#15411=EDGE_CURVE('',#12228,#12229,#10232,.T.);
#15412=EDGE_CURVE('',#12229,#12227,#10233,.T.);
#15413=EDGE_CURVE('',#12229,#12216,#10234,.T.);
#15414=EDGE_CURVE('',#12227,#12222,#10235,.T.);
#15415=EDGE_CURVE('',#12229,#12214,#245,.T.);
#15416=EDGE_CURVE('',#12214,#12230,#10236,.T.);
#15417=EDGE_CURVE('',#12228,#12230,#246,.T.);
#15418=EDGE_CURVE('',#12230,#12213,#10237,.T.);
#15419=EDGE_CURVE('',#12231,#12232,#247,.T.);
#15420=EDGE_CURVE('',#12233,#12232,#248,.T.);
#15421=EDGE_CURVE('',#12234,#12233,#10238,.T.);
#15422=EDGE_CURVE('',#12234,#12231,#249,.T.);
#15423=EDGE_CURVE('',#12231,#12213,#250,.T.);
#15424=EDGE_CURVE('',#12234,#12230,#251,.T.);
#15425=EDGE_CURVE('',#12223,#12234,#252,.T.);
#15426=EDGE_CURVE('',#12224,#12233,#253,.T.);
#15427=EDGE_CURVE('',#12235,#12236,#254,.T.);
#15428=EDGE_CURVE('',#12237,#12236,#255,.T.);
#15429=EDGE_CURVE('',#12238,#12237,#256,.T.);
#15430=EDGE_CURVE('',#12238,#12235,#257,.T.);
#15431=EDGE_CURVE('',#12239,#12238,#258,.T.);
#15432=EDGE_CURVE('',#12239,#12240,#10239,.T.);
#15433=EDGE_CURVE('',#12240,#12235,#259,.T.);
#15434=EDGE_CURVE('',#12241,#12242,#10240,.T.);
#15435=EDGE_CURVE('',#12242,#12243,#10241,.T.);
#15436=EDGE_CURVE('',#12243,#12239,#10242,.T.);
#15437=EDGE_CURVE('',#12241,#12239,#10243,.T.);
#15438=EDGE_CURVE('',#12240,#12243,#10244,.T.);
#15439=EDGE_CURVE('',#12244,#12243,#260,.T.);
#15440=EDGE_CURVE('',#12244,#12245,#10245,.T.);
#15441=EDGE_CURVE('',#12245,#12240,#261,.T.);
#15442=EDGE_CURVE('',#12245,#12246,#262,.T.);
#15443=EDGE_CURVE('',#12235,#12246,#263,.T.);
#15444=EDGE_CURVE('',#12246,#12247,#10246,.T.);
#15445=EDGE_CURVE('',#12236,#12247,#264,.T.);
#15446=EDGE_CURVE('',#12248,#12249,#265,.T.);
#15447=EDGE_CURVE('',#12247,#12249,#266,.T.);
#15448=EDGE_CURVE('',#12246,#12248,#267,.T.);
#15449=EDGE_CURVE('',#12245,#12250,#10247,.T.);
#15450=EDGE_CURVE('',#12250,#12248,#268,.T.);
#15451=EDGE_CURVE('',#12250,#12244,#10248,.T.);
#15452=EDGE_CURVE('',#12251,#12252,#269,.T.);
#15453=EDGE_CURVE('',#12253,#12252,#270,.T.);
#15454=EDGE_CURVE('',#12254,#12253,#271,.T.);
#15455=EDGE_CURVE('',#12254,#12251,#272,.T.);
#15456=EDGE_CURVE('',#12254,#12255,#273,.T.);
#15457=EDGE_CURVE('',#12255,#12256,#10249,.T.);
#15458=EDGE_CURVE('',#12251,#12256,#274,.T.);
#15459=EDGE_CURVE('',#12256,#12257,#10250,.T.);
#15460=EDGE_CURVE('',#12257,#12255,#10251,.T.);
#15461=EDGE_CURVE('',#12257,#12244,#10252,.T.);
#15462=EDGE_CURVE('',#12255,#12250,#10253,.T.);
#15463=EDGE_CURVE('',#12257,#12242,#275,.T.);
#15464=EDGE_CURVE('',#12242,#12258,#10254,.T.);
#15465=EDGE_CURVE('',#12256,#12258,#276,.T.);
#15466=EDGE_CURVE('',#12258,#12241,#10255,.T.);
#15467=EDGE_CURVE('',#12259,#12260,#277,.T.);
#15468=EDGE_CURVE('',#12261,#12260,#278,.T.);
#15469=EDGE_CURVE('',#12262,#12261,#279,.T.);
#15470=EDGE_CURVE('',#12262,#12259,#280,.T.);
#15471=EDGE_CURVE('',#12259,#12241,#281,.T.);
#15472=EDGE_CURVE('',#12262,#12258,#282,.T.);
#15473=EDGE_CURVE('',#12251,#12262,#283,.T.);
#15474=EDGE_CURVE('',#12252,#12261,#284,.T.);
#15475=EDGE_CURVE('',#12263,#12264,#285,.T.);
#15476=EDGE_CURVE('',#12265,#12264,#286,.T.);
#15477=EDGE_CURVE('',#12266,#12265,#287,.T.);
#15478=EDGE_CURVE('',#12266,#12263,#288,.T.);
#15479=EDGE_CURVE('',#12267,#12266,#289,.T.);
#15480=EDGE_CURVE('',#12267,#12268,#10256,.T.);
#15481=EDGE_CURVE('',#12268,#12263,#290,.T.);
#15482=EDGE_CURVE('',#12269,#12270,#10257,.T.);
#15483=EDGE_CURVE('',#12270,#12271,#10258,.T.);
#15484=EDGE_CURVE('',#12271,#12267,#10259,.T.);
#15485=EDGE_CURVE('',#12269,#12267,#10260,.T.);
#15486=EDGE_CURVE('',#12268,#12271,#10261,.T.);
#15487=EDGE_CURVE('',#12272,#12271,#291,.T.);
#15488=EDGE_CURVE('',#12272,#12273,#10262,.T.);
#15489=EDGE_CURVE('',#12273,#12268,#292,.T.);
#15490=EDGE_CURVE('',#12273,#12274,#293,.T.);
#15491=EDGE_CURVE('',#12263,#12274,#294,.T.);
#15492=EDGE_CURVE('',#12274,#12275,#295,.T.);
#15493=EDGE_CURVE('',#12264,#12275,#296,.T.);
#15494=EDGE_CURVE('',#12276,#12277,#297,.T.);
#15495=EDGE_CURVE('',#12275,#12277,#298,.T.);
#15496=EDGE_CURVE('',#12274,#12276,#299,.T.);
#15497=EDGE_CURVE('',#12273,#12278,#10263,.T.);
#15498=EDGE_CURVE('',#12278,#12276,#300,.T.);
#15499=EDGE_CURVE('',#12278,#12272,#10264,.T.);
#15500=EDGE_CURVE('',#12279,#12280,#10265,.T.);
#15501=EDGE_CURVE('',#12281,#12280,#301,.T.);
#15502=EDGE_CURVE('',#12282,#12281,#302,.T.);
#15503=EDGE_CURVE('',#12282,#12279,#303,.T.);
#15504=EDGE_CURVE('',#12282,#12283,#304,.T.);
#15505=EDGE_CURVE('',#12283,#12284,#10266,.T.);
#15506=EDGE_CURVE('',#12279,#12284,#305,.T.);
#15507=EDGE_CURVE('',#12284,#12285,#10267,.T.);
#15508=EDGE_CURVE('',#12285,#12283,#10268,.T.);
#15509=EDGE_CURVE('',#12285,#12272,#10269,.T.);
#15510=EDGE_CURVE('',#12283,#12278,#10270,.T.);
#15511=EDGE_CURVE('',#12285,#12270,#306,.T.);
#15512=EDGE_CURVE('',#12270,#12286,#10271,.T.);
#15513=EDGE_CURVE('',#12284,#12286,#307,.T.);
#15514=EDGE_CURVE('',#12286,#12269,#10272,.T.);
#15515=EDGE_CURVE('',#12287,#12288,#308,.T.);
#15516=EDGE_CURVE('',#12289,#12288,#309,.T.);
#15517=EDGE_CURVE('',#12290,#12289,#10273,.T.);
#15518=EDGE_CURVE('',#12290,#12287,#310,.T.);
#15519=EDGE_CURVE('',#12287,#12269,#311,.T.);
#15520=EDGE_CURVE('',#12290,#12286,#312,.T.);
#15521=EDGE_CURVE('',#12279,#12290,#313,.T.);
#15522=EDGE_CURVE('',#12280,#12289,#314,.T.);
#15523=EDGE_CURVE('',#12291,#12292,#315,.T.);
#15524=EDGE_CURVE('',#12291,#12293,#10274,.T.);
#15525=EDGE_CURVE('',#12293,#12294,#316,.T.);
#15526=EDGE_CURVE('',#12292,#12294,#317,.T.);
#15527=EDGE_CURVE('',#12294,#12295,#318,.T.);
#15528=EDGE_CURVE('',#12296,#12295,#319,.T.);
#15529=EDGE_CURVE('',#12292,#12296,#320,.T.);
#15530=EDGE_CURVE('',#12297,#12298,#321,.T.);
#15531=EDGE_CURVE('',#12295,#12298,#322,.T.);
#15532=EDGE_CURVE('',#12294,#12297,#323,.T.);
#15533=EDGE_CURVE('',#12299,#12293,#324,.T.);
#15534=EDGE_CURVE('',#12299,#12297,#325,.T.);
#15535=EDGE_CURVE('',#12293,#12300,#10275,.T.);
#15536=EDGE_CURVE('',#12301,#12300,#326,.T.);
#15537=EDGE_CURVE('',#12301,#12299,#10276,.T.);
#15538=EDGE_CURVE('',#12300,#12291,#10277,.T.);
#15539=EDGE_CURVE('',#12302,#12303,#10278,.T.);
#15540=EDGE_CURVE('',#12303,#12300,#10279,.T.);
#15541=EDGE_CURVE('',#12302,#12291,#10280,.T.);
#15542=EDGE_CURVE('',#12304,#12303,#327,.T.);
#15543=EDGE_CURVE('',#12304,#12301,#10281,.T.);
#15544=EDGE_CURVE('',#12303,#12305,#10282,.T.);
#15545=EDGE_CURVE('',#12306,#12305,#328,.T.);
#15546=EDGE_CURVE('',#12306,#12304,#10283,.T.);
#15547=EDGE_CURVE('',#12305,#12302,#10284,.T.);
#15548=EDGE_CURVE('',#12307,#12308,#329,.T.);
#15549=EDGE_CURVE('',#12309,#12308,#330,.T.);
#15550=EDGE_CURVE('',#12310,#12309,#10285,.T.);
#15551=EDGE_CURVE('',#12310,#12307,#331,.T.);
#15552=EDGE_CURVE('',#12307,#12302,#332,.T.);
#15553=EDGE_CURVE('',#12310,#12305,#333,.T.);
#15554=EDGE_CURVE('',#12311,#12306,#334,.T.);
#15555=EDGE_CURVE('',#12311,#12310,#335,.T.);
#15556=EDGE_CURVE('',#12312,#12309,#336,.T.);
#15557=EDGE_CURVE('',#12311,#12312,#10286,.T.);
#15558=EDGE_CURVE('',#12313,#12312,#337,.T.);
#15559=EDGE_CURVE('',#12314,#12313,#338,.T.);
#15560=EDGE_CURVE('',#12314,#12311,#339,.T.);
#15561=EDGE_CURVE('',#12314,#12315,#340,.T.);
#15562=EDGE_CURVE('',#12315,#12306,#10287,.T.);
#15563=EDGE_CURVE('',#12304,#12315,#10288,.T.);
#15564=EDGE_CURVE('',#12316,#12301,#10289,.T.);
#15565=EDGE_CURVE('',#12315,#12316,#10290,.T.);
#15566=EDGE_CURVE('',#12299,#12316,#10291,.T.);
#15567=EDGE_CURVE('',#12316,#12317,#341,.T.);
#15568=EDGE_CURVE('',#12297,#12317,#342,.T.);
#15569=EDGE_CURVE('',#12317,#12318,#343,.T.);
#15570=EDGE_CURVE('',#12298,#12318,#344,.T.);
#15571=EDGE_CURVE('',#12319,#12320,#10292,.T.);
#15572=EDGE_CURVE('',#12321,#12320,#345,.T.);
#15573=EDGE_CURVE('',#12322,#12321,#346,.T.);
#15574=EDGE_CURVE('',#12322,#12319,#347,.T.);
#15575=EDGE_CURVE('',#12323,#12322,#348,.T.);
#15576=EDGE_CURVE('',#12323,#12324,#10293,.T.);
#15577=EDGE_CURVE('',#12324,#12319,#349,.T.);
#15578=EDGE_CURVE('',#12325,#12326,#10294,.T.);
#15579=EDGE_CURVE('',#12326,#12327,#10295,.T.);
#15580=EDGE_CURVE('',#12327,#12323,#10296,.T.);
#15581=EDGE_CURVE('',#12325,#12323,#10297,.T.);
#15582=EDGE_CURVE('',#12324,#12327,#10298,.T.);
#15583=EDGE_CURVE('',#12328,#12327,#350,.T.);
#15584=EDGE_CURVE('',#12328,#12329,#10299,.T.);
#15585=EDGE_CURVE('',#12329,#12324,#351,.T.);
#15586=EDGE_CURVE('',#12329,#12330,#352,.T.);
#15587=EDGE_CURVE('',#12319,#12330,#353,.T.);
#15588=EDGE_CURVE('',#12330,#12331,#10300,.T.);
#15589=EDGE_CURVE('',#12320,#12331,#354,.T.);
#15590=EDGE_CURVE('',#12332,#12333,#355,.T.);
#15591=EDGE_CURVE('',#12331,#12333,#356,.T.);
#15592=EDGE_CURVE('',#12330,#12332,#357,.T.);
#15593=EDGE_CURVE('',#12329,#12334,#10301,.T.);
#15594=EDGE_CURVE('',#12334,#12332,#358,.T.);
#15595=EDGE_CURVE('',#12334,#12328,#10302,.T.);
#15596=EDGE_CURVE('',#12335,#12336,#359,.T.);
#15597=EDGE_CURVE('',#12337,#12336,#360,.T.);
#15598=EDGE_CURVE('',#12338,#12337,#361,.T.);
#15599=EDGE_CURVE('',#12338,#12335,#362,.T.);
#15600=EDGE_CURVE('',#12338,#12339,#363,.T.);
#15601=EDGE_CURVE('',#12339,#12340,#10303,.T.);
#15602=EDGE_CURVE('',#12335,#12340,#364,.T.);
#15603=EDGE_CURVE('',#12340,#12341,#10304,.T.);
#15604=EDGE_CURVE('',#12341,#12339,#10305,.T.);
#15605=EDGE_CURVE('',#12341,#12328,#10306,.T.);
#15606=EDGE_CURVE('',#12339,#12334,#10307,.T.);
#15607=EDGE_CURVE('',#12341,#12326,#365,.T.);
#15608=EDGE_CURVE('',#12326,#12342,#10308,.T.);
#15609=EDGE_CURVE('',#12340,#12342,#366,.T.);
#15610=EDGE_CURVE('',#12342,#12325,#10309,.T.);
#15611=EDGE_CURVE('',#12343,#12344,#367,.T.);
#15612=EDGE_CURVE('',#12345,#12344,#368,.T.);
#15613=EDGE_CURVE('',#12346,#12345,#10310,.T.);
#15614=EDGE_CURVE('',#12346,#12343,#369,.T.);
#15615=EDGE_CURVE('',#12343,#12325,#370,.T.);
#15616=EDGE_CURVE('',#12346,#12342,#371,.T.);
#15617=EDGE_CURVE('',#12335,#12346,#372,.T.);
#15618=EDGE_CURVE('',#12336,#12345,#373,.T.);
#15619=EDGE_CURVE('',#12125,#12308,#10311,.T.);
#15620=EDGE_CURVE('',#12313,#12137,#10312,.T.);
#15621=EDGE_CURVE('',#12153,#12148,#10313,.T.);
#15622=EDGE_CURVE('',#12141,#12165,#10314,.T.);
#15623=EDGE_CURVE('',#12181,#12176,#10315,.T.);
#15624=EDGE_CURVE('',#12169,#12193,#10316,.T.);
#15625=EDGE_CURVE('',#12209,#12204,#10317,.T.);
#15626=EDGE_CURVE('',#12197,#12221,#10318,.T.);
#15627=EDGE_CURVE('',#12237,#12232,#10319,.T.);
#15628=EDGE_CURVE('',#12225,#12249,#10320,.T.);
#15629=EDGE_CURVE('',#12265,#12260,#10321,.T.);
#15630=EDGE_CURVE('',#12253,#12277,#10322,.T.);
#15631=EDGE_CURVE('',#12321,#12288,#10323,.T.);
#15632=EDGE_CURVE('',#12281,#12333,#10324,.T.);
#15633=EDGE_CURVE('',#12296,#12344,#10325,.T.);
#15634=EDGE_CURVE('',#12337,#12318,#10326,.T.);
#15635=EDGE_CURVE('',#12347,#12347,#10327,.T.);
#15636=EDGE_CURVE('',#12348,#12348,#10328,.T.);
#15637=EDGE_CURVE('',#12348,#12347,#6894,.T.);
#15638=EDGE_CURVE('',#12349,#12349,#10329,.T.);
#15639=EDGE_CURVE('',#12350,#12350,#10330,.T.);
#15640=EDGE_CURVE('',#12350,#12349,#6895,.T.);
#15641=EDGE_CURVE('',#12351,#12351,#10331,.T.);
#15642=EDGE_CURVE('',#12352,#12352,#10332,.T.);
#15643=EDGE_CURVE('',#12352,#12351,#6896,.T.);
#15644=EDGE_CURVE('',#12353,#12353,#10333,.T.);
#15645=EDGE_CURVE('',#12354,#12354,#10334,.T.);
#15646=EDGE_CURVE('',#12354,#12353,#6897,.T.);
#15647=EDGE_CURVE('',#12355,#12355,#10335,.T.);
#15648=EDGE_CURVE('',#12355,#12356,#6898,.T.);
#15649=EDGE_CURVE('',#12356,#12356,#10336,.T.);
#15650=EDGE_CURVE('',#12357,#12357,#10337,.T.);
#15651=EDGE_CURVE('',#12357,#12358,#6899,.T.);
#15652=EDGE_CURVE('',#12358,#12358,#10338,.T.);
#15653=EDGE_CURVE('',#12359,#12359,#10339,.T.);
#15654=EDGE_CURVE('',#12359,#12360,#6900,.T.);
#15655=EDGE_CURVE('',#12360,#12360,#10340,.T.);
#15656=EDGE_CURVE('',#12361,#12361,#10341,.T.);
#15657=EDGE_CURVE('',#12362,#12363,#6901,.T.);
#15658=EDGE_CURVE('',#12363,#12364,#6902,.T.);
#15659=EDGE_CURVE('',#12364,#12365,#6903,.T.);
#15660=EDGE_CURVE('',#12365,#12366,#6904,.T.);
#15661=EDGE_CURVE('',#12366,#12367,#6905,.T.);
#15662=EDGE_CURVE('',#12367,#12362,#6906,.T.);
#15663=EDGE_CURVE('',#12368,#12368,#10342,.T.);
#15664=EDGE_CURVE('',#12361,#12368,#6907,.T.);
#15665=EDGE_CURVE('',#12369,#12370,#6908,.T.);
#15666=EDGE_CURVE('',#12371,#12369,#6909,.T.);
#15667=EDGE_CURVE('',#12372,#12371,#6910,.T.);
#15668=EDGE_CURVE('',#12373,#12372,#6911,.T.);
#15669=EDGE_CURVE('',#12374,#12373,#6912,.T.);
#15670=EDGE_CURVE('',#12370,#12374,#6913,.T.);
#15671=EDGE_CURVE('',#12369,#12367,#6914,.T.);
#15672=EDGE_CURVE('',#12370,#12362,#6915,.T.);
#15673=EDGE_CURVE('',#12371,#12366,#6916,.T.);
#15674=EDGE_CURVE('',#12372,#12365,#6917,.T.);
#15675=EDGE_CURVE('',#12373,#12364,#6918,.T.);
#15676=EDGE_CURVE('',#12374,#12363,#6919,.T.);
#15677=EDGE_CURVE('',#12375,#12375,#10343,.T.);
#15678=EDGE_CURVE('',#12376,#12376,#10344,.T.);
#15679=EDGE_CURVE('',#12375,#12377,#6920,.T.);
#15680=EDGE_CURVE('',#12377,#12377,#10345,.T.);
#15681=EDGE_CURVE('',#12377,#12378,#10346,.T.);
#15682=EDGE_CURVE('',#12378,#12378,#10347,.T.);
#15683=EDGE_CURVE('',#12379,#12380,#6921,.T.);
#15684=EDGE_CURVE('',#12380,#12381,#6922,.T.);
#15685=EDGE_CURVE('',#12381,#12382,#6923,.T.);
#15686=EDGE_CURVE('',#12382,#12383,#6924,.T.);
#15687=EDGE_CURVE('',#12383,#12384,#6925,.T.);
#15688=EDGE_CURVE('',#12384,#12379,#6926,.T.);
#15689=EDGE_CURVE('',#12385,#12386,#6927,.T.);
#15690=EDGE_CURVE('',#12386,#12387,#6928,.T.);
#15691=EDGE_CURVE('',#12387,#12388,#6929,.T.);
#15692=EDGE_CURVE('',#12388,#12389,#6930,.T.);
#15693=EDGE_CURVE('',#12389,#12390,#6931,.T.);
#15694=EDGE_CURVE('',#12390,#12385,#6932,.T.);
#15695=EDGE_CURVE('',#12381,#12390,#6933,.T.);
#15696=EDGE_CURVE('',#12380,#12385,#6934,.T.);
#15697=EDGE_CURVE('',#12382,#12389,#6935,.T.);
#15698=EDGE_CURVE('',#12383,#12388,#6936,.T.);
#15699=EDGE_CURVE('',#12384,#12387,#6937,.T.);
#15700=EDGE_CURVE('',#12379,#12386,#6938,.T.);
#15701=EDGE_CURVE('',#12391,#12391,#10348,.T.);
#15702=EDGE_CURVE('',#12392,#12392,#10349,.T.);
#15703=EDGE_CURVE('',#12392,#12391,#6939,.T.);
#15704=EDGE_CURVE('',#12392,#12376,#6940,.T.);
#15705=EDGE_CURVE('',#12393,#12393,#10350,.T.);
#15706=EDGE_CURVE('',#12394,#12394,#10351,.T.);
#15707=EDGE_CURVE('',#12393,#12395,#6941,.T.);
#15708=EDGE_CURVE('',#12395,#12395,#10352,.T.);
#15709=EDGE_CURVE('',#12395,#12396,#10353,.T.);
#15710=EDGE_CURVE('',#12396,#12396,#10354,.T.);
#15711=EDGE_CURVE('',#12397,#12398,#6942,.T.);
#15712=EDGE_CURVE('',#12398,#12399,#6943,.T.);
#15713=EDGE_CURVE('',#12399,#12400,#6944,.T.);
#15714=EDGE_CURVE('',#12400,#12401,#6945,.T.);
#15715=EDGE_CURVE('',#12401,#12402,#6946,.T.);
#15716=EDGE_CURVE('',#12402,#12397,#6947,.T.);
#15717=EDGE_CURVE('',#12403,#12404,#6948,.T.);
#15718=EDGE_CURVE('',#12404,#12405,#6949,.T.);
#15719=EDGE_CURVE('',#12405,#12406,#6950,.T.);
#15720=EDGE_CURVE('',#12406,#12407,#6951,.T.);
#15721=EDGE_CURVE('',#12407,#12408,#6952,.T.);
#15722=EDGE_CURVE('',#12408,#12403,#6953,.T.);
#15723=EDGE_CURVE('',#12399,#12408,#6954,.T.);
#15724=EDGE_CURVE('',#12398,#12403,#6955,.T.);
#15725=EDGE_CURVE('',#12400,#12407,#6956,.T.);
#15726=EDGE_CURVE('',#12401,#12406,#6957,.T.);
#15727=EDGE_CURVE('',#12402,#12405,#6958,.T.);
#15728=EDGE_CURVE('',#12397,#12404,#6959,.T.);
#15729=EDGE_CURVE('',#12409,#12409,#10355,.T.);
#15730=EDGE_CURVE('',#12410,#12410,#10356,.T.);
#15731=EDGE_CURVE('',#12410,#12409,#6960,.T.);
#15732=EDGE_CURVE('',#12410,#12394,#6961,.T.);
#15733=EDGE_CURVE('',#12411,#12412,#6962,.T.);
#15734=EDGE_CURVE('',#12412,#12413,#10357,.T.);
#15735=EDGE_CURVE('',#12413,#12414,#6963,.T.);
#15736=EDGE_CURVE('',#12414,#12411,#10358,.T.);
#15737=EDGE_CURVE('',#12415,#12416,#10359,.T.);
#15738=EDGE_CURVE('',#12416,#12413,#6964,.T.);
#15739=EDGE_CURVE('',#12412,#12415,#6965,.T.);
#15740=EDGE_CURVE('',#12417,#12418,#10360,.T.);
#15741=EDGE_CURVE('',#12419,#12418,#10361,.T.);
#15742=EDGE_CURVE('',#12419,#12420,#10362,.T.);
#15743=EDGE_CURVE('',#12420,#12417,#10363,.T.);
#15744=EDGE_CURVE('',#12421,#12422,#10364,.T.);
#15745=EDGE_CURVE('',#12423,#12422,#10365,.T.);
#15746=EDGE_CURVE('',#12423,#12424,#10366,.T.);
#15747=EDGE_CURVE('',#12424,#12421,#10367,.T.);
#15748=EDGE_CURVE('',#12425,#12426,#10368,.T.);
#15749=EDGE_CURVE('',#12426,#12421,#6966,.T.);
#15750=EDGE_CURVE('',#12424,#12425,#6967,.T.);
#15751=EDGE_CURVE('',#12427,#12417,#6968,.T.);
#15752=EDGE_CURVE('',#12420,#12428,#6969,.T.);
#15753=EDGE_CURVE('',#12428,#12427,#10369,.T.);
#15754=EDGE_CURVE('',#12429,#12423,#6970,.T.);
#15755=EDGE_CURVE('',#12429,#12425,#10370,.T.);
#15756=EDGE_CURVE('',#12430,#12419,#6971,.T.);
#15757=EDGE_CURVE('',#12430,#12428,#10371,.T.);
#15758=EDGE_CURVE('',#12426,#12431,#10372,.T.);
#15759=EDGE_CURVE('',#12422,#12431,#6972,.T.);
#15760=EDGE_CURVE('',#12427,#12432,#10373,.T.);
#15761=EDGE_CURVE('',#12418,#12432,#6973,.T.);
#15762=EDGE_CURVE('',#12431,#12430,#10374,.T.);
#15763=EDGE_CURVE('',#12432,#12433,#10375,.T.);
#15764=EDGE_CURVE('',#12433,#12416,#6974,.T.);
#15765=EDGE_CURVE('',#12415,#12434,#6975,.T.);
#15766=EDGE_CURVE('',#12434,#12429,#10376,.T.);
#15767=EDGE_CURVE('',#12435,#12436,#374,.T.);
#15768=EDGE_CURVE('',#12436,#12435,#375,.T.);
#15769=EDGE_CURVE('',#12437,#12438,#6976,.T.);
#15770=EDGE_CURVE('',#12438,#12437,#376,.T.);
#15771=EDGE_CURVE('',#12414,#12439,#6977,.T.);
#15772=EDGE_CURVE('',#12440,#12439,#10377,.T.);
#15773=EDGE_CURVE('',#12440,#12411,#6978,.T.);
#15774=EDGE_CURVE('',#12434,#12440,#6979,.T.);
#15775=EDGE_CURVE('',#12439,#12433,#6980,.T.);
#15776=EDGE_CURVE('',#12436,#12441,#6981,.T.);
#15777=EDGE_CURVE('',#12441,#12441,#10378,.T.);
#15778=EDGE_CURVE('',#12437,#12438,#10379,.T.);
#15779=EDGE_CURVE('',#12442,#12442,#10380,.T.);
#15780=EDGE_CURVE('',#12443,#12443,#10381,.T.);
#15781=EDGE_CURVE('',#12443,#12442,#6982,.T.);
#15782=EDGE_CURVE('',#12444,#12444,#10382,.T.);
#15783=EDGE_CURVE('',#12445,#12445,#10383,.T.);
#15784=EDGE_CURVE('',#12445,#12444,#6983,.T.);
#15785=EDGE_CURVE('',#12446,#12447,#10384,.T.);
#15786=EDGE_CURVE('',#12447,#12446,#377,.F.);
#15787=EDGE_CURVE('',#12448,#12449,#6984,.T.);
#15788=EDGE_CURVE('',#12450,#12448,#6985,.T.);
#15789=EDGE_CURVE('',#12451,#12450,#6986,.T.);
#15790=EDGE_CURVE('',#12452,#12451,#6987,.T.);
#15791=EDGE_CURVE('',#12449,#12452,#6988,.T.);
#15792=EDGE_CURVE('',#12453,#12453,#10385,.T.);
#15793=EDGE_CURVE('',#12454,#12455,#378,.F.);
#15794=EDGE_CURVE('',#12455,#12454,#379,.F.);
#15795=EDGE_CURVE('',#12455,#12453,#6989,.T.);
#15796=EDGE_CURVE('',#12456,#12456,#10386,.T.);
#15797=EDGE_CURVE('',#12456,#12457,#6990,.T.);
#15798=EDGE_CURVE('',#12457,#12457,#10387,.T.);
#15799=EDGE_CURVE('',#12458,#12458,#10388,.T.);
#15800=EDGE_CURVE('',#12458,#12459,#6991,.T.);
#15801=EDGE_CURVE('',#12459,#12459,#10389,.T.);
#15802=EDGE_CURVE('',#12446,#12447,#6992,.T.);
#15803=EDGE_CURVE('',#12460,#12461,#6993,.T.);
#15804=EDGE_CURVE('',#12462,#12460,#6994,.T.);
#15805=EDGE_CURVE('',#12463,#12462,#6995,.T.);
#15806=EDGE_CURVE('',#12464,#12463,#6996,.T.);
#15807=EDGE_CURVE('',#12461,#12464,#6997,.T.);
#15808=EDGE_CURVE('',#12464,#12465,#10390,.T.);
#15809=EDGE_CURVE('',#12465,#12466,#6998,.T.);
#15810=EDGE_CURVE('',#12466,#12467,#6999,.T.);
#15811=EDGE_CURVE('',#12467,#12468,#7000,.T.);
#15812=EDGE_CURVE('',#12468,#12450,#10391,.T.);
#15813=EDGE_CURVE('',#12448,#12461,#10392,.T.);
#15814=EDGE_CURVE('',#12449,#12460,#10393,.T.);
#15815=EDGE_CURVE('',#12469,#12462,#10394,.T.);
#15816=EDGE_CURVE('',#12470,#12469,#10395,.T.);
#15817=EDGE_CURVE('',#12471,#12470,#10396,.T.);
#15818=EDGE_CURVE('',#12472,#12471,#10397,.T.);
#15819=EDGE_CURVE('',#12473,#12472,#10398,.T.);
#15820=EDGE_CURVE('',#12474,#12473,#10399,.T.);
#15821=EDGE_CURVE('',#12475,#12474,#10400,.T.);
#15822=EDGE_CURVE('',#12476,#12475,#10401,.T.);
#15823=EDGE_CURVE('',#12452,#12476,#10402,.T.);
#15824=EDGE_CURVE('',#12451,#12477,#10403,.T.);
#15825=EDGE_CURVE('',#12477,#12478,#7001,.T.);
#15826=EDGE_CURVE('',#12478,#12479,#7002,.T.);
#15827=EDGE_CURVE('',#12479,#12480,#7003,.T.);
#15828=EDGE_CURVE('',#12480,#12463,#10404,.T.);
#15829=EDGE_CURVE('',#12481,#12468,#7004,.T.);
#15830=EDGE_CURVE('',#12482,#12481,#380,.T.);
#15831=EDGE_CURVE('',#12477,#12482,#7005,.T.);
#15832=EDGE_CURVE('',#12483,#12480,#7006,.T.);
#15833=EDGE_CURVE('',#12484,#12483,#381,.T.);
#15834=EDGE_CURVE('',#12465,#12484,#7007,.T.);
#15835=EDGE_CURVE('',#12485,#12486,#7008,.T.);
#15836=EDGE_CURVE('',#12486,#12487,#382,.T.);
#15837=EDGE_CURVE('',#12487,#12488,#7009,.T.);
#15838=EDGE_CURVE('',#12488,#12485,#10405,.T.);
#15839=EDGE_CURVE('',#12489,#12490,#10406,.T.);
#15840=EDGE_CURVE('',#12490,#12491,#7010,.T.);
#15841=EDGE_CURVE('',#12492,#12491,#383,.T.);
#15842=EDGE_CURVE('',#12493,#12492,#384,.T.);
#15843=EDGE_CURVE('',#12491,#12493,#385,.T.);
#15844=EDGE_CURVE('',#12490,#12494,#10407,.T.);
#15845=EDGE_CURVE('',#12494,#12484,#7011,.T.);
#15846=EDGE_CURVE('',#12483,#12495,#7012,.T.);
#15847=EDGE_CURVE('',#12495,#12496,#10408,.T.);
#15848=EDGE_CURVE('',#12496,#12482,#7013,.T.);
#15849=EDGE_CURVE('',#12481,#12489,#7014,.T.);
#15850=EDGE_CURVE('',#12494,#12466,#7015,.T.);
#15851=EDGE_CURVE('',#12479,#12495,#7016,.T.);
#15852=EDGE_CURVE('',#12467,#12489,#7017,.T.);
#15853=EDGE_CURVE('',#12496,#12478,#7018,.T.);
#15854=EDGE_CURVE('',#12497,#12498,#10409,.T.);
#15855=EDGE_CURVE('',#12476,#12497,#7019,.T.);
#15856=EDGE_CURVE('',#12498,#12475,#7020,.T.);
#15857=EDGE_CURVE('',#12499,#12500,#10410,.T.);
#15858=EDGE_CURVE('',#12472,#12499,#7021,.T.);
#15859=EDGE_CURVE('',#12500,#12471,#7022,.T.);
#15860=EDGE_CURVE('',#12501,#12469,#7023,.T.);
#15861=EDGE_CURVE('',#12502,#12501,#10411,.T.);
#15862=EDGE_CURVE('',#12470,#12502,#7024,.T.);
#15863=EDGE_CURVE('',#12498,#12503,#10412,.T.);
#15864=EDGE_CURVE('',#12474,#12503,#7025,.T.);
#15865=EDGE_CURVE('',#12500,#12502,#10413,.T.);
#15866=EDGE_CURVE('',#12504,#12473,#7026,.T.);
#15867=EDGE_CURVE('',#12503,#12504,#10414,.T.);
#15868=EDGE_CURVE('',#12499,#12501,#10415,.T.);
#15869=EDGE_CURVE('',#12497,#12504,#10416,.T.);
#15870=EDGE_CURVE('',#12505,#12506,#386,.F.);
#15871=EDGE_CURVE('',#12506,#12507,#10417,.T.);
#15872=EDGE_CURVE('',#12507,#12508,#7027,.T.);
#15873=EDGE_CURVE('',#12508,#12509,#10418,.T.);
#15874=EDGE_CURVE('',#12509,#12510,#7028,.T.);
#15875=EDGE_CURVE('',#12510,#12511,#10419,.T.);
#15876=EDGE_CURVE('',#12511,#12512,#7029,.T.);
#15877=EDGE_CURVE('',#12512,#12513,#10420,.T.);
#15878=EDGE_CURVE('',#12513,#12505,#7030,.T.);
#15879=EDGE_CURVE('',#12514,#12515,#10421,.T.);
#15880=EDGE_CURVE('',#12515,#12516,#7031,.T.);
#15881=EDGE_CURVE('',#12516,#12517,#10422,.T.);
#15882=EDGE_CURVE('',#12517,#12518,#7032,.T.);
#15883=EDGE_CURVE('',#12518,#12519,#10423,.T.);
#15884=EDGE_CURVE('',#12519,#12520,#7033,.T.);
#15885=EDGE_CURVE('',#12520,#12521,#10424,.T.);
#15886=EDGE_CURVE('',#12521,#12514,#7034,.T.);
#15887=EDGE_CURVE('',#12522,#12523,#7035,.T.);
#15888=EDGE_CURVE('',#12523,#12524,#658,.T.);
#15889=EDGE_CURVE('',#12524,#12525,#659,.T.);
#15890=EDGE_CURVE('',#12525,#12526,#7036,.T.);
#15891=EDGE_CURVE('',#12526,#12527,#660,.T.);
#15892=EDGE_CURVE('',#12527,#12522,#661,.T.);
#15893=EDGE_CURVE('',#12528,#12529,#662,.F.);
#15894=EDGE_CURVE('',#12529,#12530,#7037,.T.);
#15895=EDGE_CURVE('',#12530,#12531,#10425,.T.);
#15896=EDGE_CURVE('',#12531,#12532,#10426,.T.);
#15897=EDGE_CURVE('',#12532,#12533,#7038,.T.);
#15898=EDGE_CURVE('',#12533,#12534,#10427,.T.);
#15899=EDGE_CURVE('',#12534,#12535,#7039,.T.);
#15900=EDGE_CURVE('',#12535,#12536,#10428,.T.);
#15901=EDGE_CURVE('',#12536,#12537,#10429,.T.);
#15902=EDGE_CURVE('',#12537,#12538,#7040,.T.);
#15903=EDGE_CURVE('',#12538,#12528,#663,.T.);
#15904=EDGE_CURVE('',#12539,#12540,#664,.T.);
#15905=EDGE_CURVE('',#12540,#12541,#7041,.T.);
#15906=EDGE_CURVE('',#12541,#12542,#665,.T.);
#15907=EDGE_CURVE('',#12542,#12543,#666,.T.);
#15908=EDGE_CURVE('',#12543,#12544,#7042,.T.);
#15909=EDGE_CURVE('',#12544,#12539,#667,.T.);
#15910=EDGE_CURVE('',#12545,#12546,#10430,.T.);
#15911=EDGE_CURVE('',#12546,#12547,#7043,.T.);
#15912=EDGE_CURVE('',#12547,#12548,#10431,.T.);
#15913=EDGE_CURVE('',#12548,#12549,#7044,.T.);
#15914=EDGE_CURVE('',#12549,#12550,#10432,.T.);
#15915=EDGE_CURVE('',#12550,#12551,#7045,.T.);
#15916=EDGE_CURVE('',#12551,#12552,#10433,.T.);
#15917=EDGE_CURVE('',#12552,#12545,#7046,.T.);
#15918=EDGE_CURVE('',#12552,#12516,#7047,.T.);
#15919=EDGE_CURVE('',#12551,#12517,#7048,.T.);
#15920=EDGE_CURVE('',#12545,#12515,#7049,.T.);
#15921=EDGE_CURVE('',#12550,#12518,#7050,.T.);
#15922=EDGE_CURVE('',#12549,#12519,#7051,.T.);
#15923=EDGE_CURVE('',#12548,#12520,#7052,.T.);
#15924=EDGE_CURVE('',#12547,#12521,#7053,.T.);
#15925=EDGE_CURVE('',#12546,#12514,#7054,.T.);
#15926=EDGE_CURVE('',#12553,#12530,#7055,.T.);
#15927=EDGE_CURVE('',#12554,#12553,#668,.T.);
#15928=EDGE_CURVE('',#12554,#12531,#7056,.T.);
#15929=EDGE_CURVE('',#12555,#12529,#7057,.T.);
#15930=EDGE_CURVE('',#12553,#12555,#7058,.T.);
#15931=EDGE_CURVE('',#12556,#12528,#7059,.T.);
#15932=EDGE_CURVE('',#12555,#12556,#669,.F.);
#15933=EDGE_CURVE('',#12557,#12537,#7060,.T.);
#15934=EDGE_CURVE('',#12558,#12557,#7061,.T.);
#15935=EDGE_CURVE('',#12558,#12538,#7062,.T.);
#15936=EDGE_CURVE('',#12559,#12536,#7063,.T.);
#15937=EDGE_CURVE('',#12557,#12559,#10434,.T.);
#15938=EDGE_CURVE('',#12560,#12535,#7064,.T.);
#15939=EDGE_CURVE('',#12559,#12560,#10435,.T.);
#15940=EDGE_CURVE('',#12561,#12534,#7065,.T.);
#15941=EDGE_CURVE('',#12560,#12561,#7066,.T.);
#15942=EDGE_CURVE('',#12562,#12533,#7067,.T.);
#15943=EDGE_CURVE('',#12561,#12562,#10436,.T.);
#15944=EDGE_CURVE('',#12563,#12532,#7068,.T.);
#15945=EDGE_CURVE('',#12562,#12563,#7069,.T.);
#15946=EDGE_CURVE('',#12563,#12554,#10437,.T.);
#15947=EDGE_CURVE('',#12556,#12558,#670,.T.);
#15948=EDGE_CURVE('',#12564,#12565,#671,.T.);
#15949=EDGE_CURVE('',#12565,#12566,#7070,.T.);
#15950=EDGE_CURVE('',#12566,#12567,#672,.T.);
#15951=EDGE_CURVE('',#12567,#12568,#673,.T.);
#15952=EDGE_CURVE('',#12568,#12569,#7071,.T.);
#15953=EDGE_CURVE('',#12569,#12564,#674,.T.);
#15954=EDGE_CURVE('',#12567,#12524,#7072,.T.);
#15955=EDGE_CURVE('',#12566,#12525,#7073,.T.);
#15956=EDGE_CURVE('',#12568,#12523,#7074,.T.);
#15957=EDGE_CURVE('',#12565,#12526,#7075,.T.);
#15958=EDGE_CURVE('',#12564,#12527,#7076,.T.);
#15959=EDGE_CURVE('',#12569,#12522,#7077,.T.);
#15960=EDGE_CURVE('',#12570,#12543,#7078,.T.);
#15961=EDGE_CURVE('',#12571,#12570,#7079,.T.);
#15962=EDGE_CURVE('',#12571,#12544,#7080,.T.);
#15963=EDGE_CURVE('',#12572,#12542,#7081,.T.);
#15964=EDGE_CURVE('',#12570,#12572,#675,.T.);
#15965=EDGE_CURVE('',#12573,#12541,#7082,.T.);
#15966=EDGE_CURVE('',#12572,#12573,#676,.T.);
#15967=EDGE_CURVE('',#12574,#12540,#7083,.T.);
#15968=EDGE_CURVE('',#12573,#12574,#7084,.T.);
#15969=EDGE_CURVE('',#12575,#12571,#677,.T.);
#15970=EDGE_CURVE('',#12575,#12539,#7085,.T.);
#15971=EDGE_CURVE('',#12574,#12575,#678,.T.);
#15972=EDGE_CURVE('',#12576,#12508,#7086,.T.);
#15973=EDGE_CURVE('',#12577,#12576,#10438,.T.);
#15974=EDGE_CURVE('',#12577,#12509,#7087,.T.);
#15975=EDGE_CURVE('',#12578,#12507,#7088,.T.);
#15976=EDGE_CURVE('',#12576,#12578,#7089,.T.);
#15977=EDGE_CURVE('',#12579,#12506,#7090,.T.);
#15978=EDGE_CURVE('',#12578,#12579,#10439,.T.);
#15979=EDGE_CURVE('',#12580,#12505,#7091,.T.);
#15980=EDGE_CURVE('',#12579,#12580,#387,.F.);
#15981=EDGE_CURVE('',#12581,#12513,#7092,.T.);
#15982=EDGE_CURVE('',#12580,#12581,#7093,.T.);
#15983=EDGE_CURVE('',#12582,#12488,#7094,.T.);
#15984=EDGE_CURVE('',#12583,#12582,#10440,.T.);
#15985=EDGE_CURVE('',#12583,#12485,#7095,.T.);
#15986=EDGE_CURVE('',#12584,#12487,#7096,.T.);
#15987=EDGE_CURVE('',#12582,#12584,#7097,.T.);
#15988=EDGE_CURVE('',#12585,#12512,#7098,.T.);
#15989=EDGE_CURVE('',#12581,#12585,#10441,.T.);
#15990=EDGE_CURVE('',#12586,#12511,#7099,.T.);
#15991=EDGE_CURVE('',#12585,#12586,#7100,.T.);
#15992=EDGE_CURVE('',#12587,#12510,#7101,.T.);
#15993=EDGE_CURVE('',#12586,#12587,#10442,.T.);
#15994=EDGE_CURVE('',#12587,#12577,#7102,.T.);
#15995=EDGE_CURVE('',#12588,#12486,#7103,.T.);
#15996=EDGE_CURVE('',#12584,#12588,#388,.T.);
#15997=EDGE_CURVE('',#12588,#12583,#7104,.T.);
#15998=EDGE_CURVE('',#12589,#12589,#10443,.T.);
#15999=EDGE_CURVE('',#12590,#12591,#7105,.T.);
#16000=EDGE_CURVE('',#12591,#12592,#7106,.T.);
#16001=EDGE_CURVE('',#12592,#12593,#7107,.T.);
#16002=EDGE_CURVE('',#12593,#12594,#7108,.T.);
#16003=EDGE_CURVE('',#12594,#12595,#7109,.T.);
#16004=EDGE_CURVE('',#12595,#12590,#7110,.T.);
#16005=EDGE_CURVE('',#12596,#12596,#10444,.T.);
#16006=EDGE_CURVE('',#12589,#12596,#7111,.T.);
#16007=EDGE_CURVE('',#12597,#12598,#7112,.T.);
#16008=EDGE_CURVE('',#12599,#12597,#7113,.T.);
#16009=EDGE_CURVE('',#12600,#12599,#7114,.T.);
#16010=EDGE_CURVE('',#12601,#12600,#7115,.T.);
#16011=EDGE_CURVE('',#12602,#12601,#7116,.T.);
#16012=EDGE_CURVE('',#12598,#12602,#7117,.T.);
#16013=EDGE_CURVE('',#12597,#12595,#7118,.T.);
#16014=EDGE_CURVE('',#12598,#12590,#7119,.T.);
#16015=EDGE_CURVE('',#12599,#12594,#7120,.T.);
#16016=EDGE_CURVE('',#12600,#12593,#7121,.T.);
#16017=EDGE_CURVE('',#12601,#12592,#7122,.T.);
#16018=EDGE_CURVE('',#12602,#12591,#7123,.T.);
#16019=EDGE_CURVE('',#12603,#12603,#10445,.T.);
#16020=EDGE_CURVE('',#12604,#12604,#10446,.T.);
#16021=EDGE_CURVE('',#12603,#12605,#7124,.T.);
#16022=EDGE_CURVE('',#12605,#12605,#10447,.T.);
#16023=EDGE_CURVE('',#12605,#12606,#10448,.T.);
#16024=EDGE_CURVE('',#12606,#12606,#10449,.T.);
#16025=EDGE_CURVE('',#12607,#12608,#7125,.T.);
#16026=EDGE_CURVE('',#12608,#12609,#7126,.T.);
#16027=EDGE_CURVE('',#12609,#12610,#7127,.T.);
#16028=EDGE_CURVE('',#12610,#12611,#7128,.T.);
#16029=EDGE_CURVE('',#12611,#12612,#7129,.T.);
#16030=EDGE_CURVE('',#12612,#12607,#7130,.T.);
#16031=EDGE_CURVE('',#12613,#12614,#7131,.T.);
#16032=EDGE_CURVE('',#12614,#12615,#7132,.T.);
#16033=EDGE_CURVE('',#12615,#12616,#7133,.T.);
#16034=EDGE_CURVE('',#12616,#12617,#7134,.T.);
#16035=EDGE_CURVE('',#12617,#12618,#7135,.T.);
#16036=EDGE_CURVE('',#12618,#12613,#7136,.T.);
#16037=EDGE_CURVE('',#12609,#12618,#7137,.T.);
#16038=EDGE_CURVE('',#12608,#12613,#7138,.T.);
#16039=EDGE_CURVE('',#12610,#12617,#7139,.T.);
#16040=EDGE_CURVE('',#12611,#12616,#7140,.T.);
#16041=EDGE_CURVE('',#12612,#12615,#7141,.T.);
#16042=EDGE_CURVE('',#12607,#12614,#7142,.T.);
#16043=EDGE_CURVE('',#12619,#12619,#10450,.T.);
#16044=EDGE_CURVE('',#12620,#12620,#10451,.T.);
#16045=EDGE_CURVE('',#12620,#12619,#7143,.T.);
#16046=EDGE_CURVE('',#12620,#12604,#7144,.T.);
#16047=EDGE_CURVE('',#12621,#12621,#10452,.T.);
#16048=EDGE_CURVE('',#12622,#12622,#10453,.T.);
#16049=EDGE_CURVE('',#12621,#12623,#7145,.T.);
#16050=EDGE_CURVE('',#12623,#12623,#10454,.T.);
#16051=EDGE_CURVE('',#12623,#12624,#10455,.T.);
#16052=EDGE_CURVE('',#12624,#12624,#10456,.T.);
#16053=EDGE_CURVE('',#12625,#12626,#7146,.T.);
#16054=EDGE_CURVE('',#12626,#12627,#7147,.T.);
#16055=EDGE_CURVE('',#12627,#12628,#7148,.T.);
#16056=EDGE_CURVE('',#12628,#12629,#7149,.T.);
#16057=EDGE_CURVE('',#12629,#12630,#7150,.T.);
#16058=EDGE_CURVE('',#12630,#12625,#7151,.T.);
#16059=EDGE_CURVE('',#12631,#12632,#7152,.T.);
#16060=EDGE_CURVE('',#12632,#12633,#7153,.T.);
#16061=EDGE_CURVE('',#12633,#12634,#7154,.T.);
#16062=EDGE_CURVE('',#12634,#12635,#7155,.T.);
#16063=EDGE_CURVE('',#12635,#12636,#7156,.T.);
#16064=EDGE_CURVE('',#12636,#12631,#7157,.T.);
#16065=EDGE_CURVE('',#12627,#12636,#7158,.T.);
#16066=EDGE_CURVE('',#12626,#12631,#7159,.T.);
#16067=EDGE_CURVE('',#12628,#12635,#7160,.T.);
#16068=EDGE_CURVE('',#12629,#12634,#7161,.T.);
#16069=EDGE_CURVE('',#12630,#12633,#7162,.T.);
#16070=EDGE_CURVE('',#12625,#12632,#7163,.T.);
#16071=EDGE_CURVE('',#12637,#12637,#10457,.T.);
#16072=EDGE_CURVE('',#12638,#12638,#10458,.T.);
#16073=EDGE_CURVE('',#12638,#12637,#7164,.T.);
#16074=EDGE_CURVE('',#12638,#12622,#7165,.T.);
#16075=EDGE_CURVE('',#12639,#12640,#7166,.T.);
#16076=EDGE_CURVE('',#12640,#12641,#10459,.T.);
#16077=EDGE_CURVE('',#12641,#12642,#7167,.T.);
#16078=EDGE_CURVE('',#12642,#12639,#10460,.T.);
#16079=EDGE_CURVE('',#12643,#12644,#10461,.T.);
#16080=EDGE_CURVE('',#12644,#12641,#7168,.T.);
#16081=EDGE_CURVE('',#12640,#12643,#7169,.T.);
#16082=EDGE_CURVE('',#12645,#12646,#10462,.T.);
#16083=EDGE_CURVE('',#12647,#12646,#10463,.T.);
#16084=EDGE_CURVE('',#12647,#12648,#10464,.T.);
#16085=EDGE_CURVE('',#12648,#12645,#10465,.T.);
#16086=EDGE_CURVE('',#12649,#12650,#10466,.T.);
#16087=EDGE_CURVE('',#12651,#12650,#10467,.T.);
#16088=EDGE_CURVE('',#12651,#12652,#10468,.T.);
#16089=EDGE_CURVE('',#12652,#12649,#10469,.T.);
#16090=EDGE_CURVE('',#12653,#12654,#10470,.T.);
#16091=EDGE_CURVE('',#12654,#12649,#7170,.T.);
#16092=EDGE_CURVE('',#12652,#12653,#7171,.T.);
#16093=EDGE_CURVE('',#12655,#12645,#7172,.T.);
#16094=EDGE_CURVE('',#12648,#12656,#7173,.T.);
#16095=EDGE_CURVE('',#12656,#12655,#10471,.T.);
#16096=EDGE_CURVE('',#12657,#12651,#7174,.T.);
#16097=EDGE_CURVE('',#12657,#12653,#10472,.T.);
#16098=EDGE_CURVE('',#12658,#12647,#7175,.T.);
#16099=EDGE_CURVE('',#12658,#12656,#10473,.T.);
#16100=EDGE_CURVE('',#12654,#12659,#10474,.T.);
#16101=EDGE_CURVE('',#12650,#12659,#7176,.T.);
#16102=EDGE_CURVE('',#12655,#12660,#10475,.T.);
#16103=EDGE_CURVE('',#12646,#12660,#7177,.T.);
#16104=EDGE_CURVE('',#12659,#12658,#10476,.T.);
#16105=EDGE_CURVE('',#12660,#12661,#10477,.T.);
#16106=EDGE_CURVE('',#12661,#12644,#7178,.T.);
#16107=EDGE_CURVE('',#12643,#12662,#7179,.T.);
#16108=EDGE_CURVE('',#12662,#12657,#10478,.T.);
#16109=EDGE_CURVE('',#12663,#12664,#389,.T.);
#16110=EDGE_CURVE('',#12664,#12663,#390,.T.);
#16111=EDGE_CURVE('',#12665,#12666,#7180,.T.);
#16112=EDGE_CURVE('',#12666,#12665,#391,.T.);
#16113=EDGE_CURVE('',#12642,#12667,#7181,.T.);
#16114=EDGE_CURVE('',#12668,#12667,#10479,.T.);
#16115=EDGE_CURVE('',#12668,#12639,#7182,.T.);
#16116=EDGE_CURVE('',#12662,#12668,#7183,.T.);
#16117=EDGE_CURVE('',#12667,#12661,#7184,.T.);
#16118=EDGE_CURVE('',#12664,#12669,#7185,.T.);
#16119=EDGE_CURVE('',#12669,#12669,#10480,.T.);
#16120=EDGE_CURVE('',#12665,#12666,#10481,.T.);
#16121=EDGE_CURVE('',#12670,#12670,#10482,.T.);
#16122=EDGE_CURVE('',#12671,#12671,#10483,.T.);
#16123=EDGE_CURVE('',#12671,#12670,#7186,.T.);
#16124=EDGE_CURVE('',#12672,#12672,#10484,.T.);
#16125=EDGE_CURVE('',#12673,#12673,#10485,.T.);
#16126=EDGE_CURVE('',#12673,#12672,#7187,.T.);
#16127=EDGE_CURVE('',#12674,#12675,#10486,.T.);
#16128=EDGE_CURVE('',#12675,#12674,#392,.F.);
#16129=EDGE_CURVE('',#12676,#12677,#7188,.T.);
#16130=EDGE_CURVE('',#12678,#12676,#7189,.T.);
#16131=EDGE_CURVE('',#12679,#12678,#7190,.T.);
#16132=EDGE_CURVE('',#12680,#12679,#7191,.T.);
#16133=EDGE_CURVE('',#12677,#12680,#7192,.T.);
#16134=EDGE_CURVE('',#12681,#12681,#10487,.T.);
#16135=EDGE_CURVE('',#12682,#12683,#393,.F.);
#16136=EDGE_CURVE('',#12683,#12682,#394,.F.);
#16137=EDGE_CURVE('',#12683,#12681,#7193,.T.);
#16138=EDGE_CURVE('',#12684,#12684,#10488,.T.);
#16139=EDGE_CURVE('',#12684,#12685,#7194,.T.);
#16140=EDGE_CURVE('',#12685,#12685,#10489,.T.);
#16141=EDGE_CURVE('',#12686,#12686,#10490,.T.);
#16142=EDGE_CURVE('',#12686,#12687,#7195,.T.);
#16143=EDGE_CURVE('',#12687,#12687,#10491,.T.);
#16144=EDGE_CURVE('',#12674,#12675,#7196,.T.);
#16145=EDGE_CURVE('',#12688,#12689,#7197,.T.);
#16146=EDGE_CURVE('',#12690,#12688,#7198,.T.);
#16147=EDGE_CURVE('',#12691,#12690,#7199,.T.);
#16148=EDGE_CURVE('',#12692,#12691,#7200,.T.);
#16149=EDGE_CURVE('',#12689,#12692,#7201,.T.);
#16150=EDGE_CURVE('',#12692,#12693,#10492,.T.);
#16151=EDGE_CURVE('',#12693,#12694,#7202,.T.);
#16152=EDGE_CURVE('',#12694,#12695,#7203,.T.);
#16153=EDGE_CURVE('',#12695,#12696,#7204,.T.);
#16154=EDGE_CURVE('',#12696,#12678,#10493,.T.);
#16155=EDGE_CURVE('',#12676,#12689,#10494,.T.);
#16156=EDGE_CURVE('',#12677,#12688,#10495,.T.);
#16157=EDGE_CURVE('',#12697,#12690,#10496,.T.);
#16158=EDGE_CURVE('',#12698,#12697,#10497,.T.);
#16159=EDGE_CURVE('',#12699,#12698,#10498,.T.);
#16160=EDGE_CURVE('',#12700,#12699,#10499,.T.);
#16161=EDGE_CURVE('',#12701,#12700,#10500,.T.);
#16162=EDGE_CURVE('',#12702,#12701,#10501,.T.);
#16163=EDGE_CURVE('',#12703,#12702,#10502,.T.);
#16164=EDGE_CURVE('',#12704,#12703,#10503,.T.);
#16165=EDGE_CURVE('',#12680,#12704,#10504,.T.);
#16166=EDGE_CURVE('',#12679,#12705,#10505,.T.);
#16167=EDGE_CURVE('',#12705,#12706,#7205,.T.);
#16168=EDGE_CURVE('',#12706,#12707,#7206,.T.);
#16169=EDGE_CURVE('',#12707,#12708,#7207,.T.);
#16170=EDGE_CURVE('',#12708,#12691,#10506,.T.);
#16171=EDGE_CURVE('',#12705,#12696,#7208,.T.);
#16172=EDGE_CURVE('',#12693,#12708,#7209,.T.);
#16173=EDGE_CURVE('',#12709,#12710,#7210,.T.);
#16174=EDGE_CURVE('',#12710,#12711,#395,.T.);
#16175=EDGE_CURVE('',#12711,#12712,#7211,.T.);
#16176=EDGE_CURVE('',#12712,#12709,#10507,.T.);
#16177=EDGE_CURVE('',#12713,#12713,#10508,.T.);
#16178=EDGE_CURVE('',#12713,#12714,#7212,.T.);
#16179=EDGE_CURVE('',#12715,#12714,#396,.T.);
#16180=EDGE_CURVE('',#12716,#12715,#397,.T.);
#16181=EDGE_CURVE('',#12714,#12716,#398,.T.);
#16182=EDGE_CURVE('',#12707,#12694,#7213,.T.);
#16183=EDGE_CURVE('',#12695,#12706,#7214,.T.);
#16184=EDGE_CURVE('',#12717,#12718,#10509,.T.);
#16185=EDGE_CURVE('',#12704,#12717,#7215,.T.);
#16186=EDGE_CURVE('',#12718,#12703,#7216,.T.);
#16187=EDGE_CURVE('',#12719,#12720,#10510,.T.);
#16188=EDGE_CURVE('',#12700,#12719,#7217,.T.);
#16189=EDGE_CURVE('',#12720,#12699,#7218,.T.);
#16190=EDGE_CURVE('',#12721,#12697,#7219,.T.);
#16191=EDGE_CURVE('',#12722,#12721,#10511,.T.);
#16192=EDGE_CURVE('',#12698,#12722,#7220,.T.);
#16193=EDGE_CURVE('',#12718,#12723,#10512,.T.);
#16194=EDGE_CURVE('',#12702,#12723,#7221,.T.);
#16195=EDGE_CURVE('',#12720,#12722,#10513,.T.);
#16196=EDGE_CURVE('',#12724,#12701,#7222,.T.);
#16197=EDGE_CURVE('',#12723,#12724,#10514,.T.);
#16198=EDGE_CURVE('',#12719,#12721,#10515,.T.);
#16199=EDGE_CURVE('',#12717,#12724,#10516,.T.);
#16200=EDGE_CURVE('',#12725,#12726,#399,.F.);
#16201=EDGE_CURVE('',#12726,#12727,#10517,.T.);
#16202=EDGE_CURVE('',#12727,#12728,#7223,.T.);
#16203=EDGE_CURVE('',#12728,#12729,#10518,.T.);
#16204=EDGE_CURVE('',#12729,#12730,#7224,.T.);
#16205=EDGE_CURVE('',#12730,#12731,#10519,.T.);
#16206=EDGE_CURVE('',#12731,#12732,#7225,.T.);
#16207=EDGE_CURVE('',#12732,#12733,#10520,.T.);
#16208=EDGE_CURVE('',#12733,#12725,#7226,.T.);
#16209=EDGE_CURVE('',#12734,#12735,#10521,.T.);
#16210=EDGE_CURVE('',#12735,#12736,#7227,.T.);
#16211=EDGE_CURVE('',#12736,#12737,#10522,.T.);
#16212=EDGE_CURVE('',#12737,#12738,#7228,.T.);
#16213=EDGE_CURVE('',#12738,#12739,#10523,.T.);
#16214=EDGE_CURVE('',#12739,#12740,#7229,.T.);
#16215=EDGE_CURVE('',#12740,#12741,#10524,.T.);
#16216=EDGE_CURVE('',#12741,#12734,#7230,.T.);
#16217=EDGE_CURVE('',#12742,#12743,#7231,.T.);
#16218=EDGE_CURVE('',#12743,#12744,#679,.T.);
#16219=EDGE_CURVE('',#12744,#12745,#680,.T.);
#16220=EDGE_CURVE('',#12745,#12746,#7232,.T.);
#16221=EDGE_CURVE('',#12746,#12747,#681,.T.);
#16222=EDGE_CURVE('',#12747,#12742,#682,.T.);
#16223=EDGE_CURVE('',#12748,#12749,#683,.F.);
#16224=EDGE_CURVE('',#12749,#12750,#7233,.T.);
#16225=EDGE_CURVE('',#12750,#12751,#10525,.T.);
#16226=EDGE_CURVE('',#12751,#12752,#10526,.T.);
#16227=EDGE_CURVE('',#12752,#12753,#7234,.T.);
#16228=EDGE_CURVE('',#12753,#12754,#10527,.T.);
#16229=EDGE_CURVE('',#12754,#12755,#7235,.T.);
#16230=EDGE_CURVE('',#12755,#12756,#10528,.T.);
#16231=EDGE_CURVE('',#12756,#12757,#10529,.T.);
#16232=EDGE_CURVE('',#12757,#12758,#7236,.T.);
#16233=EDGE_CURVE('',#12758,#12748,#684,.T.);
#16234=EDGE_CURVE('',#12759,#12760,#685,.T.);
#16235=EDGE_CURVE('',#12760,#12761,#7237,.T.);
#16236=EDGE_CURVE('',#12761,#12762,#686,.T.);
#16237=EDGE_CURVE('',#12762,#12763,#687,.T.);
#16238=EDGE_CURVE('',#12763,#12764,#7238,.T.);
#16239=EDGE_CURVE('',#12764,#12759,#688,.T.);
#16240=EDGE_CURVE('',#12765,#12766,#10530,.T.);
#16241=EDGE_CURVE('',#12766,#12767,#7239,.T.);
#16242=EDGE_CURVE('',#12767,#12768,#10531,.T.);
#16243=EDGE_CURVE('',#12768,#12769,#7240,.T.);
#16244=EDGE_CURVE('',#12769,#12770,#10532,.T.);
#16245=EDGE_CURVE('',#12770,#12771,#7241,.T.);
#16246=EDGE_CURVE('',#12771,#12772,#10533,.T.);
#16247=EDGE_CURVE('',#12772,#12765,#7242,.T.);
#16248=EDGE_CURVE('',#12772,#12736,#7243,.T.);
#16249=EDGE_CURVE('',#12771,#12737,#7244,.T.);
#16250=EDGE_CURVE('',#12765,#12735,#7245,.T.);
#16251=EDGE_CURVE('',#12770,#12738,#7246,.T.);
#16252=EDGE_CURVE('',#12769,#12739,#7247,.T.);
#16253=EDGE_CURVE('',#12768,#12740,#7248,.T.);
#16254=EDGE_CURVE('',#12767,#12741,#7249,.T.);
#16255=EDGE_CURVE('',#12766,#12734,#7250,.T.);
#16256=EDGE_CURVE('',#12773,#12750,#7251,.T.);
#16257=EDGE_CURVE('',#12774,#12773,#689,.T.);
#16258=EDGE_CURVE('',#12774,#12751,#7252,.T.);
#16259=EDGE_CURVE('',#12775,#12749,#7253,.T.);
#16260=EDGE_CURVE('',#12773,#12775,#7254,.T.);
#16261=EDGE_CURVE('',#12776,#12748,#7255,.T.);
#16262=EDGE_CURVE('',#12775,#12776,#690,.F.);
#16263=EDGE_CURVE('',#12777,#12757,#7256,.T.);
#16264=EDGE_CURVE('',#12778,#12777,#7257,.T.);
#16265=EDGE_CURVE('',#12778,#12758,#7258,.T.);
#16266=EDGE_CURVE('',#12779,#12756,#7259,.T.);
#16267=EDGE_CURVE('',#12777,#12779,#10534,.T.);
#16268=EDGE_CURVE('',#12780,#12755,#7260,.T.);
#16269=EDGE_CURVE('',#12779,#12780,#10535,.T.);
#16270=EDGE_CURVE('',#12781,#12754,#7261,.T.);
#16271=EDGE_CURVE('',#12780,#12781,#7262,.T.);
#16272=EDGE_CURVE('',#12782,#12753,#7263,.T.);
#16273=EDGE_CURVE('',#12781,#12782,#10536,.T.);
#16274=EDGE_CURVE('',#12783,#12752,#7264,.T.);
#16275=EDGE_CURVE('',#12782,#12783,#7265,.T.);
#16276=EDGE_CURVE('',#12783,#12774,#10537,.T.);
#16277=EDGE_CURVE('',#12776,#12778,#691,.T.);
#16278=EDGE_CURVE('',#12784,#12785,#692,.T.);
#16279=EDGE_CURVE('',#12785,#12786,#7266,.T.);
#16280=EDGE_CURVE('',#12786,#12787,#693,.T.);
#16281=EDGE_CURVE('',#12787,#12788,#694,.T.);
#16282=EDGE_CURVE('',#12788,#12789,#7267,.T.);
#16283=EDGE_CURVE('',#12789,#12784,#695,.T.);
#16284=EDGE_CURVE('',#12787,#12744,#7268,.T.);
#16285=EDGE_CURVE('',#12786,#12745,#7269,.T.);
#16286=EDGE_CURVE('',#12788,#12743,#7270,.T.);
#16287=EDGE_CURVE('',#12785,#12746,#7271,.T.);
#16288=EDGE_CURVE('',#12784,#12747,#7272,.T.);
#16289=EDGE_CURVE('',#12789,#12742,#7273,.T.);
#16290=EDGE_CURVE('',#12790,#12763,#7274,.T.);
#16291=EDGE_CURVE('',#12791,#12790,#7275,.T.);
#16292=EDGE_CURVE('',#12791,#12764,#7276,.T.);
#16293=EDGE_CURVE('',#12792,#12762,#7277,.T.);
#16294=EDGE_CURVE('',#12790,#12792,#696,.T.);
#16295=EDGE_CURVE('',#12793,#12761,#7278,.T.);
#16296=EDGE_CURVE('',#12792,#12793,#697,.T.);
#16297=EDGE_CURVE('',#12794,#12760,#7279,.T.);
#16298=EDGE_CURVE('',#12793,#12794,#7280,.T.);
#16299=EDGE_CURVE('',#12795,#12791,#698,.T.);
#16300=EDGE_CURVE('',#12795,#12759,#7281,.T.);
#16301=EDGE_CURVE('',#12794,#12795,#699,.T.);
#16302=EDGE_CURVE('',#12796,#12728,#7282,.T.);
#16303=EDGE_CURVE('',#12797,#12796,#10538,.T.);
#16304=EDGE_CURVE('',#12797,#12729,#7283,.T.);
#16305=EDGE_CURVE('',#12798,#12727,#7284,.T.);
#16306=EDGE_CURVE('',#12796,#12798,#7285,.T.);
#16307=EDGE_CURVE('',#12799,#12726,#7286,.T.);
#16308=EDGE_CURVE('',#12798,#12799,#10539,.T.);
#16309=EDGE_CURVE('',#12800,#12725,#7287,.T.);
#16310=EDGE_CURVE('',#12799,#12800,#400,.F.);
#16311=EDGE_CURVE('',#12801,#12733,#7288,.T.);
#16312=EDGE_CURVE('',#12800,#12801,#7289,.T.);
#16313=EDGE_CURVE('',#12802,#12712,#7290,.T.);
#16314=EDGE_CURVE('',#12803,#12802,#10540,.T.);
#16315=EDGE_CURVE('',#12803,#12709,#7291,.T.);
#16316=EDGE_CURVE('',#12804,#12711,#7292,.T.);
#16317=EDGE_CURVE('',#12802,#12804,#7293,.T.);
#16318=EDGE_CURVE('',#12805,#12732,#7294,.T.);
#16319=EDGE_CURVE('',#12801,#12805,#10541,.T.);
#16320=EDGE_CURVE('',#12806,#12731,#7295,.T.);
#16321=EDGE_CURVE('',#12805,#12806,#7296,.T.);
#16322=EDGE_CURVE('',#12807,#12730,#7297,.T.);
#16323=EDGE_CURVE('',#12806,#12807,#10542,.T.);
#16324=EDGE_CURVE('',#12807,#12797,#7298,.T.);
#16325=EDGE_CURVE('',#12808,#12710,#7299,.T.);
#16326=EDGE_CURVE('',#12804,#12808,#401,.T.);
#16327=EDGE_CURVE('',#12808,#12803,#7300,.T.);
#16328=EDGE_CURVE('',#12809,#12809,#10543,.T.);
#16329=EDGE_CURVE('',#12809,#12810,#7301,.T.);
#16330=EDGE_CURVE('',#12810,#12810,#10544,.T.);
#16331=EDGE_CURVE('',#12811,#12809,#7302,.T.);
#16332=EDGE_CURVE('',#12812,#12812,#10545,.T.);
#16333=EDGE_CURVE('',#12812,#12813,#7303,.T.);
#16334=EDGE_CURVE('',#12813,#12813,#10546,.T.);
#16335=EDGE_CURVE('',#12814,#12812,#7304,.T.);
#16336=EDGE_CURVE('',#12815,#12815,#10547,.T.);
#16337=EDGE_CURVE('',#12815,#12816,#7305,.T.);
#16338=EDGE_CURVE('',#12816,#12816,#10548,.T.);
#16339=EDGE_CURVE('',#12817,#12815,#7306,.T.);
#16340=EDGE_CURVE('',#12818,#12818,#10549,.T.);
#16341=EDGE_CURVE('',#12818,#12819,#7307,.T.);
#16342=EDGE_CURVE('',#12819,#12819,#10550,.T.);
#16343=EDGE_CURVE('',#12820,#12818,#7308,.T.);
#16344=EDGE_CURVE('',#12821,#12821,#10551,.T.);
#16345=EDGE_CURVE('',#12821,#12822,#7309,.T.);
#16346=EDGE_CURVE('',#12822,#12822,#10552,.T.);
#16347=EDGE_CURVE('',#12823,#12821,#7310,.T.);
#16348=EDGE_CURVE('',#12824,#12824,#10553,.T.);
#16349=EDGE_CURVE('',#12824,#12825,#7311,.T.);
#16350=EDGE_CURVE('',#12825,#12825,#10554,.T.);
#16351=EDGE_CURVE('',#12826,#12824,#7312,.T.);
#16352=EDGE_CURVE('',#12827,#12827,#10555,.T.);
#16353=EDGE_CURVE('',#12827,#12828,#7313,.T.);
#16354=EDGE_CURVE('',#12828,#12828,#10556,.T.);
#16355=EDGE_CURVE('',#12829,#12827,#7314,.T.);
#16356=EDGE_CURVE('',#12830,#12830,#10557,.T.);
#16357=EDGE_CURVE('',#12830,#12831,#7315,.T.);
#16358=EDGE_CURVE('',#12831,#12831,#10558,.T.);
#16359=EDGE_CURVE('',#12832,#12830,#7316,.T.);
#16360=EDGE_CURVE('',#12833,#12833,#10559,.T.);
#16361=EDGE_CURVE('',#12833,#12834,#7317,.T.);
#16362=EDGE_CURVE('',#12834,#12834,#10560,.T.);
#16363=EDGE_CURVE('',#12835,#12833,#7318,.T.);
#16364=EDGE_CURVE('',#12836,#12836,#10561,.T.);
#16365=EDGE_CURVE('',#12836,#12837,#7319,.T.);
#16366=EDGE_CURVE('',#12837,#12837,#10562,.T.);
#16367=EDGE_CURVE('',#12838,#12836,#7320,.T.);
#16368=EDGE_CURVE('',#12839,#12839,#10563,.T.);
#16369=EDGE_CURVE('',#12839,#12840,#7321,.T.);
#16370=EDGE_CURVE('',#12840,#12840,#10564,.T.);
#16371=EDGE_CURVE('',#12841,#12839,#7322,.T.);
#16372=EDGE_CURVE('',#12842,#12842,#10565,.T.);
#16373=EDGE_CURVE('',#12842,#12843,#7323,.T.);
#16374=EDGE_CURVE('',#12843,#12843,#10566,.T.);
#16375=EDGE_CURVE('',#12844,#12842,#7324,.T.);
#16376=EDGE_CURVE('',#12845,#12845,#10567,.T.);
#16377=EDGE_CURVE('',#12845,#12846,#7325,.T.);
#16378=EDGE_CURVE('',#12846,#12846,#10568,.T.);
#16379=EDGE_CURVE('',#12847,#12845,#7326,.T.);
#16380=EDGE_CURVE('',#12848,#12848,#10569,.T.);
#16381=EDGE_CURVE('',#12848,#12849,#7327,.T.);
#16382=EDGE_CURVE('',#12849,#12849,#10570,.T.);
#16383=EDGE_CURVE('',#12850,#12848,#7328,.T.);
#16384=EDGE_CURVE('',#12851,#12851,#10571,.T.);
#16385=EDGE_CURVE('',#12851,#12852,#7329,.T.);
#16386=EDGE_CURVE('',#12852,#12852,#10572,.T.);
#16387=EDGE_CURVE('',#12853,#12851,#7330,.T.);
#16388=EDGE_CURVE('',#12854,#12854,#10573,.T.);
#16389=EDGE_CURVE('',#12854,#12855,#7331,.T.);
#16390=EDGE_CURVE('',#12855,#12855,#10574,.T.);
#16391=EDGE_CURVE('',#12856,#12854,#7332,.T.);
#16392=EDGE_CURVE('',#12857,#12857,#10575,.T.);
#16393=EDGE_CURVE('',#12857,#12858,#7333,.T.);
#16394=EDGE_CURVE('',#12858,#12858,#10576,.T.);
#16395=EDGE_CURVE('',#12859,#12857,#7334,.T.);
#16396=EDGE_CURVE('',#12860,#12861,#7335,.T.);
#16397=EDGE_CURVE('',#12861,#12862,#7336,.T.);
#16398=EDGE_CURVE('',#12863,#12862,#7337,.T.);
#16399=EDGE_CURVE('',#12860,#12863,#7338,.T.);
#16400=EDGE_CURVE('',#12864,#12862,#7339,.T.);
#16401=EDGE_CURVE('',#12864,#12865,#10577,.T.);
#16402=EDGE_CURVE('',#12866,#12865,#7340,.T.);
#16403=EDGE_CURVE('',#12866,#12867,#10578,.T.);
#16404=EDGE_CURVE('',#12868,#12867,#7341,.T.);
#16405=EDGE_CURVE('',#12868,#12869,#7342,.T.);
#16406=EDGE_CURVE('',#12869,#12870,#7343,.T.);
#16407=EDGE_CURVE('',#12871,#12870,#7344,.T.);
#16408=EDGE_CURVE('',#12863,#12871,#7345,.T.);
#16409=EDGE_CURVE('',#12870,#12872,#7346,.T.);
#16410=EDGE_CURVE('',#12873,#12872,#7347,.T.);
#16411=EDGE_CURVE('',#12871,#12873,#7348,.T.);
#16412=EDGE_CURVE('',#12874,#12875,#7349,.T.);
#16413=EDGE_CURVE('',#12875,#12876,#10579,.T.);
#16414=EDGE_CURVE('',#12876,#12877,#7350,.T.);
#16415=EDGE_CURVE('',#12877,#12878,#10580,.T.);
#16416=EDGE_CURVE('',#12878,#12861,#7351,.T.);
#16417=EDGE_CURVE('',#12873,#12860,#7352,.T.);
#16418=EDGE_CURVE('',#12872,#12879,#7353,.T.);
#16419=EDGE_CURVE('',#12874,#12879,#7354,.T.);
#16420=EDGE_CURVE('',#12874,#12868,#7355,.T.);
#16421=EDGE_CURVE('',#12879,#12869,#7356,.T.);
#16422=EDGE_CURVE('',#12878,#12864,#7357,.T.);
#16423=EDGE_CURVE('',#12876,#12866,#7358,.T.);
#16424=EDGE_CURVE('',#12865,#12877,#7359,.T.);
#16425=EDGE_CURVE('',#12867,#12875,#7360,.T.);
#16426=EDGE_CURVE('',#12880,#12880,#10581,.T.);
#16427=EDGE_CURVE('',#12880,#12881,#7361,.T.);
#16428=EDGE_CURVE('',#12881,#12881,#10582,.T.);
#16429=EDGE_CURVE('',#12881,#12882,#7362,.T.);
#16430=EDGE_CURVE('',#12882,#12882,#10583,.T.);
#16431=EDGE_CURVE('',#12883,#12884,#10584,.T.);
#16432=EDGE_CURVE('',#12884,#12885,#7363,.T.);
#16433=EDGE_CURVE('',#12885,#12885,#10585,.T.);
#16434=EDGE_CURVE('',#12884,#12883,#10586,.T.);
#16435=EDGE_CURVE('',#12883,#12886,#7364,.T.);
#16436=EDGE_CURVE('',#12886,#12886,#10587,.T.);
#16437=EDGE_CURVE('',#12887,#12888,#7365,.T.);
#16438=EDGE_CURVE('',#12889,#12887,#7366,.T.);
#16439=EDGE_CURVE('',#12890,#12889,#7367,.T.);
#16440=EDGE_CURVE('',#12891,#12890,#7368,.T.);
#16441=EDGE_CURVE('',#12892,#12891,#7369,.T.);
#16442=EDGE_CURVE('',#12888,#12892,#7370,.T.);
#16443=EDGE_CURVE('',#12893,#12888,#7371,.T.);
#16444=EDGE_CURVE('',#12894,#12893,#7372,.T.);
#16445=EDGE_CURVE('',#12894,#12887,#7373,.T.);
#16446=EDGE_CURVE('',#12895,#12894,#7374,.T.);
#16447=EDGE_CURVE('',#12895,#12889,#7375,.T.);
#16448=EDGE_CURVE('',#12896,#12895,#7376,.T.);
#16449=EDGE_CURVE('',#12896,#12890,#7377,.T.);
#16450=EDGE_CURVE('',#12897,#12896,#7378,.T.);
#16451=EDGE_CURVE('',#12897,#12891,#7379,.T.);
#16452=EDGE_CURVE('',#12898,#12897,#7380,.T.);
#16453=EDGE_CURVE('',#12898,#12892,#7381,.T.);
#16454=EDGE_CURVE('',#12893,#12898,#7382,.T.);
#16455=EDGE_CURVE('',#12899,#12900,#10588,.T.);
#16456=EDGE_CURVE('',#12900,#12899,#10589,.T.);
#16457=EDGE_CURVE('',#12900,#12901,#7383,.T.);
#16458=EDGE_CURVE('',#12901,#12901,#10590,.T.);
#16459=EDGE_CURVE('',#12902,#12903,#7384,.T.);
#16460=EDGE_CURVE('',#12903,#12904,#10591,.T.);
#16461=EDGE_CURVE('',#12904,#12905,#10592,.T.);
#16462=EDGE_CURVE('',#12905,#12906,#10593,.T.);
#16463=EDGE_CURVE('',#12906,#12907,#10594,.T.);
#16464=EDGE_CURVE('',#12907,#12908,#10595,.T.);
#16465=EDGE_CURVE('',#12908,#12909,#10596,.T.);
#16466=EDGE_CURVE('',#12909,#12903,#10597,.T.);
#16467=EDGE_CURVE('',#12899,#12910,#7385,.T.);
#16468=EDGE_CURVE('',#12910,#12910,#10598,.T.);
#16469=EDGE_CURVE('',#12911,#12911,#10599,.T.);
#16470=EDGE_CURVE('',#12911,#12912,#7386,.T.);
#16471=EDGE_CURVE('',#12912,#12912,#10600,.T.);
#16472=EDGE_CURVE('',#12913,#12913,#10601,.T.);
#16473=EDGE_CURVE('',#12913,#12914,#7387,.T.);
#16474=EDGE_CURVE('',#12914,#12914,#10602,.T.);
#16475=EDGE_CURVE('',#12915,#12916,#7388,.T.);
#16476=EDGE_CURVE('',#12917,#12915,#7389,.T.);
#16477=EDGE_CURVE('',#12918,#12917,#7390,.T.);
#16478=EDGE_CURVE('',#12919,#12918,#7391,.T.);
#16479=EDGE_CURVE('',#12920,#12919,#7392,.T.);
#16480=EDGE_CURVE('',#12916,#12920,#7393,.T.);
#16481=EDGE_CURVE('',#12921,#12908,#7394,.T.);
#16482=EDGE_CURVE('',#12921,#12917,#7395,.T.);
#16483=EDGE_CURVE('',#12922,#12915,#7396,.T.);
#16484=EDGE_CURVE('',#12908,#12922,#7397,.T.);
#16485=EDGE_CURVE('',#12923,#12907,#7398,.T.);
#16486=EDGE_CURVE('',#12923,#12918,#7399,.T.);
#16487=EDGE_CURVE('',#12907,#12921,#7400,.T.);
#16488=EDGE_CURVE('',#12924,#12906,#7401,.T.);
#16489=EDGE_CURVE('',#12924,#12919,#7402,.T.);
#16490=EDGE_CURVE('',#12906,#12923,#7403,.T.);
#16491=EDGE_CURVE('',#12925,#12905,#7404,.T.);
#16492=EDGE_CURVE('',#12925,#12920,#7405,.T.);
#16493=EDGE_CURVE('',#12905,#12924,#7406,.T.);
#16494=EDGE_CURVE('',#12926,#12904,#7407,.T.);
#16495=EDGE_CURVE('',#12926,#12916,#7408,.T.);
#16496=EDGE_CURVE('',#12904,#12925,#7409,.T.);
#16497=EDGE_CURVE('',#12922,#12909,#7410,.T.);
#16498=EDGE_CURVE('',#12909,#12926,#7411,.T.);
#16499=EDGE_CURVE('',#12927,#12927,#10603,.T.);
#16500=EDGE_CURVE('',#12927,#12928,#7412,.T.);
#16501=EDGE_CURVE('',#12928,#12928,#10604,.T.);
#16502=EDGE_CURVE('',#12929,#12929,#10605,.T.);
#16503=EDGE_CURVE('',#12929,#12930,#7413,.T.);
#16504=EDGE_CURVE('',#12930,#12930,#10606,.T.);
#16505=EDGE_CURVE('',#12931,#12932,#10607,.T.);
#16506=EDGE_CURVE('',#12933,#12932,#7414,.T.);
#16507=EDGE_CURVE('',#12934,#12933,#10608,.T.);
#16508=EDGE_CURVE('',#12934,#12931,#7415,.T.);
#16509=EDGE_CURVE('',#12935,#12936,#10609,.T.);
#16510=EDGE_CURVE('',#12937,#12935,#7416,.T.);
#16511=EDGE_CURVE('',#12937,#12938,#10610,.T.);
#16512=EDGE_CURVE('',#12938,#12936,#7417,.T.);
#16513=EDGE_CURVE('',#12933,#12938,#7418,.T.);
#16514=EDGE_CURVE('',#12937,#12934,#7419,.T.);
#16515=EDGE_CURVE('',#12932,#12936,#7420,.T.);
#16516=EDGE_CURVE('',#12935,#12931,#7421,.T.);
#16517=EDGE_CURVE('',#12939,#12939,#10611,.T.);
#16518=EDGE_CURVE('',#12939,#12940,#7422,.T.);
#16519=EDGE_CURVE('',#12940,#12940,#10612,.T.);
#16520=EDGE_CURVE('',#12941,#12941,#10613,.T.);
#16521=EDGE_CURVE('',#12941,#12942,#7423,.T.);
#16522=EDGE_CURVE('',#12942,#12942,#10614,.T.);
#16523=EDGE_CURVE('',#12943,#12943,#10615,.T.);
#16524=EDGE_CURVE('',#12943,#12944,#7424,.T.);
#16525=EDGE_CURVE('',#12944,#12944,#10616,.T.);
#16526=EDGE_CURVE('',#12945,#12945,#10617,.T.);
#16527=EDGE_CURVE('',#12945,#12946,#7425,.T.);
#16528=EDGE_CURVE('',#12946,#12946,#10618,.T.);
#16529=EDGE_CURVE('',#12947,#12947,#10619,.T.);
#16530=EDGE_CURVE('',#12947,#12948,#7426,.T.);
#16531=EDGE_CURVE('',#12948,#12948,#10620,.T.);
#16532=EDGE_CURVE('',#12949,#12949,#10621,.T.);
#16533=EDGE_CURVE('',#12949,#12950,#7427,.T.);
#16534=EDGE_CURVE('',#12950,#12950,#10622,.T.);
#16535=EDGE_CURVE('',#12951,#12951,#10623,.T.);
#16536=EDGE_CURVE('',#12951,#12952,#7428,.T.);
#16537=EDGE_CURVE('',#12952,#12952,#10624,.T.);
#16538=EDGE_CURVE('',#12953,#12953,#10625,.T.);
#16539=EDGE_CURVE('',#12953,#12954,#7429,.T.);
#16540=EDGE_CURVE('',#12954,#12954,#10626,.T.);
#16541=EDGE_CURVE('',#12955,#12955,#10627,.T.);
#16542=EDGE_CURVE('',#12955,#12956,#7430,.T.);
#16543=EDGE_CURVE('',#12956,#12956,#10628,.T.);
#16544=EDGE_CURVE('',#12957,#12957,#10629,.T.);
#16545=EDGE_CURVE('',#12957,#12958,#7431,.T.);
#16546=EDGE_CURVE('',#12958,#12958,#10630,.T.);
#16547=EDGE_CURVE('',#12959,#12960,#7432,.T.);
#16548=EDGE_CURVE('',#12961,#12959,#7433,.T.);
#16549=EDGE_CURVE('',#12962,#12961,#7434,.T.);
#16550=EDGE_CURVE('',#12960,#12962,#7435,.T.);
#16551=EDGE_CURVE('',#12963,#12961,#7436,.T.);
#16552=EDGE_CURVE('',#12964,#12963,#7437,.T.);
#16553=EDGE_CURVE('',#12964,#12962,#7438,.T.);
#16554=EDGE_CURVE('',#12959,#12965,#7439,.T.);
#16555=EDGE_CURVE('',#12965,#12966,#7440,.T.);
#16556=EDGE_CURVE('',#12967,#12966,#7441,.T.);
#16557=EDGE_CURVE('',#12963,#12967,#7442,.T.);
#16558=EDGE_CURVE('',#12966,#12968,#7443,.T.);
#16559=EDGE_CURVE('',#12969,#12968,#7444,.T.);
#16560=EDGE_CURVE('',#12967,#12969,#7445,.T.);
#16561=EDGE_CURVE('',#12968,#12970,#7446,.T.);
#16562=EDGE_CURVE('',#12970,#12960,#7447,.T.);
#16563=EDGE_CURVE('',#12969,#12964,#7448,.T.);
#16564=EDGE_CURVE('',#12965,#12970,#7449,.T.);
#16565=EDGE_CURVE('',#12971,#12971,#10631,.T.);
#16566=EDGE_CURVE('',#12971,#12972,#7450,.T.);
#16567=EDGE_CURVE('',#12972,#12972,#10632,.T.);
#16568=EDGE_CURVE('',#12972,#12973,#7451,.T.);
#16569=EDGE_CURVE('',#12973,#12973,#10633,.T.);
#16570=EDGE_CURVE('',#12974,#12975,#10634,.T.);
#16571=EDGE_CURVE('',#12975,#12976,#7452,.T.);
#16572=EDGE_CURVE('',#12976,#12976,#10635,.T.);
#16573=EDGE_CURVE('',#12975,#12974,#10636,.T.);
#16574=EDGE_CURVE('',#12974,#12977,#7453,.T.);
#16575=EDGE_CURVE('',#12977,#12977,#10637,.T.);
#16576=EDGE_CURVE('',#12978,#12979,#7454,.T.);
#16577=EDGE_CURVE('',#12980,#12978,#7455,.T.);
#16578=EDGE_CURVE('',#12981,#12980,#7456,.T.);
#16579=EDGE_CURVE('',#12982,#12981,#7457,.T.);
#16580=EDGE_CURVE('',#12983,#12982,#7458,.T.);
#16581=EDGE_CURVE('',#12979,#12983,#7459,.T.);
#16582=EDGE_CURVE('',#12984,#12979,#7460,.T.);
#16583=EDGE_CURVE('',#12985,#12984,#7461,.T.);
#16584=EDGE_CURVE('',#12985,#12978,#7462,.T.);
#16585=EDGE_CURVE('',#12986,#12985,#7463,.T.);
#16586=EDGE_CURVE('',#12986,#12980,#7464,.T.);
#16587=EDGE_CURVE('',#12987,#12986,#7465,.T.);
#16588=EDGE_CURVE('',#12987,#12981,#7466,.T.);
#16589=EDGE_CURVE('',#12988,#12987,#7467,.T.);
#16590=EDGE_CURVE('',#12988,#12982,#7468,.T.);
#16591=EDGE_CURVE('',#12989,#12988,#7469,.T.);
#16592=EDGE_CURVE('',#12989,#12983,#7470,.T.);
#16593=EDGE_CURVE('',#12984,#12989,#7471,.T.);
#16594=ORIENTED_EDGE('',*,*,#12990,.F.);
#16595=ORIENTED_EDGE('',*,*,#12991,.T.);
#16596=ORIENTED_EDGE('',*,*,#12992,.T.);
#16597=ORIENTED_EDGE('',*,*,#12991,.F.);
#16598=ORIENTED_EDGE('',*,*,#12993,.F.);
#16599=ORIENTED_EDGE('',*,*,#12994,.T.);
#16600=ORIENTED_EDGE('',*,*,#12995,.T.);
#16601=ORIENTED_EDGE('',*,*,#12994,.F.);
#16602=ORIENTED_EDGE('',*,*,#12996,.F.);
#16603=ORIENTED_EDGE('',*,*,#12997,.T.);
#16604=ORIENTED_EDGE('',*,*,#12998,.T.);
#16605=ORIENTED_EDGE('',*,*,#12997,.F.);
#16606=ORIENTED_EDGE('',*,*,#12999,.F.);
#16607=ORIENTED_EDGE('',*,*,#13000,.T.);
#16608=ORIENTED_EDGE('',*,*,#13001,.T.);
#16609=ORIENTED_EDGE('',*,*,#13000,.F.);
#16610=ORIENTED_EDGE('',*,*,#13002,.T.);
#16611=ORIENTED_EDGE('',*,*,#13003,.F.);
#16612=ORIENTED_EDGE('',*,*,#13004,.F.);
#16613=ORIENTED_EDGE('',*,*,#13005,.T.);
#16614=ORIENTED_EDGE('',*,*,#13006,.T.);
#16615=ORIENTED_EDGE('',*,*,#13007,.F.);
#16616=ORIENTED_EDGE('',*,*,#13008,.F.);
#16617=ORIENTED_EDGE('',*,*,#13003,.T.);
#16618=ORIENTED_EDGE('',*,*,#13009,.T.);
#16619=ORIENTED_EDGE('',*,*,#13010,.F.);
#16620=ORIENTED_EDGE('',*,*,#13011,.F.);
#16621=ORIENTED_EDGE('',*,*,#13007,.T.);
#16622=ORIENTED_EDGE('',*,*,#13012,.T.);
#16623=ORIENTED_EDGE('',*,*,#13005,.F.);
#16624=ORIENTED_EDGE('',*,*,#13013,.F.);
#16625=ORIENTED_EDGE('',*,*,#13010,.T.);
#16626=ORIENTED_EDGE('',*,*,#13004,.T.);
#16627=ORIENTED_EDGE('',*,*,#13008,.T.);
#16628=ORIENTED_EDGE('',*,*,#13011,.T.);
#16629=ORIENTED_EDGE('',*,*,#13013,.T.);
#16630=ORIENTED_EDGE('',*,*,#12992,.F.);
#16631=ORIENTED_EDGE('',*,*,#12995,.F.);
#16632=ORIENTED_EDGE('',*,*,#12998,.F.);
#16633=ORIENTED_EDGE('',*,*,#13001,.F.);
#16634=ORIENTED_EDGE('',*,*,#13014,.F.);
#16635=ORIENTED_EDGE('',*,*,#13015,.F.);
#16636=ORIENTED_EDGE('',*,*,#13016,.F.);
#16637=ORIENTED_EDGE('',*,*,#13017,.F.);
#16638=ORIENTED_EDGE('',*,*,#13018,.F.);
#16639=ORIENTED_EDGE('',*,*,#13019,.F.);
#16640=ORIENTED_EDGE('',*,*,#13020,.F.);
#16641=ORIENTED_EDGE('',*,*,#13021,.F.);
#16642=ORIENTED_EDGE('',*,*,#13002,.F.);
#16643=ORIENTED_EDGE('',*,*,#13012,.F.);
#16644=ORIENTED_EDGE('',*,*,#13009,.F.);
#16645=ORIENTED_EDGE('',*,*,#13006,.F.);
#16646=ORIENTED_EDGE('',*,*,#12990,.T.);
#16647=ORIENTED_EDGE('',*,*,#12993,.T.);
#16648=ORIENTED_EDGE('',*,*,#12996,.T.);
#16649=ORIENTED_EDGE('',*,*,#12999,.T.);
#16650=ORIENTED_EDGE('',*,*,#13022,.T.);
#16651=ORIENTED_EDGE('',*,*,#13023,.T.);
#16652=ORIENTED_EDGE('',*,*,#13024,.T.);
#16653=ORIENTED_EDGE('',*,*,#13025,.T.);
#16654=ORIENTED_EDGE('',*,*,#13026,.T.);
#16655=ORIENTED_EDGE('',*,*,#13027,.T.);
#16656=ORIENTED_EDGE('',*,*,#13028,.T.);
#16657=ORIENTED_EDGE('',*,*,#13029,.T.);
#16658=ORIENTED_EDGE('',*,*,#13019,.T.);
#16659=ORIENTED_EDGE('',*,*,#13030,.F.);
#16660=ORIENTED_EDGE('',*,*,#13026,.F.);
#16661=ORIENTED_EDGE('',*,*,#13031,.T.);
#16662=ORIENTED_EDGE('',*,*,#13020,.T.);
#16663=ORIENTED_EDGE('',*,*,#13031,.F.);
#16664=ORIENTED_EDGE('',*,*,#13029,.F.);
#16665=ORIENTED_EDGE('',*,*,#13032,.T.);
#16666=ORIENTED_EDGE('',*,*,#13021,.T.);
#16667=ORIENTED_EDGE('',*,*,#13032,.F.);
#16668=ORIENTED_EDGE('',*,*,#13028,.F.);
#16669=ORIENTED_EDGE('',*,*,#13033,.T.);
#16670=ORIENTED_EDGE('',*,*,#13018,.T.);
#16671=ORIENTED_EDGE('',*,*,#13033,.F.);
#16672=ORIENTED_EDGE('',*,*,#13027,.F.);
#16673=ORIENTED_EDGE('',*,*,#13030,.T.);
#16674=ORIENTED_EDGE('',*,*,#13015,.T.);
#16675=ORIENTED_EDGE('',*,*,#13034,.F.);
#16676=ORIENTED_EDGE('',*,*,#13022,.F.);
#16677=ORIENTED_EDGE('',*,*,#13035,.T.);
#16678=ORIENTED_EDGE('',*,*,#13016,.T.);
#16679=ORIENTED_EDGE('',*,*,#13035,.F.);
#16680=ORIENTED_EDGE('',*,*,#13025,.F.);
#16681=ORIENTED_EDGE('',*,*,#13036,.T.);
#16682=ORIENTED_EDGE('',*,*,#13017,.T.);
#16683=ORIENTED_EDGE('',*,*,#13036,.F.);
#16684=ORIENTED_EDGE('',*,*,#13024,.F.);
#16685=ORIENTED_EDGE('',*,*,#13037,.T.);
#16686=ORIENTED_EDGE('',*,*,#13014,.T.);
#16687=ORIENTED_EDGE('',*,*,#13037,.F.);
#16688=ORIENTED_EDGE('',*,*,#13023,.F.);
#16689=ORIENTED_EDGE('',*,*,#13034,.T.);
#16690=ORIENTED_EDGE('',*,*,#13038,.F.);
#16691=ORIENTED_EDGE('',*,*,#13039,.T.);
#16692=ORIENTED_EDGE('',*,*,#13040,.T.);
#16693=ORIENTED_EDGE('',*,*,#13039,.F.);
#16694=ORIENTED_EDGE('',*,*,#13041,.F.);
#16695=ORIENTED_EDGE('',*,*,#13042,.T.);
#16696=ORIENTED_EDGE('',*,*,#13043,.T.);
#16697=ORIENTED_EDGE('',*,*,#13042,.F.);
#16698=ORIENTED_EDGE('',*,*,#13044,.F.);
#16699=ORIENTED_EDGE('',*,*,#13045,.T.);
#16700=ORIENTED_EDGE('',*,*,#13046,.T.);
#16701=ORIENTED_EDGE('',*,*,#13045,.F.);
#16702=ORIENTED_EDGE('',*,*,#13047,.F.);
#16703=ORIENTED_EDGE('',*,*,#13048,.T.);
#16704=ORIENTED_EDGE('',*,*,#13049,.T.);
#16705=ORIENTED_EDGE('',*,*,#13048,.F.);
#16706=ORIENTED_EDGE('',*,*,#13050,.F.);
#16707=ORIENTED_EDGE('',*,*,#13051,.F.);
#16708=ORIENTED_EDGE('',*,*,#13052,.T.);
#16709=ORIENTED_EDGE('',*,*,#13053,.T.);
#16710=ORIENTED_EDGE('',*,*,#13052,.F.);
#16711=ORIENTED_EDGE('',*,*,#13054,.F.);
#16712=ORIENTED_EDGE('',*,*,#13055,.F.);
#16713=ORIENTED_EDGE('',*,*,#13056,.T.);
#16714=ORIENTED_EDGE('',*,*,#13057,.T.);
#16715=ORIENTED_EDGE('',*,*,#13058,.F.);
#16716=ORIENTED_EDGE('',*,*,#13059,.F.);
#16717=ORIENTED_EDGE('',*,*,#13060,.T.);
#16718=ORIENTED_EDGE('',*,*,#13053,.F.);
#16719=ORIENTED_EDGE('',*,*,#13058,.T.);
#16720=ORIENTED_EDGE('',*,*,#13061,.T.);
#16721=ORIENTED_EDGE('',*,*,#13062,.F.);
#16722=ORIENTED_EDGE('',*,*,#13063,.F.);
#16723=ORIENTED_EDGE('',*,*,#13064,.F.);
#16724=ORIENTED_EDGE('',*,*,#13065,.F.);
#16725=ORIENTED_EDGE('',*,*,#13062,.T.);
#16726=ORIENTED_EDGE('',*,*,#13066,.T.);
#16727=ORIENTED_EDGE('',*,*,#13067,.F.);
#16728=ORIENTED_EDGE('',*,*,#13068,.F.);
#16729=ORIENTED_EDGE('',*,*,#13069,.T.);
#16730=ORIENTED_EDGE('',*,*,#13070,.F.);
#16731=ORIENTED_EDGE('',*,*,#13067,.T.);
#16732=ORIENTED_EDGE('',*,*,#13071,.T.);
#16733=ORIENTED_EDGE('',*,*,#13056,.F.);
#16734=ORIENTED_EDGE('',*,*,#13072,.F.);
#16735=ORIENTED_EDGE('',*,*,#13073,.F.);
#16736=ORIENTED_EDGE('',*,*,#13063,.T.);
#16737=ORIENTED_EDGE('',*,*,#13070,.T.);
#16738=ORIENTED_EDGE('',*,*,#13057,.F.);
#16739=ORIENTED_EDGE('',*,*,#13071,.F.);
#16740=ORIENTED_EDGE('',*,*,#13066,.F.);
#16741=ORIENTED_EDGE('',*,*,#13061,.F.);
#16742=ORIENTED_EDGE('',*,*,#13038,.T.);
#16743=ORIENTED_EDGE('',*,*,#13041,.T.);
#16744=ORIENTED_EDGE('',*,*,#13044,.T.);
#16745=ORIENTED_EDGE('',*,*,#13047,.T.);
#16746=ORIENTED_EDGE('',*,*,#13050,.T.);
#16747=ORIENTED_EDGE('',*,*,#13060,.F.);
#16748=ORIENTED_EDGE('',*,*,#13074,.F.);
#16749=ORIENTED_EDGE('',*,*,#13075,.T.);
#16750=ORIENTED_EDGE('',*,*,#13051,.T.);
#16751=ORIENTED_EDGE('',*,*,#13075,.F.);
#16752=ORIENTED_EDGE('',*,*,#13076,.F.);
#16753=ORIENTED_EDGE('',*,*,#13054,.T.);
#16754=ORIENTED_EDGE('',*,*,#13072,.T.);
#16755=ORIENTED_EDGE('',*,*,#13069,.F.);
#16756=ORIENTED_EDGE('',*,*,#13077,.F.);
#16757=ORIENTED_EDGE('',*,*,#13078,.T.);
#16758=ORIENTED_EDGE('',*,*,#13073,.T.);
#16759=ORIENTED_EDGE('',*,*,#13078,.F.);
#16760=ORIENTED_EDGE('',*,*,#13079,.F.);
#16761=ORIENTED_EDGE('',*,*,#13064,.T.);
#16762=ORIENTED_EDGE('',*,*,#13065,.T.);
#16763=ORIENTED_EDGE('',*,*,#13079,.T.);
#16764=ORIENTED_EDGE('',*,*,#13077,.T.);
#16765=ORIENTED_EDGE('',*,*,#13068,.T.);
#16766=ORIENTED_EDGE('',*,*,#13055,.T.);
#16767=ORIENTED_EDGE('',*,*,#13076,.T.);
#16768=ORIENTED_EDGE('',*,*,#13074,.T.);
#16769=ORIENTED_EDGE('',*,*,#13059,.T.);
#16770=ORIENTED_EDGE('',*,*,#13040,.F.);
#16771=ORIENTED_EDGE('',*,*,#13043,.F.);
#16772=ORIENTED_EDGE('',*,*,#13046,.F.);
#16773=ORIENTED_EDGE('',*,*,#13049,.F.);
#16774=ORIENTED_EDGE('',*,*,#13080,.F.);
#16775=ORIENTED_EDGE('',*,*,#13081,.T.);
#16776=ORIENTED_EDGE('',*,*,#13082,.T.);
#16777=ORIENTED_EDGE('',*,*,#13081,.F.);
#16778=ORIENTED_EDGE('',*,*,#13083,.F.);
#16779=ORIENTED_EDGE('',*,*,#13084,.T.);
#16780=ORIENTED_EDGE('',*,*,#13085,.T.);
#16781=ORIENTED_EDGE('',*,*,#13084,.F.);
#16782=ORIENTED_EDGE('',*,*,#13086,.F.);
#16783=ORIENTED_EDGE('',*,*,#13087,.T.);
#16784=ORIENTED_EDGE('',*,*,#13088,.T.);
#16785=ORIENTED_EDGE('',*,*,#13087,.F.);
#16786=ORIENTED_EDGE('',*,*,#13089,.F.);
#16787=ORIENTED_EDGE('',*,*,#13090,.T.);
#16788=ORIENTED_EDGE('',*,*,#13091,.T.);
#16789=ORIENTED_EDGE('',*,*,#13090,.F.);
#16790=ORIENTED_EDGE('',*,*,#13092,.F.);
#16791=ORIENTED_EDGE('',*,*,#13093,.T.);
#16792=ORIENTED_EDGE('',*,*,#13094,.T.);
#16793=ORIENTED_EDGE('',*,*,#13093,.F.);
#16794=ORIENTED_EDGE('',*,*,#13095,.F.);
#16795=ORIENTED_EDGE('',*,*,#13096,.T.);
#16796=ORIENTED_EDGE('',*,*,#13097,.T.);
#16797=ORIENTED_EDGE('',*,*,#13096,.F.);
#16798=ORIENTED_EDGE('',*,*,#13098,.F.);
#16799=ORIENTED_EDGE('',*,*,#13099,.T.);
#16800=ORIENTED_EDGE('',*,*,#13100,.T.);
#16801=ORIENTED_EDGE('',*,*,#13099,.F.);
#16802=ORIENTED_EDGE('',*,*,#13101,.F.);
#16803=ORIENTED_EDGE('',*,*,#13102,.T.);
#16804=ORIENTED_EDGE('',*,*,#13103,.T.);
#16805=ORIENTED_EDGE('',*,*,#13102,.F.);
#16806=ORIENTED_EDGE('',*,*,#13104,.F.);
#16807=ORIENTED_EDGE('',*,*,#13105,.T.);
#16808=ORIENTED_EDGE('',*,*,#13106,.T.);
#16809=ORIENTED_EDGE('',*,*,#13105,.F.);
#16810=ORIENTED_EDGE('',*,*,#13107,.F.);
#16811=ORIENTED_EDGE('',*,*,#13108,.T.);
#16812=ORIENTED_EDGE('',*,*,#13109,.T.);
#16813=ORIENTED_EDGE('',*,*,#13108,.F.);
#16814=ORIENTED_EDGE('',*,*,#13110,.F.);
#16815=ORIENTED_EDGE('',*,*,#13111,.T.);
#16816=ORIENTED_EDGE('',*,*,#13112,.T.);
#16817=ORIENTED_EDGE('',*,*,#13111,.F.);
#16818=ORIENTED_EDGE('',*,*,#13113,.F.);
#16819=ORIENTED_EDGE('',*,*,#13114,.T.);
#16820=ORIENTED_EDGE('',*,*,#13115,.T.);
#16821=ORIENTED_EDGE('',*,*,#13114,.F.);
#16822=ORIENTED_EDGE('',*,*,#13116,.F.);
#16823=ORIENTED_EDGE('',*,*,#13117,.F.);
#16824=ORIENTED_EDGE('',*,*,#13118,.F.);
#16825=ORIENTED_EDGE('',*,*,#13119,.F.);
#16826=ORIENTED_EDGE('',*,*,#13110,.T.);
#16827=ORIENTED_EDGE('',*,*,#13107,.T.);
#16828=ORIENTED_EDGE('',*,*,#13101,.T.);
#16829=ORIENTED_EDGE('',*,*,#13095,.T.);
#16830=ORIENTED_EDGE('',*,*,#13092,.T.);
#16831=ORIENTED_EDGE('',*,*,#13089,.T.);
#16832=ORIENTED_EDGE('',*,*,#13086,.T.);
#16833=ORIENTED_EDGE('',*,*,#13080,.T.);
#16834=ORIENTED_EDGE('',*,*,#13083,.T.);
#16835=ORIENTED_EDGE('',*,*,#13116,.T.);
#16836=ORIENTED_EDGE('',*,*,#13120,.F.);
#16837=ORIENTED_EDGE('',*,*,#13121,.F.);
#16838=ORIENTED_EDGE('',*,*,#13122,.T.);
#16839=ORIENTED_EDGE('',*,*,#13119,.T.);
#16840=ORIENTED_EDGE('',*,*,#13123,.F.);
#16841=ORIENTED_EDGE('',*,*,#13124,.F.);
#16842=ORIENTED_EDGE('',*,*,#13120,.T.);
#16843=ORIENTED_EDGE('',*,*,#13118,.T.);
#16844=ORIENTED_EDGE('',*,*,#13125,.F.);
#16845=ORIENTED_EDGE('',*,*,#13126,.F.);
#16846=ORIENTED_EDGE('',*,*,#13123,.T.);
#16847=ORIENTED_EDGE('',*,*,#13117,.T.);
#16848=ORIENTED_EDGE('',*,*,#13122,.F.);
#16849=ORIENTED_EDGE('',*,*,#13127,.F.);
#16850=ORIENTED_EDGE('',*,*,#13125,.T.);
#16851=ORIENTED_EDGE('',*,*,#13121,.T.);
#16852=ORIENTED_EDGE('',*,*,#13124,.T.);
#16853=ORIENTED_EDGE('',*,*,#13126,.T.);
#16854=ORIENTED_EDGE('',*,*,#13127,.T.);
#16855=ORIENTED_EDGE('',*,*,#13082,.F.);
#16856=ORIENTED_EDGE('',*,*,#13085,.F.);
#16857=ORIENTED_EDGE('',*,*,#13088,.F.);
#16858=ORIENTED_EDGE('',*,*,#13091,.F.);
#16859=ORIENTED_EDGE('',*,*,#13094,.F.);
#16860=ORIENTED_EDGE('',*,*,#13097,.F.);
#16861=ORIENTED_EDGE('',*,*,#13100,.F.);
#16862=ORIENTED_EDGE('',*,*,#13106,.F.);
#16863=ORIENTED_EDGE('',*,*,#13115,.F.);
#16864=ORIENTED_EDGE('',*,*,#13113,.T.);
#16865=ORIENTED_EDGE('',*,*,#13112,.F.);
#16866=ORIENTED_EDGE('',*,*,#13104,.T.);
#16867=ORIENTED_EDGE('',*,*,#13109,.F.);
#16868=ORIENTED_EDGE('',*,*,#13098,.T.);
#16869=ORIENTED_EDGE('',*,*,#13103,.F.);
#16870=ORIENTED_EDGE('',*,*,#13128,.F.);
#16871=ORIENTED_EDGE('',*,*,#13129,.T.);
#16872=ORIENTED_EDGE('',*,*,#13130,.T.);
#16873=ORIENTED_EDGE('',*,*,#13129,.F.);
#16874=ORIENTED_EDGE('',*,*,#13131,.F.);
#16875=ORIENTED_EDGE('',*,*,#13132,.T.);
#16876=ORIENTED_EDGE('',*,*,#13133,.T.);
#16877=ORIENTED_EDGE('',*,*,#13132,.F.);
#16878=ORIENTED_EDGE('',*,*,#13134,.F.);
#16879=ORIENTED_EDGE('',*,*,#13135,.T.);
#16880=ORIENTED_EDGE('',*,*,#13136,.T.);
#16881=ORIENTED_EDGE('',*,*,#13135,.F.);
#16882=ORIENTED_EDGE('',*,*,#13137,.F.);
#16883=ORIENTED_EDGE('',*,*,#13138,.T.);
#16884=ORIENTED_EDGE('',*,*,#13139,.T.);
#16885=ORIENTED_EDGE('',*,*,#13138,.F.);
#16886=ORIENTED_EDGE('',*,*,#13140,.F.);
#16887=ORIENTED_EDGE('',*,*,#13141,.T.);
#16888=ORIENTED_EDGE('',*,*,#13142,.T.);
#16889=ORIENTED_EDGE('',*,*,#13141,.F.);
#16890=ORIENTED_EDGE('',*,*,#13143,.F.);
#16891=ORIENTED_EDGE('',*,*,#13144,.T.);
#16892=ORIENTED_EDGE('',*,*,#13145,.T.);
#16893=ORIENTED_EDGE('',*,*,#13144,.F.);
#16894=ORIENTED_EDGE('',*,*,#13146,.F.);
#16895=ORIENTED_EDGE('',*,*,#13147,.T.);
#16896=ORIENTED_EDGE('',*,*,#13148,.T.);
#16897=ORIENTED_EDGE('',*,*,#13147,.F.);
#16898=ORIENTED_EDGE('',*,*,#13149,.F.);
#16899=ORIENTED_EDGE('',*,*,#13150,.T.);
#16900=ORIENTED_EDGE('',*,*,#13151,.F.);
#16901=ORIENTED_EDGE('',*,*,#13152,.T.);
#16902=ORIENTED_EDGE('',*,*,#13153,.T.);
#16903=ORIENTED_EDGE('',*,*,#13154,.T.);
#16904=ORIENTED_EDGE('',*,*,#13136,.F.);
#16905=ORIENTED_EDGE('',*,*,#13130,.F.);
#16906=ORIENTED_EDGE('',*,*,#13133,.F.);
#16907=ORIENTED_EDGE('',*,*,#13139,.F.);
#16908=ORIENTED_EDGE('',*,*,#13142,.F.);
#16909=ORIENTED_EDGE('',*,*,#13145,.F.);
#16910=ORIENTED_EDGE('',*,*,#13148,.F.);
#16911=ORIENTED_EDGE('',*,*,#13155,.F.);
#16912=ORIENTED_EDGE('',*,*,#13156,.T.);
#16913=ORIENTED_EDGE('',*,*,#13149,.T.);
#16914=ORIENTED_EDGE('',*,*,#13157,.T.);
#16915=ORIENTED_EDGE('',*,*,#13158,.F.);
#16916=ORIENTED_EDGE('',*,*,#13159,.T.);
#16917=ORIENTED_EDGE('',*,*,#13155,.T.);
#16918=ORIENTED_EDGE('',*,*,#13160,.T.);
#16919=ORIENTED_EDGE('',*,*,#13161,.T.);
#16920=ORIENTED_EDGE('',*,*,#13162,.F.);
#16921=ORIENTED_EDGE('',*,*,#13128,.T.);
#16922=ORIENTED_EDGE('',*,*,#13131,.T.);
#16923=ORIENTED_EDGE('',*,*,#13134,.T.);
#16924=ORIENTED_EDGE('',*,*,#13137,.T.);
#16925=ORIENTED_EDGE('',*,*,#13140,.T.);
#16926=ORIENTED_EDGE('',*,*,#13143,.T.);
#16927=ORIENTED_EDGE('',*,*,#13146,.T.);
#16928=ORIENTED_EDGE('',*,*,#13163,.T.);
#16929=ORIENTED_EDGE('',*,*,#13152,.F.);
#16930=ORIENTED_EDGE('',*,*,#13164,.F.);
#16931=ORIENTED_EDGE('',*,*,#13162,.T.);
#16932=ORIENTED_EDGE('',*,*,#13151,.T.);
#16933=ORIENTED_EDGE('',*,*,#13165,.T.);
#16934=ORIENTED_EDGE('',*,*,#13158,.T.);
#16935=ORIENTED_EDGE('',*,*,#13164,.T.);
#16936=ORIENTED_EDGE('',*,*,#13161,.F.);
#16937=ORIENTED_EDGE('',*,*,#13166,.T.);
#16938=ORIENTED_EDGE('',*,*,#13153,.F.);
#16939=ORIENTED_EDGE('',*,*,#13163,.F.);
#16940=ORIENTED_EDGE('',*,*,#13150,.F.);
#16941=ORIENTED_EDGE('',*,*,#13156,.F.);
#16942=ORIENTED_EDGE('',*,*,#13159,.F.);
#16943=ORIENTED_EDGE('',*,*,#13165,.F.);
#16944=ORIENTED_EDGE('',*,*,#13154,.F.);
#16945=ORIENTED_EDGE('',*,*,#13166,.F.);
#16946=ORIENTED_EDGE('',*,*,#13160,.F.);
#16947=ORIENTED_EDGE('',*,*,#13157,.F.);
#16948=ORIENTED_EDGE('',*,*,#13167,.F.);
#16949=ORIENTED_EDGE('',*,*,#13168,.T.);
#16950=ORIENTED_EDGE('',*,*,#13169,.T.);
#16951=ORIENTED_EDGE('',*,*,#13168,.F.);
#16952=ORIENTED_EDGE('',*,*,#13170,.F.);
#16953=ORIENTED_EDGE('',*,*,#13171,.T.);
#16954=ORIENTED_EDGE('',*,*,#13172,.T.);
#16955=ORIENTED_EDGE('',*,*,#13171,.F.);
#16956=ORIENTED_EDGE('',*,*,#13173,.F.);
#16957=ORIENTED_EDGE('',*,*,#13174,.T.);
#16958=ORIENTED_EDGE('',*,*,#13175,.T.);
#16959=ORIENTED_EDGE('',*,*,#13174,.F.);
#16960=ORIENTED_EDGE('',*,*,#13176,.F.);
#16961=ORIENTED_EDGE('',*,*,#13177,.T.);
#16962=ORIENTED_EDGE('',*,*,#13178,.T.);
#16963=ORIENTED_EDGE('',*,*,#13177,.F.);
#16964=ORIENTED_EDGE('',*,*,#13179,.F.);
#16965=ORIENTED_EDGE('',*,*,#13180,.T.);
#16966=ORIENTED_EDGE('',*,*,#13181,.T.);
#16967=ORIENTED_EDGE('',*,*,#13180,.F.);
#16968=ORIENTED_EDGE('',*,*,#13182,.F.);
#16969=ORIENTED_EDGE('',*,*,#13183,.T.);
#16970=ORIENTED_EDGE('',*,*,#13184,.T.);
#16971=ORIENTED_EDGE('',*,*,#13183,.F.);
#16972=ORIENTED_EDGE('',*,*,#13185,.T.);
#16973=ORIENTED_EDGE('',*,*,#13186,.F.);
#16974=ORIENTED_EDGE('',*,*,#13187,.F.);
#16975=ORIENTED_EDGE('',*,*,#13188,.T.);
#16976=ORIENTED_EDGE('',*,*,#13189,.T.);
#16977=ORIENTED_EDGE('',*,*,#13190,.F.);
#16978=ORIENTED_EDGE('',*,*,#13191,.F.);
#16979=ORIENTED_EDGE('',*,*,#13186,.T.);
#16980=ORIENTED_EDGE('',*,*,#13192,.T.);
#16981=ORIENTED_EDGE('',*,*,#13193,.F.);
#16982=ORIENTED_EDGE('',*,*,#13194,.F.);
#16983=ORIENTED_EDGE('',*,*,#13190,.T.);
#16984=ORIENTED_EDGE('',*,*,#13195,.T.);
#16985=ORIENTED_EDGE('',*,*,#13188,.F.);
#16986=ORIENTED_EDGE('',*,*,#13196,.F.);
#16987=ORIENTED_EDGE('',*,*,#13193,.T.);
#16988=ORIENTED_EDGE('',*,*,#13187,.T.);
#16989=ORIENTED_EDGE('',*,*,#13191,.T.);
#16990=ORIENTED_EDGE('',*,*,#13194,.T.);
#16991=ORIENTED_EDGE('',*,*,#13196,.T.);
#16992=ORIENTED_EDGE('',*,*,#13169,.F.);
#16993=ORIENTED_EDGE('',*,*,#13172,.F.);
#16994=ORIENTED_EDGE('',*,*,#13175,.F.);
#16995=ORIENTED_EDGE('',*,*,#13178,.F.);
#16996=ORIENTED_EDGE('',*,*,#13181,.F.);
#16997=ORIENTED_EDGE('',*,*,#13184,.F.);
#16998=ORIENTED_EDGE('',*,*,#13185,.F.);
#16999=ORIENTED_EDGE('',*,*,#13195,.F.);
#17000=ORIENTED_EDGE('',*,*,#13192,.F.);
#17001=ORIENTED_EDGE('',*,*,#13189,.F.);
#17002=ORIENTED_EDGE('',*,*,#13167,.T.);
#17003=ORIENTED_EDGE('',*,*,#13170,.T.);
#17004=ORIENTED_EDGE('',*,*,#13173,.T.);
#17005=ORIENTED_EDGE('',*,*,#13176,.T.);
#17006=ORIENTED_EDGE('',*,*,#13179,.T.);
#17007=ORIENTED_EDGE('',*,*,#13182,.T.);
#17008=ORIENTED_EDGE('',*,*,#13197,.F.);
#17009=ORIENTED_EDGE('',*,*,#13198,.T.);
#17010=ORIENTED_EDGE('',*,*,#13199,.T.);
#17011=ORIENTED_EDGE('',*,*,#13198,.F.);
#17012=ORIENTED_EDGE('',*,*,#13200,.F.);
#17013=ORIENTED_EDGE('',*,*,#13201,.T.);
#17014=ORIENTED_EDGE('',*,*,#13202,.T.);
#17015=ORIENTED_EDGE('',*,*,#13201,.F.);
#17016=ORIENTED_EDGE('',*,*,#13203,.F.);
#17017=ORIENTED_EDGE('',*,*,#13204,.T.);
#17018=ORIENTED_EDGE('',*,*,#13205,.T.);
#17019=ORIENTED_EDGE('',*,*,#13204,.F.);
#17020=ORIENTED_EDGE('',*,*,#13206,.F.);
#17021=ORIENTED_EDGE('',*,*,#13207,.T.);
#17022=ORIENTED_EDGE('',*,*,#13208,.T.);
#17023=ORIENTED_EDGE('',*,*,#13207,.F.);
#17024=ORIENTED_EDGE('',*,*,#13209,.F.);
#17025=ORIENTED_EDGE('',*,*,#13210,.T.);
#17026=ORIENTED_EDGE('',*,*,#13211,.T.);
#17027=ORIENTED_EDGE('',*,*,#13210,.F.);
#17028=ORIENTED_EDGE('',*,*,#13212,.F.);
#17029=ORIENTED_EDGE('',*,*,#13213,.T.);
#17030=ORIENTED_EDGE('',*,*,#13214,.T.);
#17031=ORIENTED_EDGE('',*,*,#13213,.F.);
#17032=ORIENTED_EDGE('',*,*,#13215,.T.);
#17033=ORIENTED_EDGE('',*,*,#13216,.F.);
#17034=ORIENTED_EDGE('',*,*,#13217,.F.);
#17035=ORIENTED_EDGE('',*,*,#13218,.T.);
#17036=ORIENTED_EDGE('',*,*,#13219,.T.);
#17037=ORIENTED_EDGE('',*,*,#13220,.F.);
#17038=ORIENTED_EDGE('',*,*,#13221,.F.);
#17039=ORIENTED_EDGE('',*,*,#13216,.T.);
#17040=ORIENTED_EDGE('',*,*,#13222,.T.);
#17041=ORIENTED_EDGE('',*,*,#13223,.F.);
#17042=ORIENTED_EDGE('',*,*,#13224,.F.);
#17043=ORIENTED_EDGE('',*,*,#13220,.T.);
#17044=ORIENTED_EDGE('',*,*,#13225,.T.);
#17045=ORIENTED_EDGE('',*,*,#13218,.F.);
#17046=ORIENTED_EDGE('',*,*,#13226,.F.);
#17047=ORIENTED_EDGE('',*,*,#13223,.T.);
#17048=ORIENTED_EDGE('',*,*,#13217,.T.);
#17049=ORIENTED_EDGE('',*,*,#13221,.T.);
#17050=ORIENTED_EDGE('',*,*,#13224,.T.);
#17051=ORIENTED_EDGE('',*,*,#13226,.T.);
#17052=ORIENTED_EDGE('',*,*,#13199,.F.);
#17053=ORIENTED_EDGE('',*,*,#13202,.F.);
#17054=ORIENTED_EDGE('',*,*,#13205,.F.);
#17055=ORIENTED_EDGE('',*,*,#13208,.F.);
#17056=ORIENTED_EDGE('',*,*,#13211,.F.);
#17057=ORIENTED_EDGE('',*,*,#13214,.F.);
#17058=ORIENTED_EDGE('',*,*,#13215,.F.);
#17059=ORIENTED_EDGE('',*,*,#13225,.F.);
#17060=ORIENTED_EDGE('',*,*,#13222,.F.);
#17061=ORIENTED_EDGE('',*,*,#13219,.F.);
#17062=ORIENTED_EDGE('',*,*,#13197,.T.);
#17063=ORIENTED_EDGE('',*,*,#13200,.T.);
#17064=ORIENTED_EDGE('',*,*,#13203,.T.);
#17065=ORIENTED_EDGE('',*,*,#13206,.T.);
#17066=ORIENTED_EDGE('',*,*,#13209,.T.);
#17067=ORIENTED_EDGE('',*,*,#13212,.T.);
#17068=ORIENTED_EDGE('',*,*,#13227,.F.);
#17069=ORIENTED_EDGE('',*,*,#13228,.T.);
#17070=ORIENTED_EDGE('',*,*,#13229,.T.);
#17071=ORIENTED_EDGE('',*,*,#13228,.F.);
#17072=ORIENTED_EDGE('',*,*,#13230,.F.);
#17073=ORIENTED_EDGE('',*,*,#13231,.F.);
#17074=ORIENTED_EDGE('',*,*,#13232,.F.);
#17075=ORIENTED_EDGE('',*,*,#13233,.F.);
#17076=ORIENTED_EDGE('',*,*,#13234,.F.);
#17077=ORIENTED_EDGE('',*,*,#13235,.T.);
#17078=ORIENTED_EDGE('',*,*,#13236,.T.);
#17079=ORIENTED_EDGE('',*,*,#13235,.F.);
#17080=ORIENTED_EDGE('',*,*,#13237,.F.);
#17081=ORIENTED_EDGE('',*,*,#13238,.F.);
#17082=ORIENTED_EDGE('',*,*,#13239,.F.);
#17083=ORIENTED_EDGE('',*,*,#13240,.F.);
#17084=ORIENTED_EDGE('',*,*,#13241,.F.);
#17085=ORIENTED_EDGE('',*,*,#13242,.T.);
#17086=ORIENTED_EDGE('',*,*,#13243,.T.);
#17087=ORIENTED_EDGE('',*,*,#13242,.F.);
#17088=ORIENTED_EDGE('',*,*,#13244,.F.);
#17089=ORIENTED_EDGE('',*,*,#13245,.F.);
#17090=ORIENTED_EDGE('',*,*,#13246,.F.);
#17091=ORIENTED_EDGE('',*,*,#13247,.F.);
#17092=ORIENTED_EDGE('',*,*,#13248,.F.);
#17093=ORIENTED_EDGE('',*,*,#13249,.T.);
#17094=ORIENTED_EDGE('',*,*,#13250,.T.);
#17095=ORIENTED_EDGE('',*,*,#13249,.F.);
#17096=ORIENTED_EDGE('',*,*,#13251,.F.);
#17097=ORIENTED_EDGE('',*,*,#13252,.F.);
#17098=ORIENTED_EDGE('',*,*,#13253,.F.);
#17099=ORIENTED_EDGE('',*,*,#13254,.F.);
#17100=ORIENTED_EDGE('',*,*,#13255,.F.);
#17101=ORIENTED_EDGE('',*,*,#13256,.T.);
#17102=ORIENTED_EDGE('',*,*,#13257,.T.);
#17103=ORIENTED_EDGE('',*,*,#13256,.F.);
#17104=ORIENTED_EDGE('',*,*,#13258,.F.);
#17105=ORIENTED_EDGE('',*,*,#13259,.F.);
#17106=ORIENTED_EDGE('',*,*,#13260,.F.);
#17107=ORIENTED_EDGE('',*,*,#13261,.F.);
#17108=ORIENTED_EDGE('',*,*,#13262,.F.);
#17109=ORIENTED_EDGE('',*,*,#13263,.T.);
#17110=ORIENTED_EDGE('',*,*,#13264,.T.);
#17111=ORIENTED_EDGE('',*,*,#13263,.F.);
#17112=ORIENTED_EDGE('',*,*,#13265,.F.);
#17113=ORIENTED_EDGE('',*,*,#13266,.F.);
#17114=ORIENTED_EDGE('',*,*,#13267,.F.);
#17115=ORIENTED_EDGE('',*,*,#13268,.F.);
#17116=ORIENTED_EDGE('',*,*,#13269,.F.);
#17117=ORIENTED_EDGE('',*,*,#13270,.T.);
#17118=ORIENTED_EDGE('',*,*,#13271,.T.);
#17119=ORIENTED_EDGE('',*,*,#13270,.F.);
#17120=ORIENTED_EDGE('',*,*,#13272,.F.);
#17121=ORIENTED_EDGE('',*,*,#13273,.F.);
#17122=ORIENTED_EDGE('',*,*,#13274,.F.);
#17123=ORIENTED_EDGE('',*,*,#13275,.F.);
#17124=ORIENTED_EDGE('',*,*,#13276,.F.);
#17125=ORIENTED_EDGE('',*,*,#13277,.T.);
#17126=ORIENTED_EDGE('',*,*,#13278,.T.);
#17127=ORIENTED_EDGE('',*,*,#13277,.F.);
#17128=ORIENTED_EDGE('',*,*,#13279,.F.);
#17129=ORIENTED_EDGE('',*,*,#13280,.F.);
#17130=ORIENTED_EDGE('',*,*,#13281,.F.);
#17131=ORIENTED_EDGE('',*,*,#13282,.F.);
#17132=ORIENTED_EDGE('',*,*,#13283,.F.);
#17133=ORIENTED_EDGE('',*,*,#13284,.T.);
#17134=ORIENTED_EDGE('',*,*,#13285,.T.);
#17135=ORIENTED_EDGE('',*,*,#13284,.F.);
#17136=ORIENTED_EDGE('',*,*,#13286,.F.);
#17137=ORIENTED_EDGE('',*,*,#13287,.F.);
#17138=ORIENTED_EDGE('',*,*,#13288,.F.);
#17139=ORIENTED_EDGE('',*,*,#13289,.F.);
#17140=ORIENTED_EDGE('',*,*,#13290,.F.);
#17141=ORIENTED_EDGE('',*,*,#13291,.T.);
#17142=ORIENTED_EDGE('',*,*,#13292,.T.);
#17143=ORIENTED_EDGE('',*,*,#13291,.F.);
#17144=ORIENTED_EDGE('',*,*,#13293,.F.);
#17145=ORIENTED_EDGE('',*,*,#13294,.F.);
#17146=ORIENTED_EDGE('',*,*,#13295,.F.);
#17147=ORIENTED_EDGE('',*,*,#13296,.F.);
#17148=ORIENTED_EDGE('',*,*,#13297,.F.);
#17149=ORIENTED_EDGE('',*,*,#13298,.T.);
#17150=ORIENTED_EDGE('',*,*,#13299,.T.);
#17151=ORIENTED_EDGE('',*,*,#13298,.F.);
#17152=ORIENTED_EDGE('',*,*,#13300,.F.);
#17153=ORIENTED_EDGE('',*,*,#13301,.F.);
#17154=ORIENTED_EDGE('',*,*,#13302,.F.);
#17155=ORIENTED_EDGE('',*,*,#13303,.F.);
#17156=ORIENTED_EDGE('',*,*,#13304,.F.);
#17157=ORIENTED_EDGE('',*,*,#13305,.T.);
#17158=ORIENTED_EDGE('',*,*,#13306,.T.);
#17159=ORIENTED_EDGE('',*,*,#13305,.F.);
#17160=ORIENTED_EDGE('',*,*,#13307,.F.);
#17161=ORIENTED_EDGE('',*,*,#13308,.F.);
#17162=ORIENTED_EDGE('',*,*,#13309,.F.);
#17163=ORIENTED_EDGE('',*,*,#13310,.F.);
#17164=ORIENTED_EDGE('',*,*,#13311,.F.);
#17165=ORIENTED_EDGE('',*,*,#13312,.T.);
#17166=ORIENTED_EDGE('',*,*,#13313,.T.);
#17167=ORIENTED_EDGE('',*,*,#13312,.F.);
#17168=ORIENTED_EDGE('',*,*,#13314,.F.);
#17169=ORIENTED_EDGE('',*,*,#13315,.F.);
#17170=ORIENTED_EDGE('',*,*,#13316,.F.);
#17171=ORIENTED_EDGE('',*,*,#13317,.F.);
#17172=ORIENTED_EDGE('',*,*,#13318,.F.);
#17173=ORIENTED_EDGE('',*,*,#13319,.T.);
#17174=ORIENTED_EDGE('',*,*,#13320,.T.);
#17175=ORIENTED_EDGE('',*,*,#13319,.F.);
#17176=ORIENTED_EDGE('',*,*,#13321,.F.);
#17177=ORIENTED_EDGE('',*,*,#13322,.F.);
#17178=ORIENTED_EDGE('',*,*,#13323,.F.);
#17179=ORIENTED_EDGE('',*,*,#13324,.F.);
#17180=ORIENTED_EDGE('',*,*,#13325,.F.);
#17181=ORIENTED_EDGE('',*,*,#13326,.T.);
#17182=ORIENTED_EDGE('',*,*,#13327,.T.);
#17183=ORIENTED_EDGE('',*,*,#13326,.F.);
#17184=ORIENTED_EDGE('',*,*,#13328,.F.);
#17185=ORIENTED_EDGE('',*,*,#13329,.F.);
#17186=ORIENTED_EDGE('',*,*,#13330,.F.);
#17187=ORIENTED_EDGE('',*,*,#13331,.F.);
#17188=ORIENTED_EDGE('',*,*,#13332,.F.);
#17189=ORIENTED_EDGE('',*,*,#13333,.T.);
#17190=ORIENTED_EDGE('',*,*,#13334,.T.);
#17191=ORIENTED_EDGE('',*,*,#13333,.F.);
#17192=ORIENTED_EDGE('',*,*,#13335,.F.);
#17193=ORIENTED_EDGE('',*,*,#13336,.F.);
#17194=ORIENTED_EDGE('',*,*,#13337,.F.);
#17195=ORIENTED_EDGE('',*,*,#13338,.F.);
#17196=ORIENTED_EDGE('',*,*,#13339,.F.);
#17197=ORIENTED_EDGE('',*,*,#13340,.T.);
#17198=ORIENTED_EDGE('',*,*,#13341,.T.);
#17199=ORIENTED_EDGE('',*,*,#13340,.F.);
#17200=ORIENTED_EDGE('',*,*,#13342,.F.);
#17201=ORIENTED_EDGE('',*,*,#13343,.F.);
#17202=ORIENTED_EDGE('',*,*,#13344,.F.);
#17203=ORIENTED_EDGE('',*,*,#13345,.F.);
#17204=ORIENTED_EDGE('',*,*,#13346,.F.);
#17205=ORIENTED_EDGE('',*,*,#13347,.T.);
#17206=ORIENTED_EDGE('',*,*,#13348,.T.);
#17207=ORIENTED_EDGE('',*,*,#13347,.F.);
#17208=ORIENTED_EDGE('',*,*,#13349,.F.);
#17209=ORIENTED_EDGE('',*,*,#13350,.F.);
#17210=ORIENTED_EDGE('',*,*,#13351,.F.);
#17211=ORIENTED_EDGE('',*,*,#13352,.F.);
#17212=ORIENTED_EDGE('',*,*,#13353,.F.);
#17213=ORIENTED_EDGE('',*,*,#13354,.T.);
#17214=ORIENTED_EDGE('',*,*,#13355,.T.);
#17215=ORIENTED_EDGE('',*,*,#13354,.F.);
#17216=ORIENTED_EDGE('',*,*,#13356,.F.);
#17217=ORIENTED_EDGE('',*,*,#13357,.F.);
#17218=ORIENTED_EDGE('',*,*,#13358,.F.);
#17219=ORIENTED_EDGE('',*,*,#13359,.F.);
#17220=ORIENTED_EDGE('',*,*,#13360,.F.);
#17221=ORIENTED_EDGE('',*,*,#13361,.T.);
#17222=ORIENTED_EDGE('',*,*,#13362,.T.);
#17223=ORIENTED_EDGE('',*,*,#13361,.F.);
#17224=ORIENTED_EDGE('',*,*,#13363,.F.);
#17225=ORIENTED_EDGE('',*,*,#13364,.F.);
#17226=ORIENTED_EDGE('',*,*,#13365,.F.);
#17227=ORIENTED_EDGE('',*,*,#13366,.F.);
#17228=ORIENTED_EDGE('',*,*,#13367,.F.);
#17229=ORIENTED_EDGE('',*,*,#13368,.T.);
#17230=ORIENTED_EDGE('',*,*,#13369,.T.);
#17231=ORIENTED_EDGE('',*,*,#13368,.F.);
#17232=ORIENTED_EDGE('',*,*,#13370,.F.);
#17233=ORIENTED_EDGE('',*,*,#13371,.F.);
#17234=ORIENTED_EDGE('',*,*,#13372,.F.);
#17235=ORIENTED_EDGE('',*,*,#13373,.F.);
#17236=ORIENTED_EDGE('',*,*,#13374,.F.);
#17237=ORIENTED_EDGE('',*,*,#13375,.T.);
#17238=ORIENTED_EDGE('',*,*,#13376,.T.);
#17239=ORIENTED_EDGE('',*,*,#13375,.F.);
#17240=ORIENTED_EDGE('',*,*,#13377,.F.);
#17241=ORIENTED_EDGE('',*,*,#13378,.F.);
#17242=ORIENTED_EDGE('',*,*,#13379,.F.);
#17243=ORIENTED_EDGE('',*,*,#13380,.F.);
#17244=ORIENTED_EDGE('',*,*,#13381,.F.);
#17245=ORIENTED_EDGE('',*,*,#13382,.T.);
#17246=ORIENTED_EDGE('',*,*,#13383,.T.);
#17247=ORIENTED_EDGE('',*,*,#13382,.F.);
#17248=ORIENTED_EDGE('',*,*,#13384,.F.);
#17249=ORIENTED_EDGE('',*,*,#13385,.F.);
#17250=ORIENTED_EDGE('',*,*,#13386,.F.);
#17251=ORIENTED_EDGE('',*,*,#13387,.F.);
#17252=ORIENTED_EDGE('',*,*,#13388,.F.);
#17253=ORIENTED_EDGE('',*,*,#13389,.T.);
#17254=ORIENTED_EDGE('',*,*,#13390,.T.);
#17255=ORIENTED_EDGE('',*,*,#13389,.F.);
#17256=ORIENTED_EDGE('',*,*,#13391,.F.);
#17257=ORIENTED_EDGE('',*,*,#13392,.F.);
#17258=ORIENTED_EDGE('',*,*,#13393,.F.);
#17259=ORIENTED_EDGE('',*,*,#13394,.F.);
#17260=ORIENTED_EDGE('',*,*,#13395,.F.);
#17261=ORIENTED_EDGE('',*,*,#13396,.T.);
#17262=ORIENTED_EDGE('',*,*,#13397,.T.);
#17263=ORIENTED_EDGE('',*,*,#13396,.F.);
#17264=ORIENTED_EDGE('',*,*,#13398,.F.);
#17265=ORIENTED_EDGE('',*,*,#13399,.F.);
#17266=ORIENTED_EDGE('',*,*,#13400,.F.);
#17267=ORIENTED_EDGE('',*,*,#13401,.F.);
#17268=ORIENTED_EDGE('',*,*,#13402,.F.);
#17269=ORIENTED_EDGE('',*,*,#13403,.T.);
#17270=ORIENTED_EDGE('',*,*,#13404,.T.);
#17271=ORIENTED_EDGE('',*,*,#13403,.F.);
#17272=ORIENTED_EDGE('',*,*,#13405,.F.);
#17273=ORIENTED_EDGE('',*,*,#13406,.F.);
#17274=ORIENTED_EDGE('',*,*,#13407,.F.);
#17275=ORIENTED_EDGE('',*,*,#13408,.F.);
#17276=ORIENTED_EDGE('',*,*,#13409,.F.);
#17277=ORIENTED_EDGE('',*,*,#13410,.T.);
#17278=ORIENTED_EDGE('',*,*,#13411,.T.);
#17279=ORIENTED_EDGE('',*,*,#13410,.F.);
#17280=ORIENTED_EDGE('',*,*,#13412,.F.);
#17281=ORIENTED_EDGE('',*,*,#13413,.F.);
#17282=ORIENTED_EDGE('',*,*,#13414,.F.);
#17283=ORIENTED_EDGE('',*,*,#13415,.F.);
#17284=ORIENTED_EDGE('',*,*,#13416,.F.);
#17285=ORIENTED_EDGE('',*,*,#13417,.T.);
#17286=ORIENTED_EDGE('',*,*,#13418,.T.);
#17287=ORIENTED_EDGE('',*,*,#13417,.F.);
#17288=ORIENTED_EDGE('',*,*,#13419,.F.);
#17289=ORIENTED_EDGE('',*,*,#13420,.F.);
#17290=ORIENTED_EDGE('',*,*,#13421,.F.);
#17291=ORIENTED_EDGE('',*,*,#13422,.F.);
#17292=ORIENTED_EDGE('',*,*,#13423,.F.);
#17293=ORIENTED_EDGE('',*,*,#13424,.T.);
#17294=ORIENTED_EDGE('',*,*,#13425,.T.);
#17295=ORIENTED_EDGE('',*,*,#13424,.F.);
#17296=ORIENTED_EDGE('',*,*,#13426,.F.);
#17297=ORIENTED_EDGE('',*,*,#13427,.F.);
#17298=ORIENTED_EDGE('',*,*,#13428,.F.);
#17299=ORIENTED_EDGE('',*,*,#13429,.F.);
#17300=ORIENTED_EDGE('',*,*,#13430,.F.);
#17301=ORIENTED_EDGE('',*,*,#13431,.T.);
#17302=ORIENTED_EDGE('',*,*,#13432,.T.);
#17303=ORIENTED_EDGE('',*,*,#13431,.F.);
#17304=ORIENTED_EDGE('',*,*,#13433,.F.);
#17305=ORIENTED_EDGE('',*,*,#13434,.F.);
#17306=ORIENTED_EDGE('',*,*,#13435,.F.);
#17307=ORIENTED_EDGE('',*,*,#13436,.F.);
#17308=ORIENTED_EDGE('',*,*,#13437,.T.);
#17309=ORIENTED_EDGE('',*,*,#13233,.T.);
#17310=ORIENTED_EDGE('',*,*,#13438,.F.);
#17311=ORIENTED_EDGE('',*,*,#13439,.F.);
#17312=ORIENTED_EDGE('',*,*,#13440,.F.);
#17313=ORIENTED_EDGE('',*,*,#13240,.T.);
#17314=ORIENTED_EDGE('',*,*,#13441,.T.);
#17315=ORIENTED_EDGE('',*,*,#13252,.T.);
#17316=ORIENTED_EDGE('',*,*,#13438,.T.);
#17317=ORIENTED_EDGE('',*,*,#13232,.T.);
#17318=ORIENTED_EDGE('',*,*,#13442,.T.);
#17319=ORIENTED_EDGE('',*,*,#13246,.T.);
#17320=ORIENTED_EDGE('',*,*,#13443,.T.);
#17321=ORIENTED_EDGE('',*,*,#13260,.T.);
#17322=ORIENTED_EDGE('',*,*,#13444,.T.);
#17323=ORIENTED_EDGE('',*,*,#13274,.T.);
#17324=ORIENTED_EDGE('',*,*,#13445,.T.);
#17325=ORIENTED_EDGE('',*,*,#13288,.T.);
#17326=ORIENTED_EDGE('',*,*,#13446,.T.);
#17327=ORIENTED_EDGE('',*,*,#13302,.T.);
#17328=ORIENTED_EDGE('',*,*,#13447,.T.);
#17329=ORIENTED_EDGE('',*,*,#13316,.T.);
#17330=ORIENTED_EDGE('',*,*,#13448,.T.);
#17331=ORIENTED_EDGE('',*,*,#13330,.T.);
#17332=ORIENTED_EDGE('',*,*,#13449,.T.);
#17333=ORIENTED_EDGE('',*,*,#13344,.T.);
#17334=ORIENTED_EDGE('',*,*,#13450,.T.);
#17335=ORIENTED_EDGE('',*,*,#13358,.T.);
#17336=ORIENTED_EDGE('',*,*,#13451,.T.);
#17337=ORIENTED_EDGE('',*,*,#13372,.T.);
#17338=ORIENTED_EDGE('',*,*,#13452,.T.);
#17339=ORIENTED_EDGE('',*,*,#13386,.T.);
#17340=ORIENTED_EDGE('',*,*,#13453,.T.);
#17341=ORIENTED_EDGE('',*,*,#13400,.T.);
#17342=ORIENTED_EDGE('',*,*,#13454,.T.);
#17343=ORIENTED_EDGE('',*,*,#13414,.T.);
#17344=ORIENTED_EDGE('',*,*,#13455,.T.);
#17345=ORIENTED_EDGE('',*,*,#13428,.T.);
#17346=ORIENTED_EDGE('',*,*,#13456,.T.);
#17347=ORIENTED_EDGE('',*,*,#13457,.F.);
#17348=ORIENTED_EDGE('',*,*,#13458,.F.);
#17349=ORIENTED_EDGE('',*,*,#13459,.T.);
#17350=ORIENTED_EDGE('',*,*,#13460,.F.);
#17351=ORIENTED_EDGE('',*,*,#13230,.T.);
#17352=ORIENTED_EDGE('',*,*,#13440,.T.);
#17353=ORIENTED_EDGE('',*,*,#13251,.T.);
#17354=ORIENTED_EDGE('',*,*,#13248,.T.);
#17355=ORIENTED_EDGE('',*,*,#13441,.F.);
#17356=ORIENTED_EDGE('',*,*,#13239,.T.);
#17357=ORIENTED_EDGE('',*,*,#13461,.F.);
#17358=ORIENTED_EDGE('',*,*,#13462,.T.);
#17359=ORIENTED_EDGE('',*,*,#13463,.T.);
#17360=ORIENTED_EDGE('',*,*,#13464,.F.);
#17361=ORIENTED_EDGE('',*,*,#13465,.F.);
#17362=ORIENTED_EDGE('',*,*,#13435,.T.);
#17363=ORIENTED_EDGE('',*,*,#13466,.F.);
#17364=ORIENTED_EDGE('',*,*,#13421,.T.);
#17365=ORIENTED_EDGE('',*,*,#13467,.F.);
#17366=ORIENTED_EDGE('',*,*,#13407,.T.);
#17367=ORIENTED_EDGE('',*,*,#13468,.F.);
#17368=ORIENTED_EDGE('',*,*,#13393,.T.);
#17369=ORIENTED_EDGE('',*,*,#13469,.F.);
#17370=ORIENTED_EDGE('',*,*,#13379,.T.);
#17371=ORIENTED_EDGE('',*,*,#13470,.F.);
#17372=ORIENTED_EDGE('',*,*,#13365,.T.);
#17373=ORIENTED_EDGE('',*,*,#13471,.F.);
#17374=ORIENTED_EDGE('',*,*,#13351,.T.);
#17375=ORIENTED_EDGE('',*,*,#13472,.F.);
#17376=ORIENTED_EDGE('',*,*,#13337,.T.);
#17377=ORIENTED_EDGE('',*,*,#13473,.F.);
#17378=ORIENTED_EDGE('',*,*,#13323,.T.);
#17379=ORIENTED_EDGE('',*,*,#13474,.F.);
#17380=ORIENTED_EDGE('',*,*,#13309,.T.);
#17381=ORIENTED_EDGE('',*,*,#13475,.F.);
#17382=ORIENTED_EDGE('',*,*,#13295,.T.);
#17383=ORIENTED_EDGE('',*,*,#13476,.F.);
#17384=ORIENTED_EDGE('',*,*,#13281,.T.);
#17385=ORIENTED_EDGE('',*,*,#13477,.F.);
#17386=ORIENTED_EDGE('',*,*,#13267,.T.);
#17387=ORIENTED_EDGE('',*,*,#13478,.F.);
#17388=ORIENTED_EDGE('',*,*,#13253,.T.);
#17389=ORIENTED_EDGE('',*,*,#13442,.F.);
#17390=ORIENTED_EDGE('',*,*,#13231,.T.);
#17391=ORIENTED_EDGE('',*,*,#13460,.T.);
#17392=ORIENTED_EDGE('',*,*,#13247,.T.);
#17393=ORIENTED_EDGE('',*,*,#13479,.F.);
#17394=ORIENTED_EDGE('',*,*,#13244,.T.);
#17395=ORIENTED_EDGE('',*,*,#13480,.T.);
#17396=ORIENTED_EDGE('',*,*,#13265,.T.);
#17397=ORIENTED_EDGE('',*,*,#13262,.T.);
#17398=ORIENTED_EDGE('',*,*,#13480,.F.);
#17399=ORIENTED_EDGE('',*,*,#13254,.T.);
#17400=ORIENTED_EDGE('',*,*,#13478,.T.);
#17401=ORIENTED_EDGE('',*,*,#13266,.T.);
#17402=ORIENTED_EDGE('',*,*,#13443,.F.);
#17403=ORIENTED_EDGE('',*,*,#13245,.T.);
#17404=ORIENTED_EDGE('',*,*,#13479,.T.);
#17405=ORIENTED_EDGE('',*,*,#13261,.T.);
#17406=ORIENTED_EDGE('',*,*,#13481,.F.);
#17407=ORIENTED_EDGE('',*,*,#13258,.T.);
#17408=ORIENTED_EDGE('',*,*,#13482,.T.);
#17409=ORIENTED_EDGE('',*,*,#13279,.T.);
#17410=ORIENTED_EDGE('',*,*,#13276,.T.);
#17411=ORIENTED_EDGE('',*,*,#13482,.F.);
#17412=ORIENTED_EDGE('',*,*,#13268,.T.);
#17413=ORIENTED_EDGE('',*,*,#13477,.T.);
#17414=ORIENTED_EDGE('',*,*,#13280,.T.);
#17415=ORIENTED_EDGE('',*,*,#13444,.F.);
#17416=ORIENTED_EDGE('',*,*,#13259,.T.);
#17417=ORIENTED_EDGE('',*,*,#13481,.T.);
#17418=ORIENTED_EDGE('',*,*,#13275,.T.);
#17419=ORIENTED_EDGE('',*,*,#13483,.F.);
#17420=ORIENTED_EDGE('',*,*,#13272,.T.);
#17421=ORIENTED_EDGE('',*,*,#13484,.T.);
#17422=ORIENTED_EDGE('',*,*,#13293,.T.);
#17423=ORIENTED_EDGE('',*,*,#13290,.T.);
#17424=ORIENTED_EDGE('',*,*,#13484,.F.);
#17425=ORIENTED_EDGE('',*,*,#13282,.T.);
#17426=ORIENTED_EDGE('',*,*,#13476,.T.);
#17427=ORIENTED_EDGE('',*,*,#13294,.T.);
#17428=ORIENTED_EDGE('',*,*,#13445,.F.);
#17429=ORIENTED_EDGE('',*,*,#13273,.T.);
#17430=ORIENTED_EDGE('',*,*,#13483,.T.);
#17431=ORIENTED_EDGE('',*,*,#13289,.T.);
#17432=ORIENTED_EDGE('',*,*,#13485,.F.);
#17433=ORIENTED_EDGE('',*,*,#13286,.T.);
#17434=ORIENTED_EDGE('',*,*,#13486,.T.);
#17435=ORIENTED_EDGE('',*,*,#13307,.T.);
#17436=ORIENTED_EDGE('',*,*,#13304,.T.);
#17437=ORIENTED_EDGE('',*,*,#13486,.F.);
#17438=ORIENTED_EDGE('',*,*,#13296,.T.);
#17439=ORIENTED_EDGE('',*,*,#13475,.T.);
#17440=ORIENTED_EDGE('',*,*,#13308,.T.);
#17441=ORIENTED_EDGE('',*,*,#13446,.F.);
#17442=ORIENTED_EDGE('',*,*,#13287,.T.);
#17443=ORIENTED_EDGE('',*,*,#13485,.T.);
#17444=ORIENTED_EDGE('',*,*,#13303,.T.);
#17445=ORIENTED_EDGE('',*,*,#13487,.F.);
#17446=ORIENTED_EDGE('',*,*,#13300,.T.);
#17447=ORIENTED_EDGE('',*,*,#13488,.T.);
#17448=ORIENTED_EDGE('',*,*,#13321,.T.);
#17449=ORIENTED_EDGE('',*,*,#13318,.T.);
#17450=ORIENTED_EDGE('',*,*,#13488,.F.);
#17451=ORIENTED_EDGE('',*,*,#13310,.T.);
#17452=ORIENTED_EDGE('',*,*,#13474,.T.);
#17453=ORIENTED_EDGE('',*,*,#13322,.T.);
#17454=ORIENTED_EDGE('',*,*,#13447,.F.);
#17455=ORIENTED_EDGE('',*,*,#13301,.T.);
#17456=ORIENTED_EDGE('',*,*,#13487,.T.);
#17457=ORIENTED_EDGE('',*,*,#13317,.T.);
#17458=ORIENTED_EDGE('',*,*,#13489,.F.);
#17459=ORIENTED_EDGE('',*,*,#13314,.T.);
#17460=ORIENTED_EDGE('',*,*,#13490,.T.);
#17461=ORIENTED_EDGE('',*,*,#13335,.T.);
#17462=ORIENTED_EDGE('',*,*,#13332,.T.);
#17463=ORIENTED_EDGE('',*,*,#13490,.F.);
#17464=ORIENTED_EDGE('',*,*,#13324,.T.);
#17465=ORIENTED_EDGE('',*,*,#13473,.T.);
#17466=ORIENTED_EDGE('',*,*,#13336,.T.);
#17467=ORIENTED_EDGE('',*,*,#13448,.F.);
#17468=ORIENTED_EDGE('',*,*,#13315,.T.);
#17469=ORIENTED_EDGE('',*,*,#13489,.T.);
#17470=ORIENTED_EDGE('',*,*,#13331,.T.);
#17471=ORIENTED_EDGE('',*,*,#13491,.F.);
#17472=ORIENTED_EDGE('',*,*,#13328,.T.);
#17473=ORIENTED_EDGE('',*,*,#13492,.T.);
#17474=ORIENTED_EDGE('',*,*,#13349,.T.);
#17475=ORIENTED_EDGE('',*,*,#13346,.T.);
#17476=ORIENTED_EDGE('',*,*,#13492,.F.);
#17477=ORIENTED_EDGE('',*,*,#13338,.T.);
#17478=ORIENTED_EDGE('',*,*,#13472,.T.);
#17479=ORIENTED_EDGE('',*,*,#13350,.T.);
#17480=ORIENTED_EDGE('',*,*,#13449,.F.);
#17481=ORIENTED_EDGE('',*,*,#13329,.T.);
#17482=ORIENTED_EDGE('',*,*,#13491,.T.);
#17483=ORIENTED_EDGE('',*,*,#13345,.T.);
#17484=ORIENTED_EDGE('',*,*,#13493,.F.);
#17485=ORIENTED_EDGE('',*,*,#13342,.T.);
#17486=ORIENTED_EDGE('',*,*,#13494,.T.);
#17487=ORIENTED_EDGE('',*,*,#13363,.T.);
#17488=ORIENTED_EDGE('',*,*,#13360,.T.);
#17489=ORIENTED_EDGE('',*,*,#13494,.F.);
#17490=ORIENTED_EDGE('',*,*,#13352,.T.);
#17491=ORIENTED_EDGE('',*,*,#13471,.T.);
#17492=ORIENTED_EDGE('',*,*,#13364,.T.);
#17493=ORIENTED_EDGE('',*,*,#13450,.F.);
#17494=ORIENTED_EDGE('',*,*,#13343,.T.);
#17495=ORIENTED_EDGE('',*,*,#13493,.T.);
#17496=ORIENTED_EDGE('',*,*,#13359,.T.);
#17497=ORIENTED_EDGE('',*,*,#13495,.F.);
#17498=ORIENTED_EDGE('',*,*,#13356,.T.);
#17499=ORIENTED_EDGE('',*,*,#13496,.T.);
#17500=ORIENTED_EDGE('',*,*,#13377,.T.);
#17501=ORIENTED_EDGE('',*,*,#13374,.T.);
#17502=ORIENTED_EDGE('',*,*,#13496,.F.);
#17503=ORIENTED_EDGE('',*,*,#13366,.T.);
#17504=ORIENTED_EDGE('',*,*,#13470,.T.);
#17505=ORIENTED_EDGE('',*,*,#13378,.T.);
#17506=ORIENTED_EDGE('',*,*,#13497,.F.);
#17507=ORIENTED_EDGE('',*,*,#13370,.T.);
#17508=ORIENTED_EDGE('',*,*,#13498,.T.);
#17509=ORIENTED_EDGE('',*,*,#13391,.T.);
#17510=ORIENTED_EDGE('',*,*,#13388,.T.);
#17511=ORIENTED_EDGE('',*,*,#13451,.F.);
#17512=ORIENTED_EDGE('',*,*,#13357,.T.);
#17513=ORIENTED_EDGE('',*,*,#13495,.T.);
#17514=ORIENTED_EDGE('',*,*,#13373,.T.);
#17515=ORIENTED_EDGE('',*,*,#13498,.F.);
#17516=ORIENTED_EDGE('',*,*,#13380,.T.);
#17517=ORIENTED_EDGE('',*,*,#13469,.T.);
#17518=ORIENTED_EDGE('',*,*,#13392,.T.);
#17519=ORIENTED_EDGE('',*,*,#13452,.F.);
#17520=ORIENTED_EDGE('',*,*,#13371,.T.);
#17521=ORIENTED_EDGE('',*,*,#13497,.T.);
#17522=ORIENTED_EDGE('',*,*,#13387,.T.);
#17523=ORIENTED_EDGE('',*,*,#13499,.F.);
#17524=ORIENTED_EDGE('',*,*,#13384,.T.);
#17525=ORIENTED_EDGE('',*,*,#13500,.T.);
#17526=ORIENTED_EDGE('',*,*,#13405,.T.);
#17527=ORIENTED_EDGE('',*,*,#13402,.T.);
#17528=ORIENTED_EDGE('',*,*,#13500,.F.);
#17529=ORIENTED_EDGE('',*,*,#13394,.T.);
#17530=ORIENTED_EDGE('',*,*,#13468,.T.);
#17531=ORIENTED_EDGE('',*,*,#13406,.T.);
#17532=ORIENTED_EDGE('',*,*,#13453,.F.);
#17533=ORIENTED_EDGE('',*,*,#13385,.T.);
#17534=ORIENTED_EDGE('',*,*,#13499,.T.);
#17535=ORIENTED_EDGE('',*,*,#13401,.T.);
#17536=ORIENTED_EDGE('',*,*,#13501,.F.);
#17537=ORIENTED_EDGE('',*,*,#13398,.T.);
#17538=ORIENTED_EDGE('',*,*,#13502,.T.);
#17539=ORIENTED_EDGE('',*,*,#13419,.T.);
#17540=ORIENTED_EDGE('',*,*,#13416,.T.);
#17541=ORIENTED_EDGE('',*,*,#13502,.F.);
#17542=ORIENTED_EDGE('',*,*,#13408,.T.);
#17543=ORIENTED_EDGE('',*,*,#13467,.T.);
#17544=ORIENTED_EDGE('',*,*,#13420,.T.);
#17545=ORIENTED_EDGE('',*,*,#13503,.F.);
#17546=ORIENTED_EDGE('',*,*,#13412,.T.);
#17547=ORIENTED_EDGE('',*,*,#13504,.T.);
#17548=ORIENTED_EDGE('',*,*,#13433,.T.);
#17549=ORIENTED_EDGE('',*,*,#13430,.T.);
#17550=ORIENTED_EDGE('',*,*,#13454,.F.);
#17551=ORIENTED_EDGE('',*,*,#13399,.T.);
#17552=ORIENTED_EDGE('',*,*,#13501,.T.);
#17553=ORIENTED_EDGE('',*,*,#13415,.T.);
#17554=ORIENTED_EDGE('',*,*,#13504,.F.);
#17555=ORIENTED_EDGE('',*,*,#13422,.T.);
#17556=ORIENTED_EDGE('',*,*,#13466,.T.);
#17557=ORIENTED_EDGE('',*,*,#13434,.T.);
#17558=ORIENTED_EDGE('',*,*,#13505,.F.);
#17559=ORIENTED_EDGE('',*,*,#13426,.T.);
#17560=ORIENTED_EDGE('',*,*,#13506,.T.);
#17561=ORIENTED_EDGE('',*,*,#13507,.T.);
#17562=ORIENTED_EDGE('',*,*,#13455,.F.);
#17563=ORIENTED_EDGE('',*,*,#13413,.T.);
#17564=ORIENTED_EDGE('',*,*,#13503,.T.);
#17565=ORIENTED_EDGE('',*,*,#13429,.T.);
#17566=ORIENTED_EDGE('',*,*,#13506,.F.);
#17567=ORIENTED_EDGE('',*,*,#13436,.T.);
#17568=ORIENTED_EDGE('',*,*,#13465,.T.);
#17569=ORIENTED_EDGE('',*,*,#13508,.T.);
#17570=ORIENTED_EDGE('',*,*,#13439,.T.);
#17571=ORIENTED_EDGE('',*,*,#13459,.F.);
#17572=ORIENTED_EDGE('',*,*,#13509,.F.);
#17573=ORIENTED_EDGE('',*,*,#13510,.F.);
#17574=ORIENTED_EDGE('',*,*,#13511,.T.);
#17575=ORIENTED_EDGE('',*,*,#13512,.F.);
#17576=ORIENTED_EDGE('',*,*,#13513,.T.);
#17577=ORIENTED_EDGE('',*,*,#13514,.F.);
#17578=ORIENTED_EDGE('',*,*,#13515,.T.);
#17579=ORIENTED_EDGE('',*,*,#13516,.F.);
#17580=ORIENTED_EDGE('',*,*,#13517,.T.);
#17581=ORIENTED_EDGE('',*,*,#13518,.T.);
#17582=ORIENTED_EDGE('',*,*,#13519,.T.);
#17583=ORIENTED_EDGE('',*,*,#13520,.F.);
#17584=ORIENTED_EDGE('',*,*,#13521,.T.);
#17585=ORIENTED_EDGE('',*,*,#13522,.F.);
#17586=ORIENTED_EDGE('',*,*,#13523,.T.);
#17587=ORIENTED_EDGE('',*,*,#13524,.F.);
#17588=ORIENTED_EDGE('',*,*,#13525,.T.);
#17589=ORIENTED_EDGE('',*,*,#13526,.T.);
#17590=ORIENTED_EDGE('',*,*,#13527,.T.);
#17591=ORIENTED_EDGE('',*,*,#13528,.F.);
#17592=ORIENTED_EDGE('',*,*,#13529,.F.);
#17593=ORIENTED_EDGE('',*,*,#13530,.T.);
#17594=ORIENTED_EDGE('',*,*,#13531,.T.);
#17595=ORIENTED_EDGE('',*,*,#13532,.F.);
#17596=ORIENTED_EDGE('',*,*,#13533,.T.);
#17597=ORIENTED_EDGE('',*,*,#13534,.T.);
#17598=ORIENTED_EDGE('',*,*,#13535,.T.);
#17599=ORIENTED_EDGE('',*,*,#13536,.T.);
#17600=ORIENTED_EDGE('',*,*,#13537,.T.);
#17601=ORIENTED_EDGE('',*,*,#13538,.T.);
#17602=ORIENTED_EDGE('',*,*,#13539,.T.);
#17603=ORIENTED_EDGE('',*,*,#13540,.F.);
#17604=ORIENTED_EDGE('',*,*,#13541,.T.);
#17605=ORIENTED_EDGE('',*,*,#13542,.T.);
#17606=ORIENTED_EDGE('',*,*,#13543,.T.);
#17607=ORIENTED_EDGE('',*,*,#13544,.T.);
#17608=ORIENTED_EDGE('',*,*,#13545,.T.);
#17609=ORIENTED_EDGE('',*,*,#13546,.T.);
#17610=ORIENTED_EDGE('',*,*,#13547,.T.);
#17611=ORIENTED_EDGE('',*,*,#13548,.T.);
#17612=ORIENTED_EDGE('',*,*,#13549,.T.);
#17613=ORIENTED_EDGE('',*,*,#13462,.F.);
#17614=ORIENTED_EDGE('',*,*,#13550,.T.);
#17615=ORIENTED_EDGE('',*,*,#13551,.T.);
#17616=ORIENTED_EDGE('',*,*,#13457,.T.);
#17617=ORIENTED_EDGE('',*,*,#13552,.F.);
#17618=ORIENTED_EDGE('',*,*,#13507,.F.);
#17619=ORIENTED_EDGE('',*,*,#13508,.F.);
#17620=ORIENTED_EDGE('',*,*,#13464,.T.);
#17621=ORIENTED_EDGE('',*,*,#13553,.F.);
#17622=ORIENTED_EDGE('',*,*,#13554,.F.);
#17623=ORIENTED_EDGE('',*,*,#13555,.T.);
#17624=ORIENTED_EDGE('',*,*,#13556,.F.);
#17625=ORIENTED_EDGE('',*,*,#13557,.T.);
#17626=ORIENTED_EDGE('',*,*,#13558,.F.);
#17627=ORIENTED_EDGE('',*,*,#13559,.T.);
#17628=ORIENTED_EDGE('',*,*,#13560,.F.);
#17629=ORIENTED_EDGE('',*,*,#13561,.T.);
#17630=ORIENTED_EDGE('',*,*,#13562,.T.);
#17631=ORIENTED_EDGE('',*,*,#13563,.T.);
#17632=ORIENTED_EDGE('',*,*,#13564,.F.);
#17633=ORIENTED_EDGE('',*,*,#13565,.T.);
#17634=ORIENTED_EDGE('',*,*,#13566,.F.);
#17635=ORIENTED_EDGE('',*,*,#13567,.T.);
#17636=ORIENTED_EDGE('',*,*,#13568,.F.);
#17637=ORIENTED_EDGE('',*,*,#13569,.T.);
#17638=ORIENTED_EDGE('',*,*,#13570,.T.);
#17639=ORIENTED_EDGE('',*,*,#13571,.T.);
#17640=ORIENTED_EDGE('',*,*,#13572,.F.);
#17641=ORIENTED_EDGE('',*,*,#13573,.T.);
#17642=ORIENTED_EDGE('',*,*,#13574,.T.);
#17643=ORIENTED_EDGE('',*,*,#13575,.T.);
#17644=ORIENTED_EDGE('',*,*,#13576,.F.);
#17645=ORIENTED_EDGE('',*,*,#13577,.T.);
#17646=ORIENTED_EDGE('',*,*,#13578,.T.);
#17647=ORIENTED_EDGE('',*,*,#13579,.T.);
#17648=ORIENTED_EDGE('',*,*,#13580,.T.);
#17649=ORIENTED_EDGE('',*,*,#13581,.T.);
#17650=ORIENTED_EDGE('',*,*,#13582,.T.);
#17651=ORIENTED_EDGE('',*,*,#13583,.T.);
#17652=ORIENTED_EDGE('',*,*,#13584,.F.);
#17653=ORIENTED_EDGE('',*,*,#13585,.T.);
#17654=ORIENTED_EDGE('',*,*,#13586,.T.);
#17655=ORIENTED_EDGE('',*,*,#13587,.T.);
#17656=ORIENTED_EDGE('',*,*,#13588,.T.);
#17657=ORIENTED_EDGE('',*,*,#13589,.T.);
#17658=ORIENTED_EDGE('',*,*,#13590,.T.);
#17659=ORIENTED_EDGE('',*,*,#13591,.T.);
#17660=ORIENTED_EDGE('',*,*,#13592,.T.);
#17661=ORIENTED_EDGE('',*,*,#13593,.T.);
#17662=ORIENTED_EDGE('',*,*,#13560,.T.);
#17663=ORIENTED_EDGE('',*,*,#13594,.T.);
#17664=ORIENTED_EDGE('',*,*,#13542,.F.);
#17665=ORIENTED_EDGE('',*,*,#13595,.T.);
#17666=ORIENTED_EDGE('',*,*,#13538,.F.);
#17667=ORIENTED_EDGE('',*,*,#13596,.T.);
#17668=ORIENTED_EDGE('',*,*,#13564,.T.);
#17669=ORIENTED_EDGE('',*,*,#13597,.T.);
#17670=ORIENTED_EDGE('',*,*,#13534,.F.);
#17671=ORIENTED_EDGE('',*,*,#13598,.T.);
#17672=ORIENTED_EDGE('',*,*,#13568,.T.);
#17673=ORIENTED_EDGE('',*,*,#13599,.T.);
#17674=ORIENTED_EDGE('',*,*,#13572,.T.);
#17675=ORIENTED_EDGE('',*,*,#13600,.T.);
#17676=ORIENTED_EDGE('',*,*,#13530,.F.);
#17677=ORIENTED_EDGE('',*,*,#13601,.T.);
#17678=ORIENTED_EDGE('',*,*,#13516,.T.);
#17679=ORIENTED_EDGE('',*,*,#13602,.T.);
#17680=ORIENTED_EDGE('',*,*,#13586,.F.);
#17681=ORIENTED_EDGE('',*,*,#13603,.T.);
#17682=ORIENTED_EDGE('',*,*,#13578,.F.);
#17683=ORIENTED_EDGE('',*,*,#13604,.T.);
#17684=ORIENTED_EDGE('',*,*,#13524,.T.);
#17685=ORIENTED_EDGE('',*,*,#13605,.T.);
#17686=ORIENTED_EDGE('',*,*,#13573,.F.);
#17687=ORIENTED_EDGE('',*,*,#13601,.F.);
#17688=ORIENTED_EDGE('',*,*,#13529,.T.);
#17689=ORIENTED_EDGE('',*,*,#13606,.T.);
#17690=ORIENTED_EDGE('',*,*,#13229,.F.);
#17691=ORIENTED_EDGE('',*,*,#13243,.F.);
#17692=ORIENTED_EDGE('',*,*,#13257,.F.);
#17693=ORIENTED_EDGE('',*,*,#13271,.F.);
#17694=ORIENTED_EDGE('',*,*,#13285,.F.);
#17695=ORIENTED_EDGE('',*,*,#13299,.F.);
#17696=ORIENTED_EDGE('',*,*,#13313,.F.);
#17697=ORIENTED_EDGE('',*,*,#13327,.F.);
#17698=ORIENTED_EDGE('',*,*,#13341,.F.);
#17699=ORIENTED_EDGE('',*,*,#13355,.F.);
#17700=ORIENTED_EDGE('',*,*,#13369,.F.);
#17701=ORIENTED_EDGE('',*,*,#13383,.F.);
#17702=ORIENTED_EDGE('',*,*,#13397,.F.);
#17703=ORIENTED_EDGE('',*,*,#13411,.F.);
#17704=ORIENTED_EDGE('',*,*,#13425,.F.);
#17705=ORIENTED_EDGE('',*,*,#13593,.F.);
#17706=ORIENTED_EDGE('',*,*,#13607,.F.);
#17707=ORIENTED_EDGE('',*,*,#13509,.T.);
#17708=ORIENTED_EDGE('',*,*,#13458,.T.);
#17709=ORIENTED_EDGE('',*,*,#13592,.F.);
#17710=ORIENTED_EDGE('',*,*,#13608,.T.);
#17711=ORIENTED_EDGE('',*,*,#13510,.T.);
#17712=ORIENTED_EDGE('',*,*,#13607,.T.);
#17713=ORIENTED_EDGE('',*,*,#13512,.T.);
#17714=ORIENTED_EDGE('',*,*,#13609,.T.);
#17715=ORIENTED_EDGE('',*,*,#13590,.F.);
#17716=ORIENTED_EDGE('',*,*,#13610,.T.);
#17717=ORIENTED_EDGE('',*,*,#13514,.T.);
#17718=ORIENTED_EDGE('',*,*,#13611,.T.);
#17719=ORIENTED_EDGE('',*,*,#13588,.F.);
#17720=ORIENTED_EDGE('',*,*,#13612,.T.);
#17721=ORIENTED_EDGE('',*,*,#13582,.F.);
#17722=ORIENTED_EDGE('',*,*,#13613,.T.);
#17723=ORIENTED_EDGE('',*,*,#13520,.T.);
#17724=ORIENTED_EDGE('',*,*,#13614,.T.);
#17725=ORIENTED_EDGE('',*,*,#13580,.F.);
#17726=ORIENTED_EDGE('',*,*,#13615,.T.);
#17727=ORIENTED_EDGE('',*,*,#13522,.T.);
#17728=ORIENTED_EDGE('',*,*,#13616,.T.);
#17729=ORIENTED_EDGE('',*,*,#13528,.T.);
#17730=ORIENTED_EDGE('',*,*,#13617,.T.);
#17731=ORIENTED_EDGE('',*,*,#13574,.F.);
#17732=ORIENTED_EDGE('',*,*,#13606,.F.);
#17733=ORIENTED_EDGE('',*,*,#13526,.F.);
#17734=ORIENTED_EDGE('',*,*,#13618,.T.);
#17735=ORIENTED_EDGE('',*,*,#13576,.T.);
#17736=ORIENTED_EDGE('',*,*,#13619,.T.);
#17737=ORIENTED_EDGE('',*,*,#13584,.T.);
#17738=ORIENTED_EDGE('',*,*,#13620,.T.);
#17739=ORIENTED_EDGE('',*,*,#13518,.F.);
#17740=ORIENTED_EDGE('',*,*,#13621,.T.);
#17741=ORIENTED_EDGE('',*,*,#13525,.F.);
#17742=ORIENTED_EDGE('',*,*,#13604,.F.);
#17743=ORIENTED_EDGE('',*,*,#13577,.F.);
#17744=ORIENTED_EDGE('',*,*,#13618,.F.);
#17745=ORIENTED_EDGE('',*,*,#13523,.F.);
#17746=ORIENTED_EDGE('',*,*,#13615,.F.);
#17747=ORIENTED_EDGE('',*,*,#13579,.F.);
#17748=ORIENTED_EDGE('',*,*,#13605,.F.);
#17749=ORIENTED_EDGE('',*,*,#13521,.F.);
#17750=ORIENTED_EDGE('',*,*,#13613,.F.);
#17751=ORIENTED_EDGE('',*,*,#13581,.F.);
#17752=ORIENTED_EDGE('',*,*,#13616,.F.);
#17753=ORIENTED_EDGE('',*,*,#13583,.F.);
#17754=ORIENTED_EDGE('',*,*,#13614,.F.);
#17755=ORIENTED_EDGE('',*,*,#13519,.F.);
#17756=ORIENTED_EDGE('',*,*,#13620,.F.);
#17757=ORIENTED_EDGE('',*,*,#13513,.F.);
#17758=ORIENTED_EDGE('',*,*,#13610,.F.);
#17759=ORIENTED_EDGE('',*,*,#13589,.F.);
#17760=ORIENTED_EDGE('',*,*,#13611,.F.);
#17761=ORIENTED_EDGE('',*,*,#13515,.F.);
#17762=ORIENTED_EDGE('',*,*,#13612,.F.);
#17763=ORIENTED_EDGE('',*,*,#13587,.F.);
#17764=ORIENTED_EDGE('',*,*,#13602,.F.);
#17765=ORIENTED_EDGE('',*,*,#13517,.F.);
#17766=ORIENTED_EDGE('',*,*,#13603,.F.);
#17767=ORIENTED_EDGE('',*,*,#13585,.F.);
#17768=ORIENTED_EDGE('',*,*,#13621,.F.);
#17769=ORIENTED_EDGE('',*,*,#13575,.F.);
#17770=ORIENTED_EDGE('',*,*,#13617,.F.);
#17771=ORIENTED_EDGE('',*,*,#13527,.F.);
#17772=ORIENTED_EDGE('',*,*,#13619,.F.);
#17773=ORIENTED_EDGE('',*,*,#13511,.F.);
#17774=ORIENTED_EDGE('',*,*,#13608,.F.);
#17775=ORIENTED_EDGE('',*,*,#13591,.F.);
#17776=ORIENTED_EDGE('',*,*,#13609,.F.);
#17777=ORIENTED_EDGE('',*,*,#13536,.F.);
#17778=ORIENTED_EDGE('',*,*,#13622,.T.);
#17779=ORIENTED_EDGE('',*,*,#13566,.T.);
#17780=ORIENTED_EDGE('',*,*,#13623,.T.);
#17781=ORIENTED_EDGE('',*,*,#13558,.T.);
#17782=ORIENTED_EDGE('',*,*,#13624,.T.);
#17783=ORIENTED_EDGE('',*,*,#13544,.F.);
#17784=ORIENTED_EDGE('',*,*,#13625,.T.);
#17785=ORIENTED_EDGE('',*,*,#13556,.T.);
#17786=ORIENTED_EDGE('',*,*,#13626,.T.);
#17787=ORIENTED_EDGE('',*,*,#13546,.F.);
#17788=ORIENTED_EDGE('',*,*,#13627,.T.);
#17789=ORIENTED_EDGE('',*,*,#13548,.F.);
#17790=ORIENTED_EDGE('',*,*,#13628,.T.);
#17791=ORIENTED_EDGE('',*,*,#13554,.T.);
#17792=ORIENTED_EDGE('',*,*,#13629,.F.);
#17793=ORIENTED_EDGE('',*,*,#13553,.T.);
#17794=ORIENTED_EDGE('',*,*,#13463,.F.);
#17795=ORIENTED_EDGE('',*,*,#13549,.F.);
#17796=ORIENTED_EDGE('',*,*,#13629,.T.);
#17797=ORIENTED_EDGE('',*,*,#13570,.F.);
#17798=ORIENTED_EDGE('',*,*,#13630,.T.);
#17799=ORIENTED_EDGE('',*,*,#13532,.T.);
#17800=ORIENTED_EDGE('',*,*,#13631,.T.);
#17801=ORIENTED_EDGE('',*,*,#13540,.T.);
#17802=ORIENTED_EDGE('',*,*,#13632,.T.);
#17803=ORIENTED_EDGE('',*,*,#13562,.F.);
#17804=ORIENTED_EDGE('',*,*,#13633,.T.);
#17805=ORIENTED_EDGE('',*,*,#13569,.F.);
#17806=ORIENTED_EDGE('',*,*,#13598,.F.);
#17807=ORIENTED_EDGE('',*,*,#13533,.F.);
#17808=ORIENTED_EDGE('',*,*,#13630,.F.);
#17809=ORIENTED_EDGE('',*,*,#13535,.F.);
#17810=ORIENTED_EDGE('',*,*,#13599,.F.);
#17811=ORIENTED_EDGE('',*,*,#13567,.F.);
#17812=ORIENTED_EDGE('',*,*,#13622,.F.);
#17813=ORIENTED_EDGE('',*,*,#13537,.F.);
#17814=ORIENTED_EDGE('',*,*,#13623,.F.);
#17815=ORIENTED_EDGE('',*,*,#13565,.F.);
#17816=ORIENTED_EDGE('',*,*,#13596,.F.);
#17817=ORIENTED_EDGE('',*,*,#13539,.F.);
#17818=ORIENTED_EDGE('',*,*,#13597,.F.);
#17819=ORIENTED_EDGE('',*,*,#13563,.F.);
#17820=ORIENTED_EDGE('',*,*,#13632,.F.);
#17821=ORIENTED_EDGE('',*,*,#13545,.F.);
#17822=ORIENTED_EDGE('',*,*,#13624,.F.);
#17823=ORIENTED_EDGE('',*,*,#13557,.F.);
#17824=ORIENTED_EDGE('',*,*,#13627,.F.);
#17825=ORIENTED_EDGE('',*,*,#13543,.F.);
#17826=ORIENTED_EDGE('',*,*,#13594,.F.);
#17827=ORIENTED_EDGE('',*,*,#13559,.F.);
#17828=ORIENTED_EDGE('',*,*,#13625,.F.);
#17829=ORIENTED_EDGE('',*,*,#13561,.F.);
#17830=ORIENTED_EDGE('',*,*,#13595,.F.);
#17831=ORIENTED_EDGE('',*,*,#13541,.F.);
#17832=ORIENTED_EDGE('',*,*,#13633,.F.);
#17833=ORIENTED_EDGE('',*,*,#13531,.F.);
#17834=ORIENTED_EDGE('',*,*,#13600,.F.);
#17835=ORIENTED_EDGE('',*,*,#13571,.F.);
#17836=ORIENTED_EDGE('',*,*,#13631,.F.);
#17837=ORIENTED_EDGE('',*,*,#13547,.F.);
#17838=ORIENTED_EDGE('',*,*,#13626,.F.);
#17839=ORIENTED_EDGE('',*,*,#13555,.F.);
#17840=ORIENTED_EDGE('',*,*,#13628,.F.);
#17841=ORIENTED_EDGE('',*,*,#13456,.F.);
#17842=ORIENTED_EDGE('',*,*,#13427,.T.);
#17843=ORIENTED_EDGE('',*,*,#13505,.T.);
#17844=ORIENTED_EDGE('',*,*,#13552,.T.);
#17845=ORIENTED_EDGE('',*,*,#13634,.T.);
#17846=ORIENTED_EDGE('',*,*,#13237,.T.);
#17847=ORIENTED_EDGE('',*,*,#13234,.T.);
#17848=ORIENTED_EDGE('',*,*,#13437,.F.);
#17849=ORIENTED_EDGE('',*,*,#13551,.F.);
#17850=ORIENTED_EDGE('',*,*,#13461,.T.);
#17851=ORIENTED_EDGE('',*,*,#13238,.T.);
#17852=ORIENTED_EDGE('',*,*,#13634,.F.);
#17853=ORIENTED_EDGE('',*,*,#13550,.F.);
#17854=ORIENTED_EDGE('',*,*,#13423,.T.);
#17855=ORIENTED_EDGE('',*,*,#13432,.F.);
#17856=ORIENTED_EDGE('',*,*,#13409,.T.);
#17857=ORIENTED_EDGE('',*,*,#13418,.F.);
#17858=ORIENTED_EDGE('',*,*,#13395,.T.);
#17859=ORIENTED_EDGE('',*,*,#13404,.F.);
#17860=ORIENTED_EDGE('',*,*,#13381,.T.);
#17861=ORIENTED_EDGE('',*,*,#13390,.F.);
#17862=ORIENTED_EDGE('',*,*,#13367,.T.);
#17863=ORIENTED_EDGE('',*,*,#13376,.F.);
#17864=ORIENTED_EDGE('',*,*,#13353,.T.);
#17865=ORIENTED_EDGE('',*,*,#13362,.F.);
#17866=ORIENTED_EDGE('',*,*,#13339,.T.);
#17867=ORIENTED_EDGE('',*,*,#13348,.F.);
#17868=ORIENTED_EDGE('',*,*,#13325,.T.);
#17869=ORIENTED_EDGE('',*,*,#13334,.F.);
#17870=ORIENTED_EDGE('',*,*,#13311,.T.);
#17871=ORIENTED_EDGE('',*,*,#13320,.F.);
#17872=ORIENTED_EDGE('',*,*,#13297,.T.);
#17873=ORIENTED_EDGE('',*,*,#13306,.F.);
#17874=ORIENTED_EDGE('',*,*,#13283,.T.);
#17875=ORIENTED_EDGE('',*,*,#13292,.F.);
#17876=ORIENTED_EDGE('',*,*,#13269,.T.);
#17877=ORIENTED_EDGE('',*,*,#13278,.F.);
#17878=ORIENTED_EDGE('',*,*,#13255,.T.);
#17879=ORIENTED_EDGE('',*,*,#13264,.F.);
#17880=ORIENTED_EDGE('',*,*,#13241,.T.);
#17881=ORIENTED_EDGE('',*,*,#13250,.F.);
#17882=ORIENTED_EDGE('',*,*,#13227,.T.);
#17883=ORIENTED_EDGE('',*,*,#13236,.F.);
#17884=ORIENTED_EDGE('',*,*,#13635,.F.);
#17885=ORIENTED_EDGE('',*,*,#13636,.T.);
#17886=ORIENTED_EDGE('',*,*,#13637,.T.);
#17887=ORIENTED_EDGE('',*,*,#13636,.F.);
#17888=ORIENTED_EDGE('',*,*,#13638,.F.);
#17889=ORIENTED_EDGE('',*,*,#13639,.T.);
#17890=ORIENTED_EDGE('',*,*,#13640,.T.);
#17891=ORIENTED_EDGE('',*,*,#13639,.F.);
#17892=ORIENTED_EDGE('',*,*,#13641,.F.);
#17893=ORIENTED_EDGE('',*,*,#13642,.T.);
#17894=ORIENTED_EDGE('',*,*,#13643,.T.);
#17895=ORIENTED_EDGE('',*,*,#13642,.F.);
#17896=ORIENTED_EDGE('',*,*,#13644,.T.);
#17897=ORIENTED_EDGE('',*,*,#13635,.T.);
#17898=ORIENTED_EDGE('',*,*,#13644,.F.);
#17899=ORIENTED_EDGE('',*,*,#13645,.T.);
#17900=ORIENTED_EDGE('',*,*,#13638,.T.);
#17901=ORIENTED_EDGE('',*,*,#13645,.F.);
#17902=ORIENTED_EDGE('',*,*,#13646,.F.);
#17903=ORIENTED_EDGE('',*,*,#13647,.T.);
#17904=ORIENTED_EDGE('',*,*,#13648,.T.);
#17905=ORIENTED_EDGE('',*,*,#13647,.F.);
#17906=ORIENTED_EDGE('',*,*,#13649,.F.);
#17907=ORIENTED_EDGE('',*,*,#13650,.T.);
#17908=ORIENTED_EDGE('',*,*,#13651,.T.);
#17909=ORIENTED_EDGE('',*,*,#13650,.F.);
#17910=ORIENTED_EDGE('',*,*,#13652,.F.);
#17911=ORIENTED_EDGE('',*,*,#13653,.T.);
#17912=ORIENTED_EDGE('',*,*,#13654,.T.);
#17913=ORIENTED_EDGE('',*,*,#13653,.F.);
#17914=ORIENTED_EDGE('',*,*,#13655,.F.);
#17915=ORIENTED_EDGE('',*,*,#13656,.T.);
#17916=ORIENTED_EDGE('',*,*,#13657,.T.);
#17917=ORIENTED_EDGE('',*,*,#13656,.F.);
#17918=ORIENTED_EDGE('',*,*,#13658,.F.);
#17919=ORIENTED_EDGE('',*,*,#13659,.T.);
#17920=ORIENTED_EDGE('',*,*,#13660,.T.);
#17921=ORIENTED_EDGE('',*,*,#13659,.F.);
#17922=ORIENTED_EDGE('',*,*,#13661,.F.);
#17923=ORIENTED_EDGE('',*,*,#13662,.T.);
#17924=ORIENTED_EDGE('',*,*,#13663,.T.);
#17925=ORIENTED_EDGE('',*,*,#13662,.F.);
#17926=ORIENTED_EDGE('',*,*,#13664,.F.);
#17927=ORIENTED_EDGE('',*,*,#13665,.T.);
#17928=ORIENTED_EDGE('',*,*,#13666,.T.);
#17929=ORIENTED_EDGE('',*,*,#13665,.F.);
#17930=ORIENTED_EDGE('',*,*,#13667,.F.);
#17931=ORIENTED_EDGE('',*,*,#13668,.T.);
#17932=ORIENTED_EDGE('',*,*,#13669,.T.);
#17933=ORIENTED_EDGE('',*,*,#13670,.T.);
#17934=ORIENTED_EDGE('',*,*,#13671,.T.);
#17935=ORIENTED_EDGE('',*,*,#13672,.F.);
#17936=ORIENTED_EDGE('',*,*,#13668,.F.);
#17937=ORIENTED_EDGE('',*,*,#13673,.T.);
#17938=ORIENTED_EDGE('',*,*,#13658,.T.);
#17939=ORIENTED_EDGE('',*,*,#13673,.F.);
#17940=ORIENTED_EDGE('',*,*,#13674,.T.);
#17941=ORIENTED_EDGE('',*,*,#13661,.T.);
#17942=ORIENTED_EDGE('',*,*,#13674,.F.);
#17943=ORIENTED_EDGE('',*,*,#13675,.F.);
#17944=ORIENTED_EDGE('',*,*,#13676,.T.);
#17945=ORIENTED_EDGE('',*,*,#13677,.T.);
#17946=ORIENTED_EDGE('',*,*,#13678,.T.);
#17947=ORIENTED_EDGE('',*,*,#13679,.F.);
#17948=ORIENTED_EDGE('',*,*,#13680,.T.);
#17949=ORIENTED_EDGE('',*,*,#13676,.F.);
#17950=ORIENTED_EDGE('',*,*,#13681,.F.);
#17951=ORIENTED_EDGE('',*,*,#13682,.F.);
#17952=ORIENTED_EDGE('',*,*,#13683,.F.);
#17953=ORIENTED_EDGE('',*,*,#13684,.T.);
#17954=ORIENTED_EDGE('',*,*,#13685,.F.);
#17955=ORIENTED_EDGE('',*,*,#13686,.F.);
#17956=ORIENTED_EDGE('',*,*,#13684,.F.);
#17957=ORIENTED_EDGE('',*,*,#13687,.F.);
#17958=ORIENTED_EDGE('',*,*,#13688,.F.);
#17959=ORIENTED_EDGE('',*,*,#13689,.F.);
#17960=ORIENTED_EDGE('',*,*,#13690,.T.);
#17961=ORIENTED_EDGE('',*,*,#13691,.T.);
#17962=ORIENTED_EDGE('',*,*,#13685,.T.);
#17963=ORIENTED_EDGE('',*,*,#13686,.T.);
#17964=ORIENTED_EDGE('',*,*,#13691,.F.);
#17965=ORIENTED_EDGE('',*,*,#13692,.F.);
#17966=ORIENTED_EDGE('',*,*,#13693,.T.);
#17967=ORIENTED_EDGE('',*,*,#13694,.T.);
#17968=ORIENTED_EDGE('',*,*,#13693,.F.);
#17969=ORIENTED_EDGE('',*,*,#13695,.F.);
#17970=ORIENTED_EDGE('',*,*,#13696,.F.);
#17971=ORIENTED_EDGE('',*,*,#13697,.T.);
#17972=ORIENTED_EDGE('',*,*,#13698,.T.);
#17973=ORIENTED_EDGE('',*,*,#13699,.F.);
#17974=ORIENTED_EDGE('',*,*,#13700,.T.);
#17975=ORIENTED_EDGE('',*,*,#13701,.F.);
#17976=ORIENTED_EDGE('',*,*,#13702,.F.);
#17977=ORIENTED_EDGE('',*,*,#13703,.F.);
#17978=ORIENTED_EDGE('',*,*,#13704,.T.);
#17979=ORIENTED_EDGE('',*,*,#13705,.F.);
#17980=ORIENTED_EDGE('',*,*,#13706,.F.);
#17981=ORIENTED_EDGE('',*,*,#13707,.F.);
#17982=ORIENTED_EDGE('',*,*,#13708,.T.);
#17983=ORIENTED_EDGE('',*,*,#13709,.F.);
#17984=ORIENTED_EDGE('',*,*,#13710,.F.);
#17985=ORIENTED_EDGE('',*,*,#13711,.F.);
#17986=ORIENTED_EDGE('',*,*,#13712,.T.);
#17987=ORIENTED_EDGE('',*,*,#13713,.T.);
#17988=ORIENTED_EDGE('',*,*,#13714,.T.);
#17989=ORIENTED_EDGE('',*,*,#13715,.F.);
#17990=ORIENTED_EDGE('',*,*,#13716,.T.);
#17991=ORIENTED_EDGE('',*,*,#13717,.T.);
#17992=ORIENTED_EDGE('',*,*,#13718,.T.);
#17993=ORIENTED_EDGE('',*,*,#13719,.F.);
#17994=ORIENTED_EDGE('',*,*,#13720,.T.);
#17995=ORIENTED_EDGE('',*,*,#13721,.T.);
#17996=ORIENTED_EDGE('',*,*,#13722,.T.);
#17997=ORIENTED_EDGE('',*,*,#13723,.F.);
#17998=ORIENTED_EDGE('',*,*,#13724,.T.);
#17999=ORIENTED_EDGE('',*,*,#13725,.T.);
#18000=ORIENTED_EDGE('',*,*,#13726,.T.);
#18001=ORIENTED_EDGE('',*,*,#13727,.F.);
#18002=ORIENTED_EDGE('',*,*,#13728,.T.);
#18003=ORIENTED_EDGE('',*,*,#13729,.T.);
#18004=ORIENTED_EDGE('',*,*,#13730,.T.);
#18005=ORIENTED_EDGE('',*,*,#13731,.F.);
#18006=ORIENTED_EDGE('',*,*,#13732,.T.);
#18007=ORIENTED_EDGE('',*,*,#13733,.T.);
#18008=ORIENTED_EDGE('',*,*,#13734,.T.);
#18009=ORIENTED_EDGE('',*,*,#13735,.F.);
#18010=ORIENTED_EDGE('',*,*,#13736,.T.);
#18011=ORIENTED_EDGE('',*,*,#13737,.T.);
#18012=ORIENTED_EDGE('',*,*,#13738,.T.);
#18013=ORIENTED_EDGE('',*,*,#13739,.F.);
#18014=ORIENTED_EDGE('',*,*,#13740,.T.);
#18015=ORIENTED_EDGE('',*,*,#13741,.T.);
#18016=ORIENTED_EDGE('',*,*,#13742,.T.);
#18017=ORIENTED_EDGE('',*,*,#13743,.F.);
#18018=ORIENTED_EDGE('',*,*,#13744,.F.);
#18019=ORIENTED_EDGE('',*,*,#13745,.T.);
#18020=ORIENTED_EDGE('',*,*,#13746,.T.);
#18021=ORIENTED_EDGE('',*,*,#13747,.F.);
#18022=ORIENTED_EDGE('',*,*,#13748,.F.);
#18023=ORIENTED_EDGE('',*,*,#13749,.T.);
#18024=ORIENTED_EDGE('',*,*,#13744,.T.);
#18025=ORIENTED_EDGE('',*,*,#13750,.F.);
#18026=ORIENTED_EDGE('',*,*,#13751,.F.);
#18027=ORIENTED_EDGE('',*,*,#13752,.T.);
#18028=ORIENTED_EDGE('',*,*,#13753,.T.);
#18029=ORIENTED_EDGE('',*,*,#13754,.F.);
#18030=ORIENTED_EDGE('',*,*,#13755,.T.);
#18031=ORIENTED_EDGE('',*,*,#13756,.T.);
#18032=ORIENTED_EDGE('',*,*,#13751,.T.);
#18033=ORIENTED_EDGE('',*,*,#13757,.F.);
#18034=ORIENTED_EDGE('',*,*,#13758,.T.);
#18035=ORIENTED_EDGE('',*,*,#13759,.T.);
#18036=ORIENTED_EDGE('',*,*,#13760,.T.);
#18037=ORIENTED_EDGE('',*,*,#13761,.F.);
#18038=ORIENTED_EDGE('',*,*,#13762,.T.);
#18039=ORIENTED_EDGE('',*,*,#13763,.T.);
#18040=ORIENTED_EDGE('',*,*,#13764,.T.);
#18041=ORIENTED_EDGE('',*,*,#13765,.F.);
#18042=ORIENTED_EDGE('',*,*,#13766,.T.);
#18043=ORIENTED_EDGE('',*,*,#13767,.T.);
#18044=ORIENTED_EDGE('',*,*,#13768,.T.);
#18045=ORIENTED_EDGE('',*,*,#13769,.F.);
#18046=ORIENTED_EDGE('',*,*,#13770,.F.);
#18047=ORIENTED_EDGE('',*,*,#13771,.T.);
#18048=ORIENTED_EDGE('',*,*,#13772,.T.);
#18049=ORIENTED_EDGE('',*,*,#13773,.F.);
#18050=ORIENTED_EDGE('',*,*,#13726,.F.);
#18051=ORIENTED_EDGE('',*,*,#13774,.T.);
#18052=ORIENTED_EDGE('',*,*,#13770,.T.);
#18053=ORIENTED_EDGE('',*,*,#13775,.F.);
#18054=ORIENTED_EDGE('',*,*,#13776,.T.);
#18055=ORIENTED_EDGE('',*,*,#13777,.T.);
#18056=ORIENTED_EDGE('',*,*,#13778,.T.);
#18057=ORIENTED_EDGE('',*,*,#13779,.F.);
#18058=ORIENTED_EDGE('',*,*,#13780,.T.);
#18059=ORIENTED_EDGE('',*,*,#13781,.T.);
#18060=ORIENTED_EDGE('',*,*,#13782,.T.);
#18061=ORIENTED_EDGE('',*,*,#13783,.F.);
#18062=ORIENTED_EDGE('',*,*,#13784,.T.);
#18063=ORIENTED_EDGE('',*,*,#13785,.T.);
#18064=ORIENTED_EDGE('',*,*,#13786,.T.);
#18065=ORIENTED_EDGE('',*,*,#13787,.F.);
#18066=ORIENTED_EDGE('',*,*,#13788,.T.);
#18067=ORIENTED_EDGE('',*,*,#13789,.T.);
#18068=ORIENTED_EDGE('',*,*,#13790,.T.);
#18069=ORIENTED_EDGE('',*,*,#13791,.F.);
#18070=ORIENTED_EDGE('',*,*,#13760,.F.);
#18071=ORIENTED_EDGE('',*,*,#13792,.F.);
#18072=ORIENTED_EDGE('',*,*,#13755,.F.);
#18073=ORIENTED_EDGE('',*,*,#13793,.F.);
#18074=ORIENTED_EDGE('',*,*,#13746,.F.);
#18075=ORIENTED_EDGE('',*,*,#13794,.F.);
#18076=ORIENTED_EDGE('',*,*,#13740,.F.);
#18077=ORIENTED_EDGE('',*,*,#13762,.F.);
#18078=ORIENTED_EDGE('',*,*,#13795,.F.);
#18079=ORIENTED_EDGE('',*,*,#13768,.F.);
#18080=ORIENTED_EDGE('',*,*,#13796,.F.);
#18081=ORIENTED_EDGE('',*,*,#13766,.F.);
#18082=ORIENTED_EDGE('',*,*,#13797,.F.);
#18083=ORIENTED_EDGE('',*,*,#13718,.F.);
#18084=ORIENTED_EDGE('',*,*,#13798,.F.);
#18085=ORIENTED_EDGE('',*,*,#13716,.F.);
#18086=ORIENTED_EDGE('',*,*,#13799,.F.);
#18087=ORIENTED_EDGE('',*,*,#13786,.F.);
#18088=ORIENTED_EDGE('',*,*,#13800,.F.);
#18089=ORIENTED_EDGE('',*,*,#13784,.F.);
#18090=ORIENTED_EDGE('',*,*,#13801,.F.);
#18091=ORIENTED_EDGE('',*,*,#13772,.F.);
#18092=ORIENTED_EDGE('',*,*,#13802,.F.);
#18093=ORIENTED_EDGE('',*,*,#13788,.F.);
#18094=ORIENTED_EDGE('',*,*,#13803,.F.);
#18095=ORIENTED_EDGE('',*,*,#13764,.F.);
#18096=ORIENTED_EDGE('',*,*,#13804,.F.);
#18097=ORIENTED_EDGE('',*,*,#13712,.F.);
#18098=ORIENTED_EDGE('',*,*,#13805,.F.);
#18099=ORIENTED_EDGE('',*,*,#13790,.F.);
#18100=ORIENTED_EDGE('',*,*,#13806,.F.);
#18101=ORIENTED_EDGE('',*,*,#13807,.F.);
#18102=ORIENTED_EDGE('',*,*,#13714,.F.);
#18103=ORIENTED_EDGE('',*,*,#13808,.F.);
#18104=ORIENTED_EDGE('',*,*,#13758,.F.);
#18105=ORIENTED_EDGE('',*,*,#13809,.F.);
#18106=ORIENTED_EDGE('',*,*,#13742,.F.);
#18107=ORIENTED_EDGE('',*,*,#13810,.F.);
#18108=ORIENTED_EDGE('',*,*,#13736,.F.);
#18109=ORIENTED_EDGE('',*,*,#13780,.F.);
#18110=ORIENTED_EDGE('',*,*,#13811,.F.);
#18111=ORIENTED_EDGE('',*,*,#13738,.F.);
#18112=ORIENTED_EDGE('',*,*,#13812,.F.);
#18113=ORIENTED_EDGE('',*,*,#13720,.F.);
#18114=ORIENTED_EDGE('',*,*,#13813,.F.);
#18115=ORIENTED_EDGE('',*,*,#13782,.F.);
#18116=ORIENTED_EDGE('',*,*,#13814,.F.);
#18117=ORIENTED_EDGE('',*,*,#13732,.F.);
#18118=ORIENTED_EDGE('',*,*,#13815,.F.);
#18119=ORIENTED_EDGE('',*,*,#13722,.F.);
#18120=ORIENTED_EDGE('',*,*,#13816,.F.);
#18121=ORIENTED_EDGE('',*,*,#13728,.F.);
#18122=ORIENTED_EDGE('',*,*,#13817,.F.);
#18123=ORIENTED_EDGE('',*,*,#13734,.F.);
#18124=ORIENTED_EDGE('',*,*,#13818,.F.);
#18125=ORIENTED_EDGE('',*,*,#13776,.F.);
#18126=ORIENTED_EDGE('',*,*,#13819,.F.);
#18127=ORIENTED_EDGE('',*,*,#13730,.F.);
#18128=ORIENTED_EDGE('',*,*,#13820,.F.);
#18129=ORIENTED_EDGE('',*,*,#13724,.F.);
#18130=ORIENTED_EDGE('',*,*,#13821,.F.);
#18131=ORIENTED_EDGE('',*,*,#13778,.F.);
#18132=ORIENTED_EDGE('',*,*,#13822,.F.);
#18133=ORIENTED_EDGE('',*,*,#13692,.T.);
#18134=ORIENTED_EDGE('',*,*,#13690,.F.);
#18135=ORIENTED_EDGE('',*,*,#13823,.T.);
#18136=ORIENTED_EDGE('',*,*,#13824,.F.);
#18137=ORIENTED_EDGE('',*,*,#13825,.F.);
#18138=ORIENTED_EDGE('',*,*,#13826,.F.);
#18139=ORIENTED_EDGE('',*,*,#13827,.T.);
#18140=ORIENTED_EDGE('',*,*,#13828,.T.);
#18141=ORIENTED_EDGE('',*,*,#13829,.T.);
#18142=ORIENTED_EDGE('',*,*,#13826,.T.);
#18143=ORIENTED_EDGE('',*,*,#13830,.T.);
#18144=ORIENTED_EDGE('',*,*,#13831,.T.);
#18145=ORIENTED_EDGE('',*,*,#13832,.T.);
#18146=ORIENTED_EDGE('',*,*,#13752,.F.);
#18147=ORIENTED_EDGE('',*,*,#13756,.F.);
#18148=ORIENTED_EDGE('',*,*,#13792,.T.);
#18149=ORIENTED_EDGE('',*,*,#13759,.F.);
#18150=ORIENTED_EDGE('',*,*,#13808,.T.);
#18151=ORIENTED_EDGE('',*,*,#13713,.F.);
#18152=ORIENTED_EDGE('',*,*,#13806,.T.);
#18153=ORIENTED_EDGE('',*,*,#13789,.F.);
#18154=ORIENTED_EDGE('',*,*,#13804,.T.);
#18155=ORIENTED_EDGE('',*,*,#13763,.F.);
#18156=ORIENTED_EDGE('',*,*,#13796,.T.);
#18157=ORIENTED_EDGE('',*,*,#13767,.F.);
#18158=ORIENTED_EDGE('',*,*,#13798,.T.);
#18159=ORIENTED_EDGE('',*,*,#13717,.F.);
#18160=ORIENTED_EDGE('',*,*,#13800,.T.);
#18161=ORIENTED_EDGE('',*,*,#13785,.F.);
#18162=ORIENTED_EDGE('',*,*,#13802,.T.);
#18163=ORIENTED_EDGE('',*,*,#13771,.F.);
#18164=ORIENTED_EDGE('',*,*,#13774,.F.);
#18165=ORIENTED_EDGE('',*,*,#13725,.F.);
#18166=ORIENTED_EDGE('',*,*,#13822,.T.);
#18167=ORIENTED_EDGE('',*,*,#13777,.F.);
#18168=ORIENTED_EDGE('',*,*,#13820,.T.);
#18169=ORIENTED_EDGE('',*,*,#13729,.F.);
#18170=ORIENTED_EDGE('',*,*,#13818,.T.);
#18171=ORIENTED_EDGE('',*,*,#13733,.F.);
#18172=ORIENTED_EDGE('',*,*,#13816,.T.);
#18173=ORIENTED_EDGE('',*,*,#13721,.F.);
#18174=ORIENTED_EDGE('',*,*,#13814,.T.);
#18175=ORIENTED_EDGE('',*,*,#13781,.F.);
#18176=ORIENTED_EDGE('',*,*,#13812,.T.);
#18177=ORIENTED_EDGE('',*,*,#13737,.F.);
#18178=ORIENTED_EDGE('',*,*,#13810,.T.);
#18179=ORIENTED_EDGE('',*,*,#13741,.F.);
#18180=ORIENTED_EDGE('',*,*,#13794,.T.);
#18181=ORIENTED_EDGE('',*,*,#13745,.F.);
#18182=ORIENTED_EDGE('',*,*,#13749,.F.);
#18183=ORIENTED_EDGE('',*,*,#13694,.F.);
#18184=ORIENTED_EDGE('',*,*,#13833,.T.);
#18185=ORIENTED_EDGE('',*,*,#13834,.F.);
#18186=ORIENTED_EDGE('',*,*,#13823,.F.);
#18187=ORIENTED_EDGE('',*,*,#13829,.F.);
#18188=ORIENTED_EDGE('',*,*,#13835,.T.);
#18189=ORIENTED_EDGE('',*,*,#13836,.F.);
#18190=ORIENTED_EDGE('',*,*,#13833,.F.);
#18191=ORIENTED_EDGE('',*,*,#13828,.F.);
#18192=ORIENTED_EDGE('',*,*,#13748,.T.);
#18193=ORIENTED_EDGE('',*,*,#13837,.F.);
#18194=ORIENTED_EDGE('',*,*,#13835,.F.);
#18195=ORIENTED_EDGE('',*,*,#13827,.F.);
#18196=ORIENTED_EDGE('',*,*,#13838,.T.);
#18197=ORIENTED_EDGE('',*,*,#13839,.F.);
#18198=ORIENTED_EDGE('',*,*,#13753,.F.);
#18199=ORIENTED_EDGE('',*,*,#13832,.F.);
#18200=ORIENTED_EDGE('',*,*,#13840,.T.);
#18201=ORIENTED_EDGE('',*,*,#13841,.F.);
#18202=ORIENTED_EDGE('',*,*,#13838,.F.);
#18203=ORIENTED_EDGE('',*,*,#13831,.F.);
#18204=ORIENTED_EDGE('',*,*,#13825,.T.);
#18205=ORIENTED_EDGE('',*,*,#13842,.F.);
#18206=ORIENTED_EDGE('',*,*,#13840,.F.);
#18207=ORIENTED_EDGE('',*,*,#13830,.F.);
#18208=ORIENTED_EDGE('',*,*,#13843,.T.);
#18209=ORIENTED_EDGE('',*,*,#13689,.T.);
#18210=ORIENTED_EDGE('',*,*,#13844,.F.);
#18211=ORIENTED_EDGE('',*,*,#13845,.F.);
#18212=ORIENTED_EDGE('',*,*,#13681,.T.);
#18213=ORIENTED_EDGE('',*,*,#13843,.F.);
#18214=ORIENTED_EDGE('',*,*,#13846,.F.);
#18215=ORIENTED_EDGE('',*,*,#13847,.T.);
#18216=ORIENTED_EDGE('',*,*,#13848,.T.);
#18217=ORIENTED_EDGE('',*,*,#13682,.T.);
#18218=ORIENTED_EDGE('',*,*,#13847,.F.);
#18219=ORIENTED_EDGE('',*,*,#13849,.F.);
#18220=ORIENTED_EDGE('',*,*,#13850,.T.);
#18221=ORIENTED_EDGE('',*,*,#13683,.T.);
#18222=ORIENTED_EDGE('',*,*,#13848,.F.);
#18223=ORIENTED_EDGE('',*,*,#13851,.F.);
#18224=ORIENTED_EDGE('',*,*,#13852,.T.);
#18225=ORIENTED_EDGE('',*,*,#13687,.T.);
#18226=ORIENTED_EDGE('',*,*,#13850,.F.);
#18227=ORIENTED_EDGE('',*,*,#13853,.F.);
#18228=ORIENTED_EDGE('',*,*,#13844,.T.);
#18229=ORIENTED_EDGE('',*,*,#13688,.T.);
#18230=ORIENTED_EDGE('',*,*,#13852,.F.);
#18231=ORIENTED_EDGE('',*,*,#13854,.F.);
#18232=ORIENTED_EDGE('',*,*,#13845,.T.);
#18233=ORIENTED_EDGE('',*,*,#13854,.T.);
#18234=ORIENTED_EDGE('',*,*,#13853,.T.);
#18235=ORIENTED_EDGE('',*,*,#13851,.T.);
#18236=ORIENTED_EDGE('',*,*,#13849,.T.);
#18237=ORIENTED_EDGE('',*,*,#13846,.T.);
#18238=ORIENTED_EDGE('',*,*,#13754,.T.);
#18239=ORIENTED_EDGE('',*,*,#13750,.T.);
#18240=ORIENTED_EDGE('',*,*,#13839,.T.);
#18241=ORIENTED_EDGE('',*,*,#13841,.T.);
#18242=ORIENTED_EDGE('',*,*,#13842,.T.);
#18243=ORIENTED_EDGE('',*,*,#13824,.T.);
#18244=ORIENTED_EDGE('',*,*,#13834,.T.);
#18245=ORIENTED_EDGE('',*,*,#13836,.T.);
#18246=ORIENTED_EDGE('',*,*,#13837,.T.);
#18247=ORIENTED_EDGE('',*,*,#13747,.T.);
#18248=ORIENTED_EDGE('',*,*,#13743,.T.);
#18249=ORIENTED_EDGE('',*,*,#13793,.T.);
#18250=ORIENTED_EDGE('',*,*,#13739,.T.);
#18251=ORIENTED_EDGE('',*,*,#13809,.T.);
#18252=ORIENTED_EDGE('',*,*,#13735,.T.);
#18253=ORIENTED_EDGE('',*,*,#13811,.T.);
#18254=ORIENTED_EDGE('',*,*,#13779,.T.);
#18255=ORIENTED_EDGE('',*,*,#13813,.T.);
#18256=ORIENTED_EDGE('',*,*,#13719,.T.);
#18257=ORIENTED_EDGE('',*,*,#13815,.T.);
#18258=ORIENTED_EDGE('',*,*,#13731,.T.);
#18259=ORIENTED_EDGE('',*,*,#13817,.T.);
#18260=ORIENTED_EDGE('',*,*,#13727,.T.);
#18261=ORIENTED_EDGE('',*,*,#13819,.T.);
#18262=ORIENTED_EDGE('',*,*,#13775,.T.);
#18263=ORIENTED_EDGE('',*,*,#13821,.T.);
#18264=ORIENTED_EDGE('',*,*,#13723,.T.);
#18265=ORIENTED_EDGE('',*,*,#13773,.T.);
#18266=ORIENTED_EDGE('',*,*,#13769,.T.);
#18267=ORIENTED_EDGE('',*,*,#13801,.T.);
#18268=ORIENTED_EDGE('',*,*,#13783,.T.);
#18269=ORIENTED_EDGE('',*,*,#13799,.T.);
#18270=ORIENTED_EDGE('',*,*,#13715,.T.);
#18271=ORIENTED_EDGE('',*,*,#13797,.T.);
#18272=ORIENTED_EDGE('',*,*,#13765,.T.);
#18273=ORIENTED_EDGE('',*,*,#13795,.T.);
#18274=ORIENTED_EDGE('',*,*,#13761,.T.);
#18275=ORIENTED_EDGE('',*,*,#13803,.T.);
#18276=ORIENTED_EDGE('',*,*,#13787,.T.);
#18277=ORIENTED_EDGE('',*,*,#13805,.T.);
#18278=ORIENTED_EDGE('',*,*,#13711,.T.);
#18279=ORIENTED_EDGE('',*,*,#13807,.T.);
#18280=ORIENTED_EDGE('',*,*,#13757,.T.);
#18281=ORIENTED_EDGE('',*,*,#13791,.T.);
#18282=ORIENTED_EDGE('',*,*,#13855,.F.);
#18283=ORIENTED_EDGE('',*,*,#13856,.F.);
#18284=ORIENTED_EDGE('',*,*,#13857,.F.);
#18285=ORIENTED_EDGE('',*,*,#13858,.F.);
#18286=ORIENTED_EDGE('',*,*,#13859,.F.);
#18287=ORIENTED_EDGE('',*,*,#13860,.F.);
#18288=ORIENTED_EDGE('',*,*,#13861,.F.);
#18289=ORIENTED_EDGE('',*,*,#13862,.F.);
#18290=ORIENTED_EDGE('',*,*,#13863,.F.);
#18291=ORIENTED_EDGE('',*,*,#13864,.F.);
#18292=ORIENTED_EDGE('',*,*,#13865,.F.);
#18293=ORIENTED_EDGE('',*,*,#13866,.F.);
#18294=ORIENTED_EDGE('',*,*,#13867,.F.);
#18295=ORIENTED_EDGE('',*,*,#13868,.F.);
#18296=ORIENTED_EDGE('',*,*,#13869,.F.);
#18297=ORIENTED_EDGE('',*,*,#13870,.F.);
#18298=ORIENTED_EDGE('',*,*,#13871,.F.);
#18299=ORIENTED_EDGE('',*,*,#13872,.F.);
#18300=ORIENTED_EDGE('',*,*,#13873,.F.);
#18301=ORIENTED_EDGE('',*,*,#13874,.F.);
#18302=ORIENTED_EDGE('',*,*,#13875,.F.);
#18303=ORIENTED_EDGE('',*,*,#13876,.F.);
#18304=ORIENTED_EDGE('',*,*,#13877,.F.);
#18305=ORIENTED_EDGE('',*,*,#13878,.F.);
#18306=ORIENTED_EDGE('',*,*,#13879,.F.);
#18307=ORIENTED_EDGE('',*,*,#13880,.F.);
#18308=ORIENTED_EDGE('',*,*,#13881,.F.);
#18309=ORIENTED_EDGE('',*,*,#13882,.F.);
#18310=ORIENTED_EDGE('',*,*,#13883,.F.);
#18311=ORIENTED_EDGE('',*,*,#13884,.F.);
#18312=ORIENTED_EDGE('',*,*,#13885,.F.);
#18313=ORIENTED_EDGE('',*,*,#13886,.F.);
#18314=ORIENTED_EDGE('',*,*,#13887,.F.);
#18315=ORIENTED_EDGE('',*,*,#13888,.F.);
#18316=ORIENTED_EDGE('',*,*,#13889,.F.);
#18317=ORIENTED_EDGE('',*,*,#13890,.F.);
#18318=ORIENTED_EDGE('',*,*,#13891,.F.);
#18319=ORIENTED_EDGE('',*,*,#13892,.F.);
#18320=ORIENTED_EDGE('',*,*,#13893,.F.);
#18321=ORIENTED_EDGE('',*,*,#13894,.F.);
#18322=ORIENTED_EDGE('',*,*,#13895,.F.);
#18323=ORIENTED_EDGE('',*,*,#13896,.F.);
#18324=ORIENTED_EDGE('',*,*,#13897,.F.);
#18325=ORIENTED_EDGE('',*,*,#13898,.F.);
#18326=ORIENTED_EDGE('',*,*,#13899,.F.);
#18327=ORIENTED_EDGE('',*,*,#13900,.F.);
#18328=ORIENTED_EDGE('',*,*,#13855,.T.);
#18329=ORIENTED_EDGE('',*,*,#13901,.T.);
#18330=ORIENTED_EDGE('',*,*,#13902,.F.);
#18331=ORIENTED_EDGE('',*,*,#13903,.F.);
#18332=ORIENTED_EDGE('',*,*,#13856,.T.);
#18333=ORIENTED_EDGE('',*,*,#13900,.T.);
#18334=ORIENTED_EDGE('',*,*,#13904,.F.);
#18335=ORIENTED_EDGE('',*,*,#13905,.F.);
#18336=ORIENTED_EDGE('',*,*,#13857,.T.);
#18337=ORIENTED_EDGE('',*,*,#13903,.T.);
#18338=ORIENTED_EDGE('',*,*,#13906,.F.);
#18339=ORIENTED_EDGE('',*,*,#13907,.F.);
#18340=ORIENTED_EDGE('',*,*,#13858,.T.);
#18341=ORIENTED_EDGE('',*,*,#13905,.T.);
#18342=ORIENTED_EDGE('',*,*,#13908,.F.);
#18343=ORIENTED_EDGE('',*,*,#13909,.F.);
#18344=ORIENTED_EDGE('',*,*,#13859,.T.);
#18345=ORIENTED_EDGE('',*,*,#13907,.T.);
#18346=ORIENTED_EDGE('',*,*,#13910,.F.);
#18347=ORIENTED_EDGE('',*,*,#13911,.F.);
#18348=ORIENTED_EDGE('',*,*,#13860,.T.);
#18349=ORIENTED_EDGE('',*,*,#13909,.T.);
#18350=ORIENTED_EDGE('',*,*,#13912,.F.);
#18351=ORIENTED_EDGE('',*,*,#13913,.F.);
#18352=ORIENTED_EDGE('',*,*,#13861,.T.);
#18353=ORIENTED_EDGE('',*,*,#13911,.T.);
#18354=ORIENTED_EDGE('',*,*,#13914,.F.);
#18355=ORIENTED_EDGE('',*,*,#13915,.F.);
#18356=ORIENTED_EDGE('',*,*,#13862,.T.);
#18357=ORIENTED_EDGE('',*,*,#13913,.T.);
#18358=ORIENTED_EDGE('',*,*,#13916,.F.);
#18359=ORIENTED_EDGE('',*,*,#13917,.F.);
#18360=ORIENTED_EDGE('',*,*,#13863,.T.);
#18361=ORIENTED_EDGE('',*,*,#13915,.T.);
#18362=ORIENTED_EDGE('',*,*,#13918,.F.);
#18363=ORIENTED_EDGE('',*,*,#13919,.F.);
#18364=ORIENTED_EDGE('',*,*,#13864,.T.);
#18365=ORIENTED_EDGE('',*,*,#13917,.T.);
#18366=ORIENTED_EDGE('',*,*,#13920,.F.);
#18367=ORIENTED_EDGE('',*,*,#13921,.F.);
#18368=ORIENTED_EDGE('',*,*,#13865,.T.);
#18369=ORIENTED_EDGE('',*,*,#13919,.T.);
#18370=ORIENTED_EDGE('',*,*,#13922,.F.);
#18371=ORIENTED_EDGE('',*,*,#13923,.F.);
#18372=ORIENTED_EDGE('',*,*,#13866,.T.);
#18373=ORIENTED_EDGE('',*,*,#13921,.T.);
#18374=ORIENTED_EDGE('',*,*,#13924,.F.);
#18375=ORIENTED_EDGE('',*,*,#13925,.F.);
#18376=ORIENTED_EDGE('',*,*,#13867,.T.);
#18377=ORIENTED_EDGE('',*,*,#13923,.T.);
#18378=ORIENTED_EDGE('',*,*,#13926,.F.);
#18379=ORIENTED_EDGE('',*,*,#13927,.F.);
#18380=ORIENTED_EDGE('',*,*,#13868,.T.);
#18381=ORIENTED_EDGE('',*,*,#13925,.T.);
#18382=ORIENTED_EDGE('',*,*,#13928,.F.);
#18383=ORIENTED_EDGE('',*,*,#13929,.F.);
#18384=ORIENTED_EDGE('',*,*,#13869,.T.);
#18385=ORIENTED_EDGE('',*,*,#13927,.T.);
#18386=ORIENTED_EDGE('',*,*,#13930,.F.);
#18387=ORIENTED_EDGE('',*,*,#13931,.F.);
#18388=ORIENTED_EDGE('',*,*,#13870,.T.);
#18389=ORIENTED_EDGE('',*,*,#13929,.T.);
#18390=ORIENTED_EDGE('',*,*,#13932,.F.);
#18391=ORIENTED_EDGE('',*,*,#13933,.F.);
#18392=ORIENTED_EDGE('',*,*,#13871,.T.);
#18393=ORIENTED_EDGE('',*,*,#13931,.T.);
#18394=ORIENTED_EDGE('',*,*,#13934,.F.);
#18395=ORIENTED_EDGE('',*,*,#13935,.F.);
#18396=ORIENTED_EDGE('',*,*,#13872,.T.);
#18397=ORIENTED_EDGE('',*,*,#13933,.T.);
#18398=ORIENTED_EDGE('',*,*,#13936,.F.);
#18399=ORIENTED_EDGE('',*,*,#13937,.F.);
#18400=ORIENTED_EDGE('',*,*,#13873,.T.);
#18401=ORIENTED_EDGE('',*,*,#13935,.T.);
#18402=ORIENTED_EDGE('',*,*,#13938,.F.);
#18403=ORIENTED_EDGE('',*,*,#13939,.F.);
#18404=ORIENTED_EDGE('',*,*,#13874,.T.);
#18405=ORIENTED_EDGE('',*,*,#13937,.T.);
#18406=ORIENTED_EDGE('',*,*,#13940,.F.);
#18407=ORIENTED_EDGE('',*,*,#13941,.F.);
#18408=ORIENTED_EDGE('',*,*,#13875,.T.);
#18409=ORIENTED_EDGE('',*,*,#13939,.T.);
#18410=ORIENTED_EDGE('',*,*,#13942,.F.);
#18411=ORIENTED_EDGE('',*,*,#13943,.F.);
#18412=ORIENTED_EDGE('',*,*,#13876,.T.);
#18413=ORIENTED_EDGE('',*,*,#13941,.T.);
#18414=ORIENTED_EDGE('',*,*,#13944,.F.);
#18415=ORIENTED_EDGE('',*,*,#13945,.F.);
#18416=ORIENTED_EDGE('',*,*,#13877,.T.);
#18417=ORIENTED_EDGE('',*,*,#13943,.T.);
#18418=ORIENTED_EDGE('',*,*,#13946,.F.);
#18419=ORIENTED_EDGE('',*,*,#13947,.F.);
#18420=ORIENTED_EDGE('',*,*,#13878,.T.);
#18421=ORIENTED_EDGE('',*,*,#13945,.T.);
#18422=ORIENTED_EDGE('',*,*,#13948,.F.);
#18423=ORIENTED_EDGE('',*,*,#13949,.F.);
#18424=ORIENTED_EDGE('',*,*,#13879,.T.);
#18425=ORIENTED_EDGE('',*,*,#13947,.T.);
#18426=ORIENTED_EDGE('',*,*,#13950,.F.);
#18427=ORIENTED_EDGE('',*,*,#13951,.F.);
#18428=ORIENTED_EDGE('',*,*,#13880,.T.);
#18429=ORIENTED_EDGE('',*,*,#13949,.T.);
#18430=ORIENTED_EDGE('',*,*,#13952,.F.);
#18431=ORIENTED_EDGE('',*,*,#13953,.F.);
#18432=ORIENTED_EDGE('',*,*,#13881,.T.);
#18433=ORIENTED_EDGE('',*,*,#13951,.T.);
#18434=ORIENTED_EDGE('',*,*,#13954,.F.);
#18435=ORIENTED_EDGE('',*,*,#13955,.F.);
#18436=ORIENTED_EDGE('',*,*,#13882,.T.);
#18437=ORIENTED_EDGE('',*,*,#13953,.T.);
#18438=ORIENTED_EDGE('',*,*,#13956,.F.);
#18439=ORIENTED_EDGE('',*,*,#13957,.F.);
#18440=ORIENTED_EDGE('',*,*,#13883,.T.);
#18441=ORIENTED_EDGE('',*,*,#13955,.T.);
#18442=ORIENTED_EDGE('',*,*,#13958,.F.);
#18443=ORIENTED_EDGE('',*,*,#13959,.F.);
#18444=ORIENTED_EDGE('',*,*,#13884,.T.);
#18445=ORIENTED_EDGE('',*,*,#13957,.T.);
#18446=ORIENTED_EDGE('',*,*,#13960,.F.);
#18447=ORIENTED_EDGE('',*,*,#13961,.F.);
#18448=ORIENTED_EDGE('',*,*,#13885,.T.);
#18449=ORIENTED_EDGE('',*,*,#13959,.T.);
#18450=ORIENTED_EDGE('',*,*,#13962,.F.);
#18451=ORIENTED_EDGE('',*,*,#13963,.F.);
#18452=ORIENTED_EDGE('',*,*,#13886,.T.);
#18453=ORIENTED_EDGE('',*,*,#13961,.T.);
#18454=ORIENTED_EDGE('',*,*,#13964,.F.);
#18455=ORIENTED_EDGE('',*,*,#13965,.F.);
#18456=ORIENTED_EDGE('',*,*,#13887,.T.);
#18457=ORIENTED_EDGE('',*,*,#13963,.T.);
#18458=ORIENTED_EDGE('',*,*,#13966,.F.);
#18459=ORIENTED_EDGE('',*,*,#13967,.F.);
#18460=ORIENTED_EDGE('',*,*,#13888,.T.);
#18461=ORIENTED_EDGE('',*,*,#13965,.T.);
#18462=ORIENTED_EDGE('',*,*,#13968,.F.);
#18463=ORIENTED_EDGE('',*,*,#13969,.F.);
#18464=ORIENTED_EDGE('',*,*,#13889,.T.);
#18465=ORIENTED_EDGE('',*,*,#13967,.T.);
#18466=ORIENTED_EDGE('',*,*,#13970,.F.);
#18467=ORIENTED_EDGE('',*,*,#13971,.F.);
#18468=ORIENTED_EDGE('',*,*,#13890,.T.);
#18469=ORIENTED_EDGE('',*,*,#13969,.T.);
#18470=ORIENTED_EDGE('',*,*,#13972,.F.);
#18471=ORIENTED_EDGE('',*,*,#13973,.F.);
#18472=ORIENTED_EDGE('',*,*,#13891,.T.);
#18473=ORIENTED_EDGE('',*,*,#13971,.T.);
#18474=ORIENTED_EDGE('',*,*,#13974,.F.);
#18475=ORIENTED_EDGE('',*,*,#13975,.F.);
#18476=ORIENTED_EDGE('',*,*,#13892,.T.);
#18477=ORIENTED_EDGE('',*,*,#13973,.T.);
#18478=ORIENTED_EDGE('',*,*,#13976,.F.);
#18479=ORIENTED_EDGE('',*,*,#13977,.F.);
#18480=ORIENTED_EDGE('',*,*,#13893,.T.);
#18481=ORIENTED_EDGE('',*,*,#13975,.T.);
#18482=ORIENTED_EDGE('',*,*,#13978,.F.);
#18483=ORIENTED_EDGE('',*,*,#13979,.F.);
#18484=ORIENTED_EDGE('',*,*,#13894,.T.);
#18485=ORIENTED_EDGE('',*,*,#13977,.T.);
#18486=ORIENTED_EDGE('',*,*,#13980,.F.);
#18487=ORIENTED_EDGE('',*,*,#13981,.F.);
#18488=ORIENTED_EDGE('',*,*,#13895,.T.);
#18489=ORIENTED_EDGE('',*,*,#13979,.T.);
#18490=ORIENTED_EDGE('',*,*,#13982,.F.);
#18491=ORIENTED_EDGE('',*,*,#13983,.F.);
#18492=ORIENTED_EDGE('',*,*,#13896,.T.);
#18493=ORIENTED_EDGE('',*,*,#13981,.T.);
#18494=ORIENTED_EDGE('',*,*,#13984,.F.);
#18495=ORIENTED_EDGE('',*,*,#13985,.F.);
#18496=ORIENTED_EDGE('',*,*,#13897,.T.);
#18497=ORIENTED_EDGE('',*,*,#13983,.T.);
#18498=ORIENTED_EDGE('',*,*,#13986,.F.);
#18499=ORIENTED_EDGE('',*,*,#13901,.F.);
#18500=ORIENTED_EDGE('',*,*,#13898,.T.);
#18501=ORIENTED_EDGE('',*,*,#13985,.T.);
#18502=ORIENTED_EDGE('',*,*,#13675,.T.);
#18503=ORIENTED_EDGE('',*,*,#13680,.F.);
#18504=ORIENTED_EDGE('',*,*,#13987,.T.);
#18505=ORIENTED_EDGE('',*,*,#13988,.T.);
#18506=ORIENTED_EDGE('',*,*,#13989,.T.);
#18507=ORIENTED_EDGE('',*,*,#13990,.F.);
#18508=ORIENTED_EDGE('',*,*,#13991,.F.);
#18509=ORIENTED_EDGE('',*,*,#13992,.F.);
#18510=ORIENTED_EDGE('',*,*,#13993,.F.);
#18511=ORIENTED_EDGE('',*,*,#13994,.F.);
#18512=ORIENTED_EDGE('',*,*,#13995,.F.);
#18513=ORIENTED_EDGE('',*,*,#13996,.F.);
#18514=ORIENTED_EDGE('',*,*,#13997,.F.);
#18515=ORIENTED_EDGE('',*,*,#13998,.T.);
#18516=ORIENTED_EDGE('',*,*,#13999,.T.);
#18517=ORIENTED_EDGE('',*,*,#14000,.T.);
#18518=ORIENTED_EDGE('',*,*,#14001,.T.);
#18519=ORIENTED_EDGE('',*,*,#14002,.T.);
#18520=ORIENTED_EDGE('',*,*,#14003,.T.);
#18521=ORIENTED_EDGE('',*,*,#14004,.T.);
#18522=ORIENTED_EDGE('',*,*,#14005,.T.);
#18523=ORIENTED_EDGE('',*,*,#14006,.T.);
#18524=ORIENTED_EDGE('',*,*,#14007,.T.);
#18525=ORIENTED_EDGE('',*,*,#14008,.T.);
#18526=ORIENTED_EDGE('',*,*,#14009,.T.);
#18527=ORIENTED_EDGE('',*,*,#14010,.T.);
#18528=ORIENTED_EDGE('',*,*,#14011,.T.);
#18529=ORIENTED_EDGE('',*,*,#14012,.T.);
#18530=ORIENTED_EDGE('',*,*,#14013,.T.);
#18531=ORIENTED_EDGE('',*,*,#14014,.T.);
#18532=ORIENTED_EDGE('',*,*,#14015,.T.);
#18533=ORIENTED_EDGE('',*,*,#14016,.T.);
#18534=ORIENTED_EDGE('',*,*,#14017,.T.);
#18535=ORIENTED_EDGE('',*,*,#14018,.T.);
#18536=ORIENTED_EDGE('',*,*,#14019,.T.);
#18537=ORIENTED_EDGE('',*,*,#14020,.T.);
#18538=ORIENTED_EDGE('',*,*,#14021,.T.);
#18539=ORIENTED_EDGE('',*,*,#14022,.T.);
#18540=ORIENTED_EDGE('',*,*,#14023,.T.);
#18541=ORIENTED_EDGE('',*,*,#14024,.T.);
#18542=ORIENTED_EDGE('',*,*,#14025,.T.);
#18543=ORIENTED_EDGE('',*,*,#14026,.T.);
#18544=ORIENTED_EDGE('',*,*,#14027,.T.);
#18545=ORIENTED_EDGE('',*,*,#14028,.T.);
#18546=ORIENTED_EDGE('',*,*,#14029,.T.);
#18547=ORIENTED_EDGE('',*,*,#14030,.T.);
#18548=ORIENTED_EDGE('',*,*,#14031,.T.);
#18549=ORIENTED_EDGE('',*,*,#14032,.T.);
#18550=ORIENTED_EDGE('',*,*,#14033,.T.);
#18551=ORIENTED_EDGE('',*,*,#14034,.T.);
#18552=ORIENTED_EDGE('',*,*,#14035,.F.);
#18553=ORIENTED_EDGE('',*,*,#14036,.F.);
#18554=ORIENTED_EDGE('',*,*,#14037,.F.);
#18555=ORIENTED_EDGE('',*,*,#14038,.T.);
#18556=ORIENTED_EDGE('',*,*,#13677,.F.);
#18557=ORIENTED_EDGE('',*,*,#13989,.F.);
#18558=ORIENTED_EDGE('',*,*,#14039,.T.);
#18559=ORIENTED_EDGE('',*,*,#14040,.T.);
#18560=ORIENTED_EDGE('',*,*,#14041,.F.);
#18561=ORIENTED_EDGE('',*,*,#13987,.F.);
#18562=ORIENTED_EDGE('',*,*,#13679,.T.);
#18563=ORIENTED_EDGE('',*,*,#14042,.T.);
#18564=ORIENTED_EDGE('',*,*,#14039,.F.);
#18565=ORIENTED_EDGE('',*,*,#13988,.F.);
#18566=ORIENTED_EDGE('',*,*,#14041,.T.);
#18567=ORIENTED_EDGE('',*,*,#13667,.T.);
#18568=ORIENTED_EDGE('',*,*,#13669,.F.);
#18569=ORIENTED_EDGE('',*,*,#14043,.T.);
#18570=ORIENTED_EDGE('',*,*,#14044,.T.);
#18571=ORIENTED_EDGE('',*,*,#14045,.T.);
#18572=ORIENTED_EDGE('',*,*,#14046,.T.);
#18573=ORIENTED_EDGE('',*,*,#14047,.T.);
#18574=ORIENTED_EDGE('',*,*,#14034,.F.);
#18575=ORIENTED_EDGE('',*,*,#14048,.F.);
#18576=ORIENTED_EDGE('',*,*,#14047,.F.);
#18577=ORIENTED_EDGE('',*,*,#14049,.T.);
#18578=ORIENTED_EDGE('',*,*,#14050,.T.);
#18579=ORIENTED_EDGE('',*,*,#14035,.T.);
#18580=ORIENTED_EDGE('',*,*,#14050,.F.);
#18581=ORIENTED_EDGE('',*,*,#14051,.T.);
#18582=ORIENTED_EDGE('',*,*,#14052,.T.);
#18583=ORIENTED_EDGE('',*,*,#14036,.T.);
#18584=ORIENTED_EDGE('',*,*,#14052,.F.);
#18585=ORIENTED_EDGE('',*,*,#14053,.T.);
#18586=ORIENTED_EDGE('',*,*,#14054,.T.);
#18587=ORIENTED_EDGE('',*,*,#14037,.T.);
#18588=ORIENTED_EDGE('',*,*,#14055,.F.);
#18589=ORIENTED_EDGE('',*,*,#14056,.T.);
#18590=ORIENTED_EDGE('',*,*,#13990,.T.);
#18591=ORIENTED_EDGE('',*,*,#14054,.F.);
#18592=ORIENTED_EDGE('',*,*,#14057,.T.);
#18593=ORIENTED_EDGE('',*,*,#14058,.T.);
#18594=ORIENTED_EDGE('',*,*,#13994,.T.);
#18595=ORIENTED_EDGE('',*,*,#14059,.F.);
#18596=ORIENTED_EDGE('',*,*,#14058,.F.);
#18597=ORIENTED_EDGE('',*,*,#14060,.T.);
#18598=ORIENTED_EDGE('',*,*,#14061,.T.);
#18599=ORIENTED_EDGE('',*,*,#13995,.T.);
#18600=ORIENTED_EDGE('',*,*,#14061,.F.);
#18601=ORIENTED_EDGE('',*,*,#14062,.T.);
#18602=ORIENTED_EDGE('',*,*,#14063,.T.);
#18603=ORIENTED_EDGE('',*,*,#13996,.T.);
#18604=ORIENTED_EDGE('',*,*,#14063,.F.);
#18605=ORIENTED_EDGE('',*,*,#14064,.T.);
#18606=ORIENTED_EDGE('',*,*,#14065,.T.);
#18607=ORIENTED_EDGE('',*,*,#13997,.T.);
#18608=ORIENTED_EDGE('',*,*,#14066,.T.);
#18609=ORIENTED_EDGE('',*,*,#14067,.T.);
#18610=ORIENTED_EDGE('',*,*,#13998,.F.);
#18611=ORIENTED_EDGE('',*,*,#14065,.F.);
#18612=ORIENTED_EDGE('',*,*,#14068,.T.);
#18613=ORIENTED_EDGE('',*,*,#14069,.T.);
#18614=ORIENTED_EDGE('',*,*,#13999,.F.);
#18615=ORIENTED_EDGE('',*,*,#14067,.F.);
#18616=ORIENTED_EDGE('',*,*,#14070,.T.);
#18617=ORIENTED_EDGE('',*,*,#14071,.F.);
#18618=ORIENTED_EDGE('',*,*,#14000,.F.);
#18619=ORIENTED_EDGE('',*,*,#14069,.F.);
#18620=ORIENTED_EDGE('',*,*,#14072,.T.);
#18621=ORIENTED_EDGE('',*,*,#14073,.T.);
#18622=ORIENTED_EDGE('',*,*,#14001,.F.);
#18623=ORIENTED_EDGE('',*,*,#14071,.T.);
#18624=ORIENTED_EDGE('',*,*,#14074,.T.);
#18625=ORIENTED_EDGE('',*,*,#14075,.F.);
#18626=ORIENTED_EDGE('',*,*,#14002,.F.);
#18627=ORIENTED_EDGE('',*,*,#14073,.F.);
#18628=ORIENTED_EDGE('',*,*,#14076,.T.);
#18629=ORIENTED_EDGE('',*,*,#14077,.T.);
#18630=ORIENTED_EDGE('',*,*,#14003,.F.);
#18631=ORIENTED_EDGE('',*,*,#14075,.T.);
#18632=ORIENTED_EDGE('',*,*,#14077,.F.);
#18633=ORIENTED_EDGE('',*,*,#14078,.T.);
#18634=ORIENTED_EDGE('',*,*,#14079,.F.);
#18635=ORIENTED_EDGE('',*,*,#14004,.F.);
#18636=ORIENTED_EDGE('',*,*,#14080,.T.);
#18637=ORIENTED_EDGE('',*,*,#14081,.T.);
#18638=ORIENTED_EDGE('',*,*,#14005,.F.);
#18639=ORIENTED_EDGE('',*,*,#14079,.T.);
#18640=ORIENTED_EDGE('',*,*,#14081,.F.);
#18641=ORIENTED_EDGE('',*,*,#14082,.T.);
#18642=ORIENTED_EDGE('',*,*,#14083,.F.);
#18643=ORIENTED_EDGE('',*,*,#14006,.F.);
#18644=ORIENTED_EDGE('',*,*,#14084,.T.);
#18645=ORIENTED_EDGE('',*,*,#14085,.T.);
#18646=ORIENTED_EDGE('',*,*,#14007,.F.);
#18647=ORIENTED_EDGE('',*,*,#14083,.T.);
#18648=ORIENTED_EDGE('',*,*,#14085,.F.);
#18649=ORIENTED_EDGE('',*,*,#14086,.T.);
#18650=ORIENTED_EDGE('',*,*,#14087,.F.);
#18651=ORIENTED_EDGE('',*,*,#14008,.F.);
#18652=ORIENTED_EDGE('',*,*,#14088,.T.);
#18653=ORIENTED_EDGE('',*,*,#14089,.T.);
#18654=ORIENTED_EDGE('',*,*,#14009,.F.);
#18655=ORIENTED_EDGE('',*,*,#14087,.T.);
#18656=ORIENTED_EDGE('',*,*,#14089,.F.);
#18657=ORIENTED_EDGE('',*,*,#14090,.T.);
#18658=ORIENTED_EDGE('',*,*,#14091,.F.);
#18659=ORIENTED_EDGE('',*,*,#14010,.F.);
#18660=ORIENTED_EDGE('',*,*,#14092,.T.);
#18661=ORIENTED_EDGE('',*,*,#14093,.T.);
#18662=ORIENTED_EDGE('',*,*,#14011,.F.);
#18663=ORIENTED_EDGE('',*,*,#14091,.T.);
#18664=ORIENTED_EDGE('',*,*,#14093,.F.);
#18665=ORIENTED_EDGE('',*,*,#14094,.T.);
#18666=ORIENTED_EDGE('',*,*,#14095,.F.);
#18667=ORIENTED_EDGE('',*,*,#14012,.F.);
#18668=ORIENTED_EDGE('',*,*,#14096,.T.);
#18669=ORIENTED_EDGE('',*,*,#14097,.T.);
#18670=ORIENTED_EDGE('',*,*,#14013,.F.);
#18671=ORIENTED_EDGE('',*,*,#14095,.T.);
#18672=ORIENTED_EDGE('',*,*,#14097,.F.);
#18673=ORIENTED_EDGE('',*,*,#14098,.T.);
#18674=ORIENTED_EDGE('',*,*,#14099,.F.);
#18675=ORIENTED_EDGE('',*,*,#14014,.F.);
#18676=ORIENTED_EDGE('',*,*,#14100,.T.);
#18677=ORIENTED_EDGE('',*,*,#14101,.T.);
#18678=ORIENTED_EDGE('',*,*,#14015,.F.);
#18679=ORIENTED_EDGE('',*,*,#14099,.T.);
#18680=ORIENTED_EDGE('',*,*,#14102,.T.);
#18681=ORIENTED_EDGE('',*,*,#14103,.T.);
#18682=ORIENTED_EDGE('',*,*,#14016,.F.);
#18683=ORIENTED_EDGE('',*,*,#14101,.F.);
#18684=ORIENTED_EDGE('',*,*,#14104,.T.);
#18685=ORIENTED_EDGE('',*,*,#14105,.T.);
#18686=ORIENTED_EDGE('',*,*,#14017,.F.);
#18687=ORIENTED_EDGE('',*,*,#14103,.F.);
#18688=ORIENTED_EDGE('',*,*,#14105,.F.);
#18689=ORIENTED_EDGE('',*,*,#14106,.T.);
#18690=ORIENTED_EDGE('',*,*,#14107,.F.);
#18691=ORIENTED_EDGE('',*,*,#14018,.F.);
#18692=ORIENTED_EDGE('',*,*,#14108,.T.);
#18693=ORIENTED_EDGE('',*,*,#14109,.T.);
#18694=ORIENTED_EDGE('',*,*,#14019,.F.);
#18695=ORIENTED_EDGE('',*,*,#14107,.T.);
#18696=ORIENTED_EDGE('',*,*,#14109,.F.);
#18697=ORIENTED_EDGE('',*,*,#14110,.T.);
#18698=ORIENTED_EDGE('',*,*,#14111,.F.);
#18699=ORIENTED_EDGE('',*,*,#14020,.F.);
#18700=ORIENTED_EDGE('',*,*,#14112,.T.);
#18701=ORIENTED_EDGE('',*,*,#14113,.T.);
#18702=ORIENTED_EDGE('',*,*,#14021,.F.);
#18703=ORIENTED_EDGE('',*,*,#14111,.T.);
#18704=ORIENTED_EDGE('',*,*,#14113,.F.);
#18705=ORIENTED_EDGE('',*,*,#14114,.T.);
#18706=ORIENTED_EDGE('',*,*,#14115,.F.);
#18707=ORIENTED_EDGE('',*,*,#14022,.F.);
#18708=ORIENTED_EDGE('',*,*,#14116,.T.);
#18709=ORIENTED_EDGE('',*,*,#14117,.T.);
#18710=ORIENTED_EDGE('',*,*,#14023,.F.);
#18711=ORIENTED_EDGE('',*,*,#14115,.T.);
#18712=ORIENTED_EDGE('',*,*,#14117,.F.);
#18713=ORIENTED_EDGE('',*,*,#14118,.T.);
#18714=ORIENTED_EDGE('',*,*,#14119,.F.);
#18715=ORIENTED_EDGE('',*,*,#14024,.F.);
#18716=ORIENTED_EDGE('',*,*,#14120,.T.);
#18717=ORIENTED_EDGE('',*,*,#14121,.T.);
#18718=ORIENTED_EDGE('',*,*,#14025,.F.);
#18719=ORIENTED_EDGE('',*,*,#14119,.T.);
#18720=ORIENTED_EDGE('',*,*,#14121,.F.);
#18721=ORIENTED_EDGE('',*,*,#14122,.T.);
#18722=ORIENTED_EDGE('',*,*,#14123,.F.);
#18723=ORIENTED_EDGE('',*,*,#14026,.F.);
#18724=ORIENTED_EDGE('',*,*,#14124,.T.);
#18725=ORIENTED_EDGE('',*,*,#14125,.T.);
#18726=ORIENTED_EDGE('',*,*,#14027,.F.);
#18727=ORIENTED_EDGE('',*,*,#14123,.T.);
#18728=ORIENTED_EDGE('',*,*,#14125,.F.);
#18729=ORIENTED_EDGE('',*,*,#14126,.T.);
#18730=ORIENTED_EDGE('',*,*,#14127,.F.);
#18731=ORIENTED_EDGE('',*,*,#14028,.F.);
#18732=ORIENTED_EDGE('',*,*,#14128,.T.);
#18733=ORIENTED_EDGE('',*,*,#14129,.T.);
#18734=ORIENTED_EDGE('',*,*,#14029,.F.);
#18735=ORIENTED_EDGE('',*,*,#14127,.T.);
#18736=ORIENTED_EDGE('',*,*,#14130,.T.);
#18737=ORIENTED_EDGE('',*,*,#14131,.F.);
#18738=ORIENTED_EDGE('',*,*,#14030,.F.);
#18739=ORIENTED_EDGE('',*,*,#14129,.F.);
#18740=ORIENTED_EDGE('',*,*,#14132,.T.);
#18741=ORIENTED_EDGE('',*,*,#14133,.T.);
#18742=ORIENTED_EDGE('',*,*,#14031,.F.);
#18743=ORIENTED_EDGE('',*,*,#14131,.T.);
#18744=ORIENTED_EDGE('',*,*,#14134,.T.);
#18745=ORIENTED_EDGE('',*,*,#14135,.F.);
#18746=ORIENTED_EDGE('',*,*,#14032,.F.);
#18747=ORIENTED_EDGE('',*,*,#14133,.F.);
#18748=ORIENTED_EDGE('',*,*,#14136,.T.);
#18749=ORIENTED_EDGE('',*,*,#14048,.T.);
#18750=ORIENTED_EDGE('',*,*,#14033,.F.);
#18751=ORIENTED_EDGE('',*,*,#14135,.T.);
#18752=ORIENTED_EDGE('',*,*,#13664,.T.);
#18753=ORIENTED_EDGE('',*,*,#14042,.F.);
#18754=ORIENTED_EDGE('',*,*,#14040,.F.);
#18755=ORIENTED_EDGE('',*,*,#13678,.F.);
#18756=ORIENTED_EDGE('',*,*,#14038,.F.);
#18757=ORIENTED_EDGE('',*,*,#14137,.T.);
#18758=ORIENTED_EDGE('',*,*,#14138,.T.);
#18759=ORIENTED_EDGE('',*,*,#14139,.T.);
#18760=ORIENTED_EDGE('',*,*,#14140,.T.);
#18761=ORIENTED_EDGE('',*,*,#14141,.T.);
#18762=ORIENTED_EDGE('',*,*,#14142,.T.);
#18763=ORIENTED_EDGE('',*,*,#14143,.T.);
#18764=ORIENTED_EDGE('',*,*,#14144,.F.);
#18765=ORIENTED_EDGE('',*,*,#14145,.T.);
#18766=ORIENTED_EDGE('',*,*,#13670,.F.);
#18767=ORIENTED_EDGE('',*,*,#14045,.F.);
#18768=ORIENTED_EDGE('',*,*,#14146,.T.);
#18769=ORIENTED_EDGE('',*,*,#14147,.T.);
#18770=ORIENTED_EDGE('',*,*,#14148,.F.);
#18771=ORIENTED_EDGE('',*,*,#14043,.F.);
#18772=ORIENTED_EDGE('',*,*,#13672,.T.);
#18773=ORIENTED_EDGE('',*,*,#14149,.T.);
#18774=ORIENTED_EDGE('',*,*,#14146,.F.);
#18775=ORIENTED_EDGE('',*,*,#14044,.F.);
#18776=ORIENTED_EDGE('',*,*,#14148,.T.);
#18777=ORIENTED_EDGE('',*,*,#14150,.F.);
#18778=ORIENTED_EDGE('',*,*,#14137,.F.);
#18779=ORIENTED_EDGE('',*,*,#14151,.F.);
#18780=ORIENTED_EDGE('',*,*,#14152,.F.);
#18781=ORIENTED_EDGE('',*,*,#14150,.T.);
#18782=ORIENTED_EDGE('',*,*,#14153,.F.);
#18783=ORIENTED_EDGE('',*,*,#14154,.T.);
#18784=ORIENTED_EDGE('',*,*,#14155,.T.);
#18785=ORIENTED_EDGE('',*,*,#14156,.F.);
#18786=ORIENTED_EDGE('',*,*,#14138,.F.);
#18787=ORIENTED_EDGE('',*,*,#14157,.T.);
#18788=ORIENTED_EDGE('',*,*,#14158,.T.);
#18789=ORIENTED_EDGE('',*,*,#14159,.F.);
#18790=ORIENTED_EDGE('',*,*,#14154,.F.);
#18791=ORIENTED_EDGE('',*,*,#14160,.T.);
#18792=ORIENTED_EDGE('',*,*,#14161,.T.);
#18793=ORIENTED_EDGE('',*,*,#14162,.T.);
#18794=ORIENTED_EDGE('',*,*,#14163,.F.);
#18795=ORIENTED_EDGE('',*,*,#14163,.T.);
#18796=ORIENTED_EDGE('',*,*,#14164,.F.);
#18797=ORIENTED_EDGE('',*,*,#14165,.T.);
#18798=ORIENTED_EDGE('',*,*,#14142,.F.);
#18799=ORIENTED_EDGE('',*,*,#14166,.F.);
#18800=ORIENTED_EDGE('',*,*,#14167,.T.);
#18801=ORIENTED_EDGE('',*,*,#14165,.F.);
#18802=ORIENTED_EDGE('',*,*,#14168,.F.);
#18803=ORIENTED_EDGE('',*,*,#14169,.T.);
#18804=ORIENTED_EDGE('',*,*,#14143,.F.);
#18805=ORIENTED_EDGE('',*,*,#14136,.F.);
#18806=ORIENTED_EDGE('',*,*,#14134,.F.);
#18807=ORIENTED_EDGE('',*,*,#14132,.F.);
#18808=ORIENTED_EDGE('',*,*,#14130,.F.);
#18809=ORIENTED_EDGE('',*,*,#14128,.F.);
#18810=ORIENTED_EDGE('',*,*,#14126,.F.);
#18811=ORIENTED_EDGE('',*,*,#14124,.F.);
#18812=ORIENTED_EDGE('',*,*,#14122,.F.);
#18813=ORIENTED_EDGE('',*,*,#14120,.F.);
#18814=ORIENTED_EDGE('',*,*,#14118,.F.);
#18815=ORIENTED_EDGE('',*,*,#14116,.F.);
#18816=ORIENTED_EDGE('',*,*,#14114,.F.);
#18817=ORIENTED_EDGE('',*,*,#14112,.F.);
#18818=ORIENTED_EDGE('',*,*,#14110,.F.);
#18819=ORIENTED_EDGE('',*,*,#14108,.F.);
#18820=ORIENTED_EDGE('',*,*,#14106,.F.);
#18821=ORIENTED_EDGE('',*,*,#14104,.F.);
#18822=ORIENTED_EDGE('',*,*,#14102,.F.);
#18823=ORIENTED_EDGE('',*,*,#14100,.F.);
#18824=ORIENTED_EDGE('',*,*,#14098,.F.);
#18825=ORIENTED_EDGE('',*,*,#14096,.F.);
#18826=ORIENTED_EDGE('',*,*,#14094,.F.);
#18827=ORIENTED_EDGE('',*,*,#14092,.F.);
#18828=ORIENTED_EDGE('',*,*,#14090,.F.);
#18829=ORIENTED_EDGE('',*,*,#14088,.F.);
#18830=ORIENTED_EDGE('',*,*,#14086,.F.);
#18831=ORIENTED_EDGE('',*,*,#14084,.F.);
#18832=ORIENTED_EDGE('',*,*,#14082,.F.);
#18833=ORIENTED_EDGE('',*,*,#14080,.F.);
#18834=ORIENTED_EDGE('',*,*,#14078,.F.);
#18835=ORIENTED_EDGE('',*,*,#14076,.F.);
#18836=ORIENTED_EDGE('',*,*,#14074,.F.);
#18837=ORIENTED_EDGE('',*,*,#14072,.F.);
#18838=ORIENTED_EDGE('',*,*,#14070,.F.);
#18839=ORIENTED_EDGE('',*,*,#14068,.F.);
#18840=ORIENTED_EDGE('',*,*,#14066,.F.);
#18841=ORIENTED_EDGE('',*,*,#14064,.F.);
#18842=ORIENTED_EDGE('',*,*,#14062,.F.);
#18843=ORIENTED_EDGE('',*,*,#14060,.F.);
#18844=ORIENTED_EDGE('',*,*,#14057,.F.);
#18845=ORIENTED_EDGE('',*,*,#14053,.F.);
#18846=ORIENTED_EDGE('',*,*,#14051,.F.);
#18847=ORIENTED_EDGE('',*,*,#14049,.F.);
#18848=ORIENTED_EDGE('',*,*,#14046,.F.);
#18849=ORIENTED_EDGE('',*,*,#14170,.T.);
#18850=ORIENTED_EDGE('',*,*,#14171,.T.);
#18851=ORIENTED_EDGE('',*,*,#14172,.T.);
#18852=ORIENTED_EDGE('',*,*,#14173,.T.);
#18853=ORIENTED_EDGE('',*,*,#14174,.T.);
#18854=ORIENTED_EDGE('',*,*,#14175,.T.);
#18855=ORIENTED_EDGE('',*,*,#14176,.T.);
#18856=ORIENTED_EDGE('',*,*,#14177,.T.);
#18857=ORIENTED_EDGE('',*,*,#14178,.T.);
#18858=ORIENTED_EDGE('',*,*,#14179,.T.);
#18859=ORIENTED_EDGE('',*,*,#14180,.T.);
#18860=ORIENTED_EDGE('',*,*,#14181,.T.);
#18861=ORIENTED_EDGE('',*,*,#14182,.T.);
#18862=ORIENTED_EDGE('',*,*,#14183,.T.);
#18863=ORIENTED_EDGE('',*,*,#14184,.T.);
#18864=ORIENTED_EDGE('',*,*,#14185,.T.);
#18865=ORIENTED_EDGE('',*,*,#14186,.T.);
#18866=ORIENTED_EDGE('',*,*,#14187,.T.);
#18867=ORIENTED_EDGE('',*,*,#14188,.T.);
#18868=ORIENTED_EDGE('',*,*,#14189,.T.);
#18869=ORIENTED_EDGE('',*,*,#14190,.T.);
#18870=ORIENTED_EDGE('',*,*,#14191,.T.);
#18871=ORIENTED_EDGE('',*,*,#14192,.T.);
#18872=ORIENTED_EDGE('',*,*,#14193,.T.);
#18873=ORIENTED_EDGE('',*,*,#14194,.T.);
#18874=ORIENTED_EDGE('',*,*,#14195,.T.);
#18875=ORIENTED_EDGE('',*,*,#14196,.T.);
#18876=ORIENTED_EDGE('',*,*,#14197,.T.);
#18877=ORIENTED_EDGE('',*,*,#14198,.T.);
#18878=ORIENTED_EDGE('',*,*,#14199,.T.);
#18879=ORIENTED_EDGE('',*,*,#14200,.T.);
#18880=ORIENTED_EDGE('',*,*,#14201,.T.);
#18881=ORIENTED_EDGE('',*,*,#14202,.T.);
#18882=ORIENTED_EDGE('',*,*,#14203,.T.);
#18883=ORIENTED_EDGE('',*,*,#14204,.T.);
#18884=ORIENTED_EDGE('',*,*,#14205,.T.);
#18885=ORIENTED_EDGE('',*,*,#14206,.T.);
#18886=ORIENTED_EDGE('',*,*,#14207,.T.);
#18887=ORIENTED_EDGE('',*,*,#14208,.T.);
#18888=ORIENTED_EDGE('',*,*,#14209,.T.);
#18889=ORIENTED_EDGE('',*,*,#14210,.T.);
#18890=ORIENTED_EDGE('',*,*,#14211,.T.);
#18891=ORIENTED_EDGE('',*,*,#14212,.T.);
#18892=ORIENTED_EDGE('',*,*,#14213,.T.);
#18893=ORIENTED_EDGE('',*,*,#14214,.F.);
#18894=ORIENTED_EDGE('',*,*,#14166,.T.);
#18895=ORIENTED_EDGE('',*,*,#14141,.F.);
#18896=ORIENTED_EDGE('',*,*,#14215,.F.);
#18897=ORIENTED_EDGE('',*,*,#14139,.F.);
#18898=ORIENTED_EDGE('',*,*,#14156,.T.);
#18899=ORIENTED_EDGE('',*,*,#14216,.F.);
#18900=ORIENTED_EDGE('',*,*,#14217,.T.);
#18901=ORIENTED_EDGE('',*,*,#14218,.T.);
#18902=ORIENTED_EDGE('',*,*,#14219,.F.);
#18903=ORIENTED_EDGE('',*,*,#14151,.T.);
#18904=ORIENTED_EDGE('',*,*,#14140,.F.);
#18905=ORIENTED_EDGE('',*,*,#14217,.F.);
#18906=ORIENTED_EDGE('',*,*,#14220,.T.);
#18907=ORIENTED_EDGE('',*,*,#14221,.T.);
#18908=ORIENTED_EDGE('',*,*,#14222,.T.);
#18909=ORIENTED_EDGE('',*,*,#14223,.T.);
#18910=ORIENTED_EDGE('',*,*,#14218,.F.);
#18911=ORIENTED_EDGE('',*,*,#14224,.T.);
#18912=ORIENTED_EDGE('',*,*,#14215,.T.);
#18913=ORIENTED_EDGE('',*,*,#14144,.T.);
#18914=ORIENTED_EDGE('',*,*,#14169,.F.);
#18915=ORIENTED_EDGE('',*,*,#14225,.T.);
#18916=ORIENTED_EDGE('',*,*,#14226,.T.);
#18917=ORIENTED_EDGE('',*,*,#14227,.T.);
#18918=ORIENTED_EDGE('',*,*,#14228,.T.);
#18919=ORIENTED_EDGE('',*,*,#14229,.F.);
#18920=ORIENTED_EDGE('',*,*,#14226,.F.);
#18921=ORIENTED_EDGE('',*,*,#13641,.T.);
#18922=ORIENTED_EDGE('',*,*,#14149,.F.);
#18923=ORIENTED_EDGE('',*,*,#14147,.F.);
#18924=ORIENTED_EDGE('',*,*,#13671,.F.);
#18925=ORIENTED_EDGE('',*,*,#14145,.F.);
#18926=ORIENTED_EDGE('',*,*,#14230,.F.);
#18927=ORIENTED_EDGE('',*,*,#13706,.T.);
#18928=ORIENTED_EDGE('',*,*,#14231,.F.);
#18929=ORIENTED_EDGE('',*,*,#14157,.F.);
#18930=ORIENTED_EDGE('',*,*,#14153,.T.);
#18931=ORIENTED_EDGE('',*,*,#14152,.T.);
#18932=ORIENTED_EDGE('',*,*,#14219,.T.);
#18933=ORIENTED_EDGE('',*,*,#14223,.F.);
#18934=ORIENTED_EDGE('',*,*,#14232,.T.);
#18935=ORIENTED_EDGE('',*,*,#14160,.F.);
#18936=ORIENTED_EDGE('',*,*,#14167,.F.);
#18937=ORIENTED_EDGE('',*,*,#14233,.F.);
#18938=ORIENTED_EDGE('',*,*,#14234,.T.);
#18939=ORIENTED_EDGE('',*,*,#14235,.F.);
#18940=ORIENTED_EDGE('',*,*,#13649,.T.);
#18941=ORIENTED_EDGE('',*,*,#14236,.T.);
#18942=ORIENTED_EDGE('',*,*,#14237,.T.);
#18943=ORIENTED_EDGE('',*,*,#14235,.T.);
#18944=ORIENTED_EDGE('',*,*,#14238,.T.);
#18945=ORIENTED_EDGE('',*,*,#14239,.F.);
#18946=ORIENTED_EDGE('',*,*,#13710,.T.);
#18947=ORIENTED_EDGE('',*,*,#14240,.F.);
#18948=ORIENTED_EDGE('',*,*,#14241,.F.);
#18949=ORIENTED_EDGE('',*,*,#14242,.F.);
#18950=ORIENTED_EDGE('',*,*,#14243,.T.);
#18951=ORIENTED_EDGE('',*,*,#14241,.T.);
#18952=ORIENTED_EDGE('',*,*,#14244,.T.);
#18953=ORIENTED_EDGE('',*,*,#14245,.T.);
#18954=ORIENTED_EDGE('',*,*,#14246,.F.);
#18955=ORIENTED_EDGE('',*,*,#14155,.F.);
#18956=ORIENTED_EDGE('',*,*,#14159,.T.);
#18957=ORIENTED_EDGE('',*,*,#14247,.T.);
#18958=ORIENTED_EDGE('',*,*,#14242,.T.);
#18959=ORIENTED_EDGE('',*,*,#13655,.T.);
#18960=ORIENTED_EDGE('',*,*,#14248,.F.);
#18961=ORIENTED_EDGE('',*,*,#14236,.F.);
#18962=ORIENTED_EDGE('',*,*,#14249,.F.);
#18963=ORIENTED_EDGE('',*,*,#14250,.F.);
#18964=ORIENTED_EDGE('',*,*,#14251,.F.);
#18965=ORIENTED_EDGE('',*,*,#14227,.F.);
#18966=ORIENTED_EDGE('',*,*,#14225,.F.);
#18967=ORIENTED_EDGE('',*,*,#14168,.T.);
#18968=ORIENTED_EDGE('',*,*,#14164,.T.);
#18969=ORIENTED_EDGE('',*,*,#14162,.F.);
#18970=ORIENTED_EDGE('',*,*,#14252,.F.);
#18971=ORIENTED_EDGE('',*,*,#13700,.F.);
#18972=ORIENTED_EDGE('',*,*,#14253,.T.);
#18973=ORIENTED_EDGE('',*,*,#14254,.F.);
#18974=ORIENTED_EDGE('',*,*,#14170,.F.);
#18975=ORIENTED_EDGE('',*,*,#14255,.T.);
#18976=ORIENTED_EDGE('',*,*,#14256,.T.);
#18977=ORIENTED_EDGE('',*,*,#14257,.F.);
#18978=ORIENTED_EDGE('',*,*,#14171,.F.);
#18979=ORIENTED_EDGE('',*,*,#14254,.T.);
#18980=ORIENTED_EDGE('',*,*,#14258,.T.);
#18981=ORIENTED_EDGE('',*,*,#14259,.F.);
#18982=ORIENTED_EDGE('',*,*,#14172,.F.);
#18983=ORIENTED_EDGE('',*,*,#14257,.T.);
#18984=ORIENTED_EDGE('',*,*,#14260,.T.);
#18985=ORIENTED_EDGE('',*,*,#14261,.F.);
#18986=ORIENTED_EDGE('',*,*,#14173,.F.);
#18987=ORIENTED_EDGE('',*,*,#14259,.T.);
#18988=ORIENTED_EDGE('',*,*,#14262,.T.);
#18989=ORIENTED_EDGE('',*,*,#14263,.F.);
#18990=ORIENTED_EDGE('',*,*,#14174,.F.);
#18991=ORIENTED_EDGE('',*,*,#14261,.T.);
#18992=ORIENTED_EDGE('',*,*,#14264,.T.);
#18993=ORIENTED_EDGE('',*,*,#14265,.F.);
#18994=ORIENTED_EDGE('',*,*,#14175,.F.);
#18995=ORIENTED_EDGE('',*,*,#14263,.T.);
#18996=ORIENTED_EDGE('',*,*,#14266,.T.);
#18997=ORIENTED_EDGE('',*,*,#14267,.F.);
#18998=ORIENTED_EDGE('',*,*,#14176,.F.);
#18999=ORIENTED_EDGE('',*,*,#14265,.T.);
#19000=ORIENTED_EDGE('',*,*,#14268,.T.);
#19001=ORIENTED_EDGE('',*,*,#14269,.F.);
#19002=ORIENTED_EDGE('',*,*,#14177,.F.);
#19003=ORIENTED_EDGE('',*,*,#14267,.T.);
#19004=ORIENTED_EDGE('',*,*,#14270,.T.);
#19005=ORIENTED_EDGE('',*,*,#14271,.F.);
#19006=ORIENTED_EDGE('',*,*,#14178,.F.);
#19007=ORIENTED_EDGE('',*,*,#14269,.T.);
#19008=ORIENTED_EDGE('',*,*,#14272,.T.);
#19009=ORIENTED_EDGE('',*,*,#14273,.F.);
#19010=ORIENTED_EDGE('',*,*,#14179,.F.);
#19011=ORIENTED_EDGE('',*,*,#14271,.T.);
#19012=ORIENTED_EDGE('',*,*,#14274,.T.);
#19013=ORIENTED_EDGE('',*,*,#14275,.F.);
#19014=ORIENTED_EDGE('',*,*,#14180,.F.);
#19015=ORIENTED_EDGE('',*,*,#14273,.T.);
#19016=ORIENTED_EDGE('',*,*,#14276,.T.);
#19017=ORIENTED_EDGE('',*,*,#14277,.F.);
#19018=ORIENTED_EDGE('',*,*,#14181,.F.);
#19019=ORIENTED_EDGE('',*,*,#14275,.T.);
#19020=ORIENTED_EDGE('',*,*,#14278,.T.);
#19021=ORIENTED_EDGE('',*,*,#14279,.F.);
#19022=ORIENTED_EDGE('',*,*,#14182,.F.);
#19023=ORIENTED_EDGE('',*,*,#14277,.T.);
#19024=ORIENTED_EDGE('',*,*,#14280,.T.);
#19025=ORIENTED_EDGE('',*,*,#14281,.F.);
#19026=ORIENTED_EDGE('',*,*,#14183,.F.);
#19027=ORIENTED_EDGE('',*,*,#14279,.T.);
#19028=ORIENTED_EDGE('',*,*,#14282,.T.);
#19029=ORIENTED_EDGE('',*,*,#14283,.F.);
#19030=ORIENTED_EDGE('',*,*,#14184,.F.);
#19031=ORIENTED_EDGE('',*,*,#14281,.T.);
#19032=ORIENTED_EDGE('',*,*,#14284,.T.);
#19033=ORIENTED_EDGE('',*,*,#14285,.F.);
#19034=ORIENTED_EDGE('',*,*,#14185,.F.);
#19035=ORIENTED_EDGE('',*,*,#14283,.T.);
#19036=ORIENTED_EDGE('',*,*,#14286,.T.);
#19037=ORIENTED_EDGE('',*,*,#14287,.F.);
#19038=ORIENTED_EDGE('',*,*,#14186,.F.);
#19039=ORIENTED_EDGE('',*,*,#14285,.T.);
#19040=ORIENTED_EDGE('',*,*,#14288,.T.);
#19041=ORIENTED_EDGE('',*,*,#14289,.F.);
#19042=ORIENTED_EDGE('',*,*,#14187,.F.);
#19043=ORIENTED_EDGE('',*,*,#14287,.T.);
#19044=ORIENTED_EDGE('',*,*,#14290,.T.);
#19045=ORIENTED_EDGE('',*,*,#14291,.F.);
#19046=ORIENTED_EDGE('',*,*,#14188,.F.);
#19047=ORIENTED_EDGE('',*,*,#14289,.T.);
#19048=ORIENTED_EDGE('',*,*,#14292,.T.);
#19049=ORIENTED_EDGE('',*,*,#14293,.F.);
#19050=ORIENTED_EDGE('',*,*,#14189,.F.);
#19051=ORIENTED_EDGE('',*,*,#14291,.T.);
#19052=ORIENTED_EDGE('',*,*,#14294,.T.);
#19053=ORIENTED_EDGE('',*,*,#14295,.F.);
#19054=ORIENTED_EDGE('',*,*,#14190,.F.);
#19055=ORIENTED_EDGE('',*,*,#14293,.T.);
#19056=ORIENTED_EDGE('',*,*,#14296,.T.);
#19057=ORIENTED_EDGE('',*,*,#14297,.F.);
#19058=ORIENTED_EDGE('',*,*,#14191,.F.);
#19059=ORIENTED_EDGE('',*,*,#14295,.T.);
#19060=ORIENTED_EDGE('',*,*,#14298,.T.);
#19061=ORIENTED_EDGE('',*,*,#14299,.F.);
#19062=ORIENTED_EDGE('',*,*,#14192,.F.);
#19063=ORIENTED_EDGE('',*,*,#14297,.T.);
#19064=ORIENTED_EDGE('',*,*,#14300,.T.);
#19065=ORIENTED_EDGE('',*,*,#14301,.F.);
#19066=ORIENTED_EDGE('',*,*,#14193,.F.);
#19067=ORIENTED_EDGE('',*,*,#14299,.T.);
#19068=ORIENTED_EDGE('',*,*,#14302,.T.);
#19069=ORIENTED_EDGE('',*,*,#14303,.F.);
#19070=ORIENTED_EDGE('',*,*,#14194,.F.);
#19071=ORIENTED_EDGE('',*,*,#14301,.T.);
#19072=ORIENTED_EDGE('',*,*,#14304,.T.);
#19073=ORIENTED_EDGE('',*,*,#14305,.F.);
#19074=ORIENTED_EDGE('',*,*,#14195,.F.);
#19075=ORIENTED_EDGE('',*,*,#14303,.T.);
#19076=ORIENTED_EDGE('',*,*,#14306,.T.);
#19077=ORIENTED_EDGE('',*,*,#14307,.F.);
#19078=ORIENTED_EDGE('',*,*,#14196,.F.);
#19079=ORIENTED_EDGE('',*,*,#14305,.T.);
#19080=ORIENTED_EDGE('',*,*,#14308,.T.);
#19081=ORIENTED_EDGE('',*,*,#14309,.F.);
#19082=ORIENTED_EDGE('',*,*,#14197,.F.);
#19083=ORIENTED_EDGE('',*,*,#14307,.T.);
#19084=ORIENTED_EDGE('',*,*,#14310,.T.);
#19085=ORIENTED_EDGE('',*,*,#14311,.F.);
#19086=ORIENTED_EDGE('',*,*,#14198,.F.);
#19087=ORIENTED_EDGE('',*,*,#14309,.T.);
#19088=ORIENTED_EDGE('',*,*,#14312,.T.);
#19089=ORIENTED_EDGE('',*,*,#14313,.F.);
#19090=ORIENTED_EDGE('',*,*,#14199,.F.);
#19091=ORIENTED_EDGE('',*,*,#14311,.T.);
#19092=ORIENTED_EDGE('',*,*,#14314,.T.);
#19093=ORIENTED_EDGE('',*,*,#14315,.F.);
#19094=ORIENTED_EDGE('',*,*,#14200,.F.);
#19095=ORIENTED_EDGE('',*,*,#14313,.T.);
#19096=ORIENTED_EDGE('',*,*,#14316,.T.);
#19097=ORIENTED_EDGE('',*,*,#14317,.F.);
#19098=ORIENTED_EDGE('',*,*,#14201,.F.);
#19099=ORIENTED_EDGE('',*,*,#14315,.T.);
#19100=ORIENTED_EDGE('',*,*,#14318,.T.);
#19101=ORIENTED_EDGE('',*,*,#14319,.F.);
#19102=ORIENTED_EDGE('',*,*,#14202,.F.);
#19103=ORIENTED_EDGE('',*,*,#14317,.T.);
#19104=ORIENTED_EDGE('',*,*,#14320,.T.);
#19105=ORIENTED_EDGE('',*,*,#14321,.F.);
#19106=ORIENTED_EDGE('',*,*,#14203,.F.);
#19107=ORIENTED_EDGE('',*,*,#14319,.T.);
#19108=ORIENTED_EDGE('',*,*,#14322,.T.);
#19109=ORIENTED_EDGE('',*,*,#14323,.F.);
#19110=ORIENTED_EDGE('',*,*,#14204,.F.);
#19111=ORIENTED_EDGE('',*,*,#14321,.T.);
#19112=ORIENTED_EDGE('',*,*,#14324,.T.);
#19113=ORIENTED_EDGE('',*,*,#14325,.F.);
#19114=ORIENTED_EDGE('',*,*,#14205,.F.);
#19115=ORIENTED_EDGE('',*,*,#14323,.T.);
#19116=ORIENTED_EDGE('',*,*,#14326,.T.);
#19117=ORIENTED_EDGE('',*,*,#14327,.F.);
#19118=ORIENTED_EDGE('',*,*,#14206,.F.);
#19119=ORIENTED_EDGE('',*,*,#14325,.T.);
#19120=ORIENTED_EDGE('',*,*,#14328,.T.);
#19121=ORIENTED_EDGE('',*,*,#14329,.F.);
#19122=ORIENTED_EDGE('',*,*,#14207,.F.);
#19123=ORIENTED_EDGE('',*,*,#14327,.T.);
#19124=ORIENTED_EDGE('',*,*,#14330,.T.);
#19125=ORIENTED_EDGE('',*,*,#14331,.F.);
#19126=ORIENTED_EDGE('',*,*,#14208,.F.);
#19127=ORIENTED_EDGE('',*,*,#14329,.T.);
#19128=ORIENTED_EDGE('',*,*,#14332,.T.);
#19129=ORIENTED_EDGE('',*,*,#14333,.F.);
#19130=ORIENTED_EDGE('',*,*,#14209,.F.);
#19131=ORIENTED_EDGE('',*,*,#14331,.T.);
#19132=ORIENTED_EDGE('',*,*,#14334,.T.);
#19133=ORIENTED_EDGE('',*,*,#14335,.F.);
#19134=ORIENTED_EDGE('',*,*,#14210,.F.);
#19135=ORIENTED_EDGE('',*,*,#14333,.T.);
#19136=ORIENTED_EDGE('',*,*,#14336,.T.);
#19137=ORIENTED_EDGE('',*,*,#14337,.F.);
#19138=ORIENTED_EDGE('',*,*,#14211,.F.);
#19139=ORIENTED_EDGE('',*,*,#14335,.T.);
#19140=ORIENTED_EDGE('',*,*,#14338,.T.);
#19141=ORIENTED_EDGE('',*,*,#14339,.F.);
#19142=ORIENTED_EDGE('',*,*,#14212,.F.);
#19143=ORIENTED_EDGE('',*,*,#14337,.T.);
#19144=ORIENTED_EDGE('',*,*,#14340,.T.);
#19145=ORIENTED_EDGE('',*,*,#14255,.F.);
#19146=ORIENTED_EDGE('',*,*,#14213,.F.);
#19147=ORIENTED_EDGE('',*,*,#14339,.T.);
#19148=ORIENTED_EDGE('',*,*,#14341,.T.);
#19149=ORIENTED_EDGE('',*,*,#14342,.T.);
#19150=ORIENTED_EDGE('',*,*,#14343,.T.);
#19151=ORIENTED_EDGE('',*,*,#14344,.T.);
#19152=ORIENTED_EDGE('',*,*,#13666,.F.);
#19153=ORIENTED_EDGE('',*,*,#14345,.F.);
#19154=ORIENTED_EDGE('',*,*,#14346,.T.);
#19155=ORIENTED_EDGE('',*,*,#14347,.F.);
#19156=ORIENTED_EDGE('',*,*,#14342,.F.);
#19157=ORIENTED_EDGE('',*,*,#14348,.F.);
#19158=ORIENTED_EDGE('',*,*,#14349,.F.);
#19159=ORIENTED_EDGE('',*,*,#14350,.F.);
#19160=ORIENTED_EDGE('',*,*,#14346,.F.);
#19161=ORIENTED_EDGE('',*,*,#14351,.F.);
#19162=ORIENTED_EDGE('',*,*,#14352,.F.);
#19163=ORIENTED_EDGE('',*,*,#14353,.F.);
#19164=ORIENTED_EDGE('',*,*,#14349,.T.);
#19165=ORIENTED_EDGE('',*,*,#14354,.F.);
#19166=ORIENTED_EDGE('',*,*,#14355,.F.);
#19167=ORIENTED_EDGE('',*,*,#14356,.F.);
#19168=ORIENTED_EDGE('',*,*,#14352,.T.);
#19169=ORIENTED_EDGE('',*,*,#13663,.F.);
#19170=ORIENTED_EDGE('',*,*,#14357,.F.);
#19171=ORIENTED_EDGE('',*,*,#14358,.F.);
#19172=ORIENTED_EDGE('',*,*,#14359,.F.);
#19173=ORIENTED_EDGE('',*,*,#14360,.T.);
#19174=ORIENTED_EDGE('',*,*,#13660,.F.);
#19175=ORIENTED_EDGE('',*,*,#14361,.F.);
#19176=ORIENTED_EDGE('',*,*,#14362,.F.);
#19177=ORIENTED_EDGE('',*,*,#14363,.F.);
#19178=ORIENTED_EDGE('',*,*,#14358,.T.);
#19179=ORIENTED_EDGE('',*,*,#14364,.F.);
#19180=ORIENTED_EDGE('',*,*,#14365,.F.);
#19181=ORIENTED_EDGE('',*,*,#14366,.F.);
#19182=ORIENTED_EDGE('',*,*,#14362,.T.);
#19183=ORIENTED_EDGE('',*,*,#14367,.F.);
#19184=ORIENTED_EDGE('',*,*,#14365,.T.);
#19185=ORIENTED_EDGE('',*,*,#14368,.F.);
#19186=ORIENTED_EDGE('',*,*,#14344,.F.);
#19187=ORIENTED_EDGE('',*,*,#14369,.F.);
#19188=ORIENTED_EDGE('',*,*,#14233,.T.);
#19189=ORIENTED_EDGE('',*,*,#14214,.T.);
#19190=ORIENTED_EDGE('',*,*,#14370,.T.);
#19191=ORIENTED_EDGE('',*,*,#14371,.T.);
#19192=ORIENTED_EDGE('',*,*,#14372,.T.);
#19193=ORIENTED_EDGE('',*,*,#14372,.F.);
#19194=ORIENTED_EDGE('',*,*,#14373,.T.);
#19195=ORIENTED_EDGE('',*,*,#14374,.T.);
#19196=ORIENTED_EDGE('',*,*,#14375,.F.);
#19197=ORIENTED_EDGE('',*,*,#14376,.T.);
#19198=ORIENTED_EDGE('',*,*,#14377,.F.);
#19199=ORIENTED_EDGE('',*,*,#14374,.F.);
#19200=ORIENTED_EDGE('',*,*,#14378,.T.);
#19201=ORIENTED_EDGE('',*,*,#13648,.F.);
#19202=ORIENTED_EDGE('',*,*,#13651,.F.);
#19203=ORIENTED_EDGE('',*,*,#14379,.T.);
#19204=ORIENTED_EDGE('',*,*,#14380,.T.);
#19205=ORIENTED_EDGE('',*,*,#14376,.F.);
#19206=ORIENTED_EDGE('',*,*,#14381,.F.);
#19207=ORIENTED_EDGE('',*,*,#14382,.T.);
#19208=ORIENTED_EDGE('',*,*,#14383,.T.);
#19209=ORIENTED_EDGE('',*,*,#14379,.F.);
#19210=ORIENTED_EDGE('',*,*,#14384,.F.);
#19211=ORIENTED_EDGE('',*,*,#14385,.T.);
#19212=ORIENTED_EDGE('',*,*,#14386,.T.);
#19213=ORIENTED_EDGE('',*,*,#14382,.F.);
#19214=ORIENTED_EDGE('',*,*,#14387,.F.);
#19215=ORIENTED_EDGE('',*,*,#14385,.F.);
#19216=ORIENTED_EDGE('',*,*,#14388,.T.);
#19217=ORIENTED_EDGE('',*,*,#14389,.T.);
#19218=ORIENTED_EDGE('',*,*,#14390,.F.);
#19219=ORIENTED_EDGE('',*,*,#14391,.T.);
#19220=ORIENTED_EDGE('',*,*,#14392,.T.);
#19221=ORIENTED_EDGE('',*,*,#14389,.F.);
#19222=ORIENTED_EDGE('',*,*,#14393,.F.);
#19223=ORIENTED_EDGE('',*,*,#14394,.T.);
#19224=ORIENTED_EDGE('',*,*,#14395,.T.);
#19225=ORIENTED_EDGE('',*,*,#14391,.F.);
#19226=ORIENTED_EDGE('',*,*,#14396,.F.);
#19227=ORIENTED_EDGE('',*,*,#14397,.T.);
#19228=ORIENTED_EDGE('',*,*,#14398,.T.);
#19229=ORIENTED_EDGE('',*,*,#14394,.F.);
#19230=ORIENTED_EDGE('',*,*,#14399,.F.);
#19231=ORIENTED_EDGE('',*,*,#14397,.F.);
#19232=ORIENTED_EDGE('',*,*,#14400,.T.);
#19233=ORIENTED_EDGE('',*,*,#14401,.T.);
#19234=ORIENTED_EDGE('',*,*,#14402,.F.);
#19235=ORIENTED_EDGE('',*,*,#13654,.F.);
#19236=ORIENTED_EDGE('',*,*,#13657,.F.);
#19237=ORIENTED_EDGE('',*,*,#14401,.F.);
#19238=ORIENTED_EDGE('',*,*,#14403,.T.);
#19239=ORIENTED_EDGE('',*,*,#14404,.T.);
#19240=ORIENTED_EDGE('',*,*,#14405,.F.);
#19241=ORIENTED_EDGE('',*,*,#14404,.F.);
#19242=ORIENTED_EDGE('',*,*,#14406,.T.);
#19243=ORIENTED_EDGE('',*,*,#14407,.T.);
#19244=ORIENTED_EDGE('',*,*,#14408,.F.);
#19245=ORIENTED_EDGE('',*,*,#14407,.F.);
#19246=ORIENTED_EDGE('',*,*,#14409,.T.);
#19247=ORIENTED_EDGE('',*,*,#14410,.T.);
#19248=ORIENTED_EDGE('',*,*,#14411,.F.);
#19249=ORIENTED_EDGE('',*,*,#14412,.T.);
#19250=ORIENTED_EDGE('',*,*,#14413,.T.);
#19251=ORIENTED_EDGE('',*,*,#14216,.T.);
#19252=ORIENTED_EDGE('',*,*,#14246,.T.);
#19253=ORIENTED_EDGE('',*,*,#14414,.F.);
#19254=ORIENTED_EDGE('',*,*,#14410,.F.);
#19255=ORIENTED_EDGE('',*,*,#14415,.T.);
#19256=ORIENTED_EDGE('',*,*,#14221,.F.);
#19257=ORIENTED_EDGE('',*,*,#14220,.F.);
#19258=ORIENTED_EDGE('',*,*,#14413,.F.);
#19259=ORIENTED_EDGE('',*,*,#14416,.T.);
#19260=ORIENTED_EDGE('',*,*,#14417,.F.);
#19261=ORIENTED_EDGE('',*,*,#13652,.T.);
#19262=ORIENTED_EDGE('',*,*,#14418,.T.);
#19263=ORIENTED_EDGE('',*,*,#14419,.T.);
#19264=ORIENTED_EDGE('',*,*,#14417,.T.);
#19265=ORIENTED_EDGE('',*,*,#14420,.T.);
#19266=ORIENTED_EDGE('',*,*,#14421,.F.);
#19267=ORIENTED_EDGE('',*,*,#14418,.F.);
#19268=ORIENTED_EDGE('',*,*,#14422,.T.);
#19269=ORIENTED_EDGE('',*,*,#14423,.T.);
#19270=ORIENTED_EDGE('',*,*,#14424,.F.);
#19271=ORIENTED_EDGE('',*,*,#13698,.F.);
#19272=ORIENTED_EDGE('',*,*,#14425,.T.);
#19273=ORIENTED_EDGE('',*,*,#14426,.F.);
#19274=ORIENTED_EDGE('',*,*,#14427,.F.);
#19275=ORIENTED_EDGE('',*,*,#14428,.T.);
#19276=ORIENTED_EDGE('',*,*,#14426,.T.);
#19277=ORIENTED_EDGE('',*,*,#14429,.T.);
#19278=ORIENTED_EDGE('',*,*,#14430,.T.);
#19279=ORIENTED_EDGE('',*,*,#14370,.F.);
#19280=ORIENTED_EDGE('',*,*,#14224,.F.);
#19281=ORIENTED_EDGE('',*,*,#14229,.T.);
#19282=ORIENTED_EDGE('',*,*,#14431,.T.);
#19283=ORIENTED_EDGE('',*,*,#14427,.T.);
#19284=ORIENTED_EDGE('',*,*,#13646,.T.);
#19285=ORIENTED_EDGE('',*,*,#14432,.F.);
#19286=ORIENTED_EDGE('',*,*,#14423,.F.);
#19287=ORIENTED_EDGE('',*,*,#14433,.T.);
#19288=ORIENTED_EDGE('',*,*,#14434,.T.);
#19289=ORIENTED_EDGE('',*,*,#14435,.F.);
#19290=ORIENTED_EDGE('',*,*,#14360,.F.);
#19291=ORIENTED_EDGE('',*,*,#14436,.F.);
#19292=ORIENTED_EDGE('',*,*,#14437,.T.);
#19293=ORIENTED_EDGE('',*,*,#14438,.F.);
#19294=ORIENTED_EDGE('',*,*,#14439,.F.);
#19295=ORIENTED_EDGE('',*,*,#14440,.F.);
#19296=ORIENTED_EDGE('',*,*,#14355,.T.);
#19297=ORIENTED_EDGE('',*,*,#14245,.F.);
#19298=ORIENTED_EDGE('',*,*,#14244,.F.);
#19299=ORIENTED_EDGE('',*,*,#14240,.T.);
#19300=ORIENTED_EDGE('',*,*,#13709,.T.);
#19301=ORIENTED_EDGE('',*,*,#14441,.T.);
#19302=ORIENTED_EDGE('',*,*,#14436,.T.);
#19303=ORIENTED_EDGE('',*,*,#14359,.T.);
#19304=ORIENTED_EDGE('',*,*,#14363,.T.);
#19305=ORIENTED_EDGE('',*,*,#14366,.T.);
#19306=ORIENTED_EDGE('',*,*,#14367,.T.);
#19307=ORIENTED_EDGE('',*,*,#14343,.F.);
#19308=ORIENTED_EDGE('',*,*,#14347,.T.);
#19309=ORIENTED_EDGE('',*,*,#14350,.T.);
#19310=ORIENTED_EDGE('',*,*,#14353,.T.);
#19311=ORIENTED_EDGE('',*,*,#14356,.T.);
#19312=ORIENTED_EDGE('',*,*,#14440,.T.);
#19313=ORIENTED_EDGE('',*,*,#14442,.T.);
#19314=ORIENTED_EDGE('',*,*,#14443,.T.);
#19315=ORIENTED_EDGE('',*,*,#14249,.T.);
#19316=ORIENTED_EDGE('',*,*,#14238,.F.);
#19317=ORIENTED_EDGE('',*,*,#14234,.F.);
#19318=ORIENTED_EDGE('',*,*,#14369,.T.);
#19319=ORIENTED_EDGE('',*,*,#14375,.T.);
#19320=ORIENTED_EDGE('',*,*,#14377,.T.);
#19321=ORIENTED_EDGE('',*,*,#14380,.F.);
#19322=ORIENTED_EDGE('',*,*,#14383,.F.);
#19323=ORIENTED_EDGE('',*,*,#14386,.F.);
#19324=ORIENTED_EDGE('',*,*,#14390,.T.);
#19325=ORIENTED_EDGE('',*,*,#14392,.F.);
#19326=ORIENTED_EDGE('',*,*,#14395,.F.);
#19327=ORIENTED_EDGE('',*,*,#14398,.F.);
#19328=ORIENTED_EDGE('',*,*,#14402,.T.);
#19329=ORIENTED_EDGE('',*,*,#14405,.T.);
#19330=ORIENTED_EDGE('',*,*,#14408,.T.);
#19331=ORIENTED_EDGE('',*,*,#14411,.T.);
#19332=ORIENTED_EDGE('',*,*,#14414,.T.);
#19333=ORIENTED_EDGE('',*,*,#14444,.F.);
#19334=ORIENTED_EDGE('',*,*,#14250,.T.);
#19335=ORIENTED_EDGE('',*,*,#14443,.F.);
#19336=ORIENTED_EDGE('',*,*,#14445,.F.);
#19337=ORIENTED_EDGE('',*,*,#14368,.T.);
#19338=ORIENTED_EDGE('',*,*,#14364,.T.);
#19339=ORIENTED_EDGE('',*,*,#14361,.T.);
#19340=ORIENTED_EDGE('',*,*,#14357,.T.);
#19341=ORIENTED_EDGE('',*,*,#14435,.T.);
#19342=ORIENTED_EDGE('',*,*,#14446,.T.);
#19343=ORIENTED_EDGE('',*,*,#14447,.T.);
#19344=ORIENTED_EDGE('',*,*,#14448,.T.);
#19345=ORIENTED_EDGE('',*,*,#14449,.T.);
#19346=ORIENTED_EDGE('',*,*,#14450,.T.);
#19347=ORIENTED_EDGE('',*,*,#14451,.T.);
#19348=ORIENTED_EDGE('',*,*,#14452,.T.);
#19349=ORIENTED_EDGE('',*,*,#14453,.T.);
#19350=ORIENTED_EDGE('',*,*,#14454,.T.);
#19351=ORIENTED_EDGE('',*,*,#14455,.T.);
#19352=ORIENTED_EDGE('',*,*,#14456,.T.);
#19353=ORIENTED_EDGE('',*,*,#14457,.T.);
#19354=ORIENTED_EDGE('',*,*,#14458,.T.);
#19355=ORIENTED_EDGE('',*,*,#14459,.T.);
#19356=ORIENTED_EDGE('',*,*,#14460,.T.);
#19357=ORIENTED_EDGE('',*,*,#14461,.T.);
#19358=ORIENTED_EDGE('',*,*,#14462,.T.);
#19359=ORIENTED_EDGE('',*,*,#14463,.T.);
#19360=ORIENTED_EDGE('',*,*,#14464,.T.);
#19361=ORIENTED_EDGE('',*,*,#14465,.T.);
#19362=ORIENTED_EDGE('',*,*,#14466,.T.);
#19363=ORIENTED_EDGE('',*,*,#14467,.T.);
#19364=ORIENTED_EDGE('',*,*,#14468,.T.);
#19365=ORIENTED_EDGE('',*,*,#14469,.T.);
#19366=ORIENTED_EDGE('',*,*,#14470,.T.);
#19367=ORIENTED_EDGE('',*,*,#14471,.T.);
#19368=ORIENTED_EDGE('',*,*,#14472,.T.);
#19369=ORIENTED_EDGE('',*,*,#14473,.T.);
#19370=ORIENTED_EDGE('',*,*,#14474,.T.);
#19371=ORIENTED_EDGE('',*,*,#14475,.T.);
#19372=ORIENTED_EDGE('',*,*,#14476,.T.);
#19373=ORIENTED_EDGE('',*,*,#14477,.T.);
#19374=ORIENTED_EDGE('',*,*,#14478,.T.);
#19375=ORIENTED_EDGE('',*,*,#14479,.T.);
#19376=ORIENTED_EDGE('',*,*,#14480,.T.);
#19377=ORIENTED_EDGE('',*,*,#14481,.T.);
#19378=ORIENTED_EDGE('',*,*,#14482,.T.);
#19379=ORIENTED_EDGE('',*,*,#14438,.T.);
#19380=ORIENTED_EDGE('',*,*,#14354,.T.);
#19381=ORIENTED_EDGE('',*,*,#14351,.T.);
#19382=ORIENTED_EDGE('',*,*,#14348,.T.);
#19383=ORIENTED_EDGE('',*,*,#14345,.T.);
#19384=ORIENTED_EDGE('',*,*,#14341,.F.);
#19385=ORIENTED_EDGE('',*,*,#14340,.F.);
#19386=ORIENTED_EDGE('',*,*,#14338,.F.);
#19387=ORIENTED_EDGE('',*,*,#14336,.F.);
#19388=ORIENTED_EDGE('',*,*,#14334,.F.);
#19389=ORIENTED_EDGE('',*,*,#14332,.F.);
#19390=ORIENTED_EDGE('',*,*,#14330,.F.);
#19391=ORIENTED_EDGE('',*,*,#14328,.F.);
#19392=ORIENTED_EDGE('',*,*,#14326,.F.);
#19393=ORIENTED_EDGE('',*,*,#14324,.F.);
#19394=ORIENTED_EDGE('',*,*,#14322,.F.);
#19395=ORIENTED_EDGE('',*,*,#14320,.F.);
#19396=ORIENTED_EDGE('',*,*,#14318,.F.);
#19397=ORIENTED_EDGE('',*,*,#14316,.F.);
#19398=ORIENTED_EDGE('',*,*,#14314,.F.);
#19399=ORIENTED_EDGE('',*,*,#14312,.F.);
#19400=ORIENTED_EDGE('',*,*,#14310,.F.);
#19401=ORIENTED_EDGE('',*,*,#14308,.F.);
#19402=ORIENTED_EDGE('',*,*,#14306,.F.);
#19403=ORIENTED_EDGE('',*,*,#14304,.F.);
#19404=ORIENTED_EDGE('',*,*,#14302,.F.);
#19405=ORIENTED_EDGE('',*,*,#14300,.F.);
#19406=ORIENTED_EDGE('',*,*,#14298,.F.);
#19407=ORIENTED_EDGE('',*,*,#14296,.F.);
#19408=ORIENTED_EDGE('',*,*,#14294,.F.);
#19409=ORIENTED_EDGE('',*,*,#14292,.F.);
#19410=ORIENTED_EDGE('',*,*,#14290,.F.);
#19411=ORIENTED_EDGE('',*,*,#14288,.F.);
#19412=ORIENTED_EDGE('',*,*,#14286,.F.);
#19413=ORIENTED_EDGE('',*,*,#14284,.F.);
#19414=ORIENTED_EDGE('',*,*,#14282,.F.);
#19415=ORIENTED_EDGE('',*,*,#14280,.F.);
#19416=ORIENTED_EDGE('',*,*,#14278,.F.);
#19417=ORIENTED_EDGE('',*,*,#14276,.F.);
#19418=ORIENTED_EDGE('',*,*,#14274,.F.);
#19419=ORIENTED_EDGE('',*,*,#14272,.F.);
#19420=ORIENTED_EDGE('',*,*,#14270,.F.);
#19421=ORIENTED_EDGE('',*,*,#14268,.F.);
#19422=ORIENTED_EDGE('',*,*,#14266,.F.);
#19423=ORIENTED_EDGE('',*,*,#14264,.F.);
#19424=ORIENTED_EDGE('',*,*,#14262,.F.);
#19425=ORIENTED_EDGE('',*,*,#14260,.F.);
#19426=ORIENTED_EDGE('',*,*,#14258,.F.);
#19427=ORIENTED_EDGE('',*,*,#14256,.F.);
#19428=ORIENTED_EDGE('',*,*,#14253,.F.);
#19429=ORIENTED_EDGE('',*,*,#14430,.F.);
#19430=ORIENTED_EDGE('',*,*,#14429,.F.);
#19431=ORIENTED_EDGE('',*,*,#14425,.F.);
#19432=ORIENTED_EDGE('',*,*,#13697,.F.);
#19433=ORIENTED_EDGE('',*,*,#14483,.F.);
#19434=ORIENTED_EDGE('',*,*,#14484,.F.);
#19435=ORIENTED_EDGE('',*,*,#14485,.F.);
#19436=ORIENTED_EDGE('',*,*,#14486,.F.);
#19437=ORIENTED_EDGE('',*,*,#14487,.F.);
#19438=ORIENTED_EDGE('',*,*,#14488,.T.);
#19439=ORIENTED_EDGE('',*,*,#14489,.F.);
#19440=ORIENTED_EDGE('',*,*,#14490,.T.);
#19441=ORIENTED_EDGE('',*,*,#14491,.F.);
#19442=ORIENTED_EDGE('',*,*,#14492,.F.);
#19443=ORIENTED_EDGE('',*,*,#14493,.F.);
#19444=ORIENTED_EDGE('',*,*,#14494,.F.);
#19445=ORIENTED_EDGE('',*,*,#14495,.F.);
#19446=ORIENTED_EDGE('',*,*,#14433,.F.);
#19447=ORIENTED_EDGE('',*,*,#14422,.F.);
#19448=ORIENTED_EDGE('',*,*,#14420,.F.);
#19449=ORIENTED_EDGE('',*,*,#14416,.F.);
#19450=ORIENTED_EDGE('',*,*,#14412,.F.);
#19451=ORIENTED_EDGE('',*,*,#14409,.F.);
#19452=ORIENTED_EDGE('',*,*,#14406,.F.);
#19453=ORIENTED_EDGE('',*,*,#14403,.F.);
#19454=ORIENTED_EDGE('',*,*,#14400,.F.);
#19455=ORIENTED_EDGE('',*,*,#14399,.T.);
#19456=ORIENTED_EDGE('',*,*,#14396,.T.);
#19457=ORIENTED_EDGE('',*,*,#14393,.T.);
#19458=ORIENTED_EDGE('',*,*,#14388,.F.);
#19459=ORIENTED_EDGE('',*,*,#14387,.T.);
#19460=ORIENTED_EDGE('',*,*,#14384,.T.);
#19461=ORIENTED_EDGE('',*,*,#14381,.T.);
#19462=ORIENTED_EDGE('',*,*,#14378,.F.);
#19463=ORIENTED_EDGE('',*,*,#14373,.F.);
#19464=ORIENTED_EDGE('',*,*,#14371,.F.);
#19465=ORIENTED_EDGE('',*,*,#14496,.F.);
#19466=ORIENTED_EDGE('',*,*,#14497,.T.);
#19467=ORIENTED_EDGE('',*,*,#14490,.F.);
#19468=ORIENTED_EDGE('',*,*,#14498,.F.);
#19469=ORIENTED_EDGE('',*,*,#14499,.T.);
#19470=ORIENTED_EDGE('',*,*,#14500,.T.);
#19471=ORIENTED_EDGE('',*,*,#14486,.T.);
#19472=ORIENTED_EDGE('',*,*,#14501,.F.);
#19473=ORIENTED_EDGE('',*,*,#14502,.T.);
#19474=ORIENTED_EDGE('',*,*,#14501,.T.);
#19475=ORIENTED_EDGE('',*,*,#14485,.T.);
#19476=ORIENTED_EDGE('',*,*,#14503,.F.);
#19477=ORIENTED_EDGE('',*,*,#13637,.F.);
#19478=ORIENTED_EDGE('',*,*,#14504,.T.);
#19479=ORIENTED_EDGE('',*,*,#14503,.T.);
#19480=ORIENTED_EDGE('',*,*,#14484,.T.);
#19481=ORIENTED_EDGE('',*,*,#14505,.F.);
#19482=ORIENTED_EDGE('',*,*,#14506,.T.);
#19483=ORIENTED_EDGE('',*,*,#14507,.F.);
#19484=ORIENTED_EDGE('',*,*,#14487,.T.);
#19485=ORIENTED_EDGE('',*,*,#14500,.F.);
#19486=ORIENTED_EDGE('',*,*,#14508,.F.);
#19487=ORIENTED_EDGE('',*,*,#14509,.T.);
#19488=ORIENTED_EDGE('',*,*,#14510,.F.);
#19489=ORIENTED_EDGE('',*,*,#14480,.F.);
#19490=ORIENTED_EDGE('',*,*,#14511,.F.);
#19491=ORIENTED_EDGE('',*,*,#14512,.T.);
#19492=ORIENTED_EDGE('',*,*,#14513,.F.);
#19493=ORIENTED_EDGE('',*,*,#14478,.F.);
#19494=ORIENTED_EDGE('',*,*,#14513,.T.);
#19495=ORIENTED_EDGE('',*,*,#14514,.T.);
#19496=ORIENTED_EDGE('',*,*,#14508,.T.);
#19497=ORIENTED_EDGE('',*,*,#14479,.F.);
#19498=ORIENTED_EDGE('',*,*,#14510,.T.);
#19499=ORIENTED_EDGE('',*,*,#14515,.T.);
#19500=ORIENTED_EDGE('',*,*,#14516,.T.);
#19501=ORIENTED_EDGE('',*,*,#14481,.F.);
#19502=ORIENTED_EDGE('',*,*,#14516,.F.);
#19503=ORIENTED_EDGE('',*,*,#14517,.T.);
#19504=ORIENTED_EDGE('',*,*,#14505,.T.);
#19505=ORIENTED_EDGE('',*,*,#14483,.T.);
#19506=ORIENTED_EDGE('',*,*,#13696,.T.);
#19507=ORIENTED_EDGE('',*,*,#13702,.T.);
#19508=ORIENTED_EDGE('',*,*,#14445,.T.);
#19509=ORIENTED_EDGE('',*,*,#14442,.F.);
#19510=ORIENTED_EDGE('',*,*,#14439,.T.);
#19511=ORIENTED_EDGE('',*,*,#14482,.F.);
#19512=ORIENTED_EDGE('',*,*,#14518,.T.);
#19513=ORIENTED_EDGE('',*,*,#14519,.F.);
#19514=ORIENTED_EDGE('',*,*,#14476,.F.);
#19515=ORIENTED_EDGE('',*,*,#14520,.F.);
#19516=ORIENTED_EDGE('',*,*,#14521,.T.);
#19517=ORIENTED_EDGE('',*,*,#14522,.F.);
#19518=ORIENTED_EDGE('',*,*,#14474,.F.);
#19519=ORIENTED_EDGE('',*,*,#14523,.F.);
#19520=ORIENTED_EDGE('',*,*,#14522,.T.);
#19521=ORIENTED_EDGE('',*,*,#14524,.T.);
#19522=ORIENTED_EDGE('',*,*,#14520,.T.);
#19523=ORIENTED_EDGE('',*,*,#14475,.F.);
#19524=ORIENTED_EDGE('',*,*,#14525,.T.);
#19525=ORIENTED_EDGE('',*,*,#14526,.F.);
#19526=ORIENTED_EDGE('',*,*,#14472,.F.);
#19527=ORIENTED_EDGE('',*,*,#14527,.F.);
#19528=ORIENTED_EDGE('',*,*,#14528,.T.);
#19529=ORIENTED_EDGE('',*,*,#14529,.F.);
#19530=ORIENTED_EDGE('',*,*,#14470,.F.);
#19531=ORIENTED_EDGE('',*,*,#14530,.F.);
#19532=ORIENTED_EDGE('',*,*,#14529,.T.);
#19533=ORIENTED_EDGE('',*,*,#14531,.T.);
#19534=ORIENTED_EDGE('',*,*,#14527,.T.);
#19535=ORIENTED_EDGE('',*,*,#14471,.F.);
#19536=ORIENTED_EDGE('',*,*,#14526,.T.);
#19537=ORIENTED_EDGE('',*,*,#14532,.T.);
#19538=ORIENTED_EDGE('',*,*,#14523,.T.);
#19539=ORIENTED_EDGE('',*,*,#14473,.F.);
#19540=ORIENTED_EDGE('',*,*,#14533,.T.);
#19541=ORIENTED_EDGE('',*,*,#14534,.F.);
#19542=ORIENTED_EDGE('',*,*,#14468,.F.);
#19543=ORIENTED_EDGE('',*,*,#14535,.F.);
#19544=ORIENTED_EDGE('',*,*,#14536,.T.);
#19545=ORIENTED_EDGE('',*,*,#14537,.F.);
#19546=ORIENTED_EDGE('',*,*,#14466,.F.);
#19547=ORIENTED_EDGE('',*,*,#14538,.F.);
#19548=ORIENTED_EDGE('',*,*,#14537,.T.);
#19549=ORIENTED_EDGE('',*,*,#14539,.T.);
#19550=ORIENTED_EDGE('',*,*,#14535,.T.);
#19551=ORIENTED_EDGE('',*,*,#14467,.F.);
#19552=ORIENTED_EDGE('',*,*,#14540,.F.);
#19553=ORIENTED_EDGE('',*,*,#14541,.T.);
#19554=ORIENTED_EDGE('',*,*,#14542,.T.);
#19555=ORIENTED_EDGE('',*,*,#14464,.F.);
#19556=ORIENTED_EDGE('',*,*,#14542,.F.);
#19557=ORIENTED_EDGE('',*,*,#14543,.T.);
#19558=ORIENTED_EDGE('',*,*,#14538,.T.);
#19559=ORIENTED_EDGE('',*,*,#14465,.F.);
#19560=ORIENTED_EDGE('',*,*,#14544,.T.);
#19561=ORIENTED_EDGE('',*,*,#14545,.F.);
#19562=ORIENTED_EDGE('',*,*,#14462,.F.);
#19563=ORIENTED_EDGE('',*,*,#14546,.F.);
#19564=ORIENTED_EDGE('',*,*,#14547,.T.);
#19565=ORIENTED_EDGE('',*,*,#14548,.F.);
#19566=ORIENTED_EDGE('',*,*,#14460,.F.);
#19567=ORIENTED_EDGE('',*,*,#14549,.F.);
#19568=ORIENTED_EDGE('',*,*,#14548,.T.);
#19569=ORIENTED_EDGE('',*,*,#14550,.T.);
#19570=ORIENTED_EDGE('',*,*,#14546,.T.);
#19571=ORIENTED_EDGE('',*,*,#14461,.F.);
#19572=ORIENTED_EDGE('',*,*,#14551,.T.);
#19573=ORIENTED_EDGE('',*,*,#14552,.F.);
#19574=ORIENTED_EDGE('',*,*,#14458,.F.);
#19575=ORIENTED_EDGE('',*,*,#14553,.F.);
#19576=ORIENTED_EDGE('',*,*,#14554,.T.);
#19577=ORIENTED_EDGE('',*,*,#14555,.F.);
#19578=ORIENTED_EDGE('',*,*,#14456,.F.);
#19579=ORIENTED_EDGE('',*,*,#14556,.F.);
#19580=ORIENTED_EDGE('',*,*,#14555,.T.);
#19581=ORIENTED_EDGE('',*,*,#14557,.T.);
#19582=ORIENTED_EDGE('',*,*,#14553,.T.);
#19583=ORIENTED_EDGE('',*,*,#14457,.F.);
#19584=ORIENTED_EDGE('',*,*,#14552,.T.);
#19585=ORIENTED_EDGE('',*,*,#14558,.T.);
#19586=ORIENTED_EDGE('',*,*,#14549,.T.);
#19587=ORIENTED_EDGE('',*,*,#14459,.F.);
#19588=ORIENTED_EDGE('',*,*,#14545,.T.);
#19589=ORIENTED_EDGE('',*,*,#14559,.T.);
#19590=ORIENTED_EDGE('',*,*,#14540,.T.);
#19591=ORIENTED_EDGE('',*,*,#14463,.F.);
#19592=ORIENTED_EDGE('',*,*,#14560,.T.);
#19593=ORIENTED_EDGE('',*,*,#14561,.F.);
#19594=ORIENTED_EDGE('',*,*,#14454,.F.);
#19595=ORIENTED_EDGE('',*,*,#14562,.F.);
#19596=ORIENTED_EDGE('',*,*,#14563,.T.);
#19597=ORIENTED_EDGE('',*,*,#14564,.F.);
#19598=ORIENTED_EDGE('',*,*,#14452,.F.);
#19599=ORIENTED_EDGE('',*,*,#14565,.F.);
#19600=ORIENTED_EDGE('',*,*,#14564,.T.);
#19601=ORIENTED_EDGE('',*,*,#14566,.T.);
#19602=ORIENTED_EDGE('',*,*,#14562,.T.);
#19603=ORIENTED_EDGE('',*,*,#14453,.F.);
#19604=ORIENTED_EDGE('',*,*,#14567,.F.);
#19605=ORIENTED_EDGE('',*,*,#14568,.T.);
#19606=ORIENTED_EDGE('',*,*,#14569,.F.);
#19607=ORIENTED_EDGE('',*,*,#14450,.F.);
#19608=ORIENTED_EDGE('',*,*,#14570,.F.);
#19609=ORIENTED_EDGE('',*,*,#14571,.T.);
#19610=ORIENTED_EDGE('',*,*,#14572,.F.);
#19611=ORIENTED_EDGE('',*,*,#14448,.F.);
#19612=ORIENTED_EDGE('',*,*,#14573,.T.);
#19613=ORIENTED_EDGE('',*,*,#14574,.T.);
#19614=ORIENTED_EDGE('',*,*,#14494,.T.);
#19615=ORIENTED_EDGE('',*,*,#14575,.F.);
#19616=ORIENTED_EDGE('',*,*,#14576,.T.);
#19617=ORIENTED_EDGE('',*,*,#14575,.T.);
#19618=ORIENTED_EDGE('',*,*,#14493,.T.);
#19619=ORIENTED_EDGE('',*,*,#14577,.F.);
#19620=ORIENTED_EDGE('',*,*,#13640,.F.);
#19621=ORIENTED_EDGE('',*,*,#14578,.T.);
#19622=ORIENTED_EDGE('',*,*,#14577,.T.);
#19623=ORIENTED_EDGE('',*,*,#14492,.T.);
#19624=ORIENTED_EDGE('',*,*,#14579,.F.);
#19625=ORIENTED_EDGE('',*,*,#14580,.T.);
#19626=ORIENTED_EDGE('',*,*,#14579,.T.);
#19627=ORIENTED_EDGE('',*,*,#14491,.T.);
#19628=ORIENTED_EDGE('',*,*,#14497,.F.);
#19629=ORIENTED_EDGE('',*,*,#14574,.F.);
#19630=ORIENTED_EDGE('',*,*,#14581,.T.);
#19631=ORIENTED_EDGE('',*,*,#14582,.T.);
#19632=ORIENTED_EDGE('',*,*,#14446,.F.);
#19633=ORIENTED_EDGE('',*,*,#14437,.F.);
#19634=ORIENTED_EDGE('',*,*,#14441,.F.);
#19635=ORIENTED_EDGE('',*,*,#13708,.F.);
#19636=ORIENTED_EDGE('',*,*,#13704,.F.);
#19637=ORIENTED_EDGE('',*,*,#14434,.F.);
#19638=ORIENTED_EDGE('',*,*,#14495,.T.);
#19639=ORIENTED_EDGE('',*,*,#14582,.F.);
#19640=ORIENTED_EDGE('',*,*,#14583,.T.);
#19641=ORIENTED_EDGE('',*,*,#14570,.T.);
#19642=ORIENTED_EDGE('',*,*,#14447,.F.);
#19643=ORIENTED_EDGE('',*,*,#14572,.T.);
#19644=ORIENTED_EDGE('',*,*,#14584,.T.);
#19645=ORIENTED_EDGE('',*,*,#14567,.T.);
#19646=ORIENTED_EDGE('',*,*,#14449,.F.);
#19647=ORIENTED_EDGE('',*,*,#14569,.T.);
#19648=ORIENTED_EDGE('',*,*,#14585,.T.);
#19649=ORIENTED_EDGE('',*,*,#14565,.T.);
#19650=ORIENTED_EDGE('',*,*,#14451,.F.);
#19651=ORIENTED_EDGE('',*,*,#14561,.T.);
#19652=ORIENTED_EDGE('',*,*,#14586,.T.);
#19653=ORIENTED_EDGE('',*,*,#14556,.T.);
#19654=ORIENTED_EDGE('',*,*,#14455,.F.);
#19655=ORIENTED_EDGE('',*,*,#14534,.T.);
#19656=ORIENTED_EDGE('',*,*,#14587,.T.);
#19657=ORIENTED_EDGE('',*,*,#14530,.T.);
#19658=ORIENTED_EDGE('',*,*,#14469,.F.);
#19659=ORIENTED_EDGE('',*,*,#14519,.T.);
#19660=ORIENTED_EDGE('',*,*,#14588,.T.);
#19661=ORIENTED_EDGE('',*,*,#14511,.T.);
#19662=ORIENTED_EDGE('',*,*,#14477,.F.);
#19663=ORIENTED_EDGE('',*,*,#14488,.F.);
#19664=ORIENTED_EDGE('',*,*,#14507,.T.);
#19665=ORIENTED_EDGE('',*,*,#14589,.F.);
#19666=ORIENTED_EDGE('',*,*,#14590,.F.);
#19667=ORIENTED_EDGE('',*,*,#14489,.T.);
#19668=ORIENTED_EDGE('',*,*,#14590,.T.);
#19669=ORIENTED_EDGE('',*,*,#14591,.T.);
#19670=ORIENTED_EDGE('',*,*,#14498,.T.);
#19671=ORIENTED_EDGE('',*,*,#13643,.F.);
#19672=ORIENTED_EDGE('',*,*,#14591,.F.);
#19673=ORIENTED_EDGE('',*,*,#14589,.T.);
#19674=ORIENTED_EDGE('',*,*,#14506,.F.);
#19675=ORIENTED_EDGE('',*,*,#14499,.F.);
#19676=ORIENTED_EDGE('',*,*,#14502,.F.);
#19677=ORIENTED_EDGE('',*,*,#14504,.F.);
#19678=ORIENTED_EDGE('',*,*,#14517,.F.);
#19679=ORIENTED_EDGE('',*,*,#14515,.F.);
#19680=ORIENTED_EDGE('',*,*,#14509,.F.);
#19681=ORIENTED_EDGE('',*,*,#14514,.F.);
#19682=ORIENTED_EDGE('',*,*,#14512,.F.);
#19683=ORIENTED_EDGE('',*,*,#14588,.F.);
#19684=ORIENTED_EDGE('',*,*,#14518,.F.);
#19685=ORIENTED_EDGE('',*,*,#14524,.F.);
#19686=ORIENTED_EDGE('',*,*,#14521,.F.);
#19687=ORIENTED_EDGE('',*,*,#14532,.F.);
#19688=ORIENTED_EDGE('',*,*,#14525,.F.);
#19689=ORIENTED_EDGE('',*,*,#14531,.F.);
#19690=ORIENTED_EDGE('',*,*,#14528,.F.);
#19691=ORIENTED_EDGE('',*,*,#14587,.F.);
#19692=ORIENTED_EDGE('',*,*,#14533,.F.);
#19693=ORIENTED_EDGE('',*,*,#14539,.F.);
#19694=ORIENTED_EDGE('',*,*,#14536,.F.);
#19695=ORIENTED_EDGE('',*,*,#14543,.F.);
#19696=ORIENTED_EDGE('',*,*,#14541,.F.);
#19697=ORIENTED_EDGE('',*,*,#14559,.F.);
#19698=ORIENTED_EDGE('',*,*,#14544,.F.);
#19699=ORIENTED_EDGE('',*,*,#14550,.F.);
#19700=ORIENTED_EDGE('',*,*,#14547,.F.);
#19701=ORIENTED_EDGE('',*,*,#14558,.F.);
#19702=ORIENTED_EDGE('',*,*,#14551,.F.);
#19703=ORIENTED_EDGE('',*,*,#14557,.F.);
#19704=ORIENTED_EDGE('',*,*,#14554,.F.);
#19705=ORIENTED_EDGE('',*,*,#14586,.F.);
#19706=ORIENTED_EDGE('',*,*,#14560,.F.);
#19707=ORIENTED_EDGE('',*,*,#14566,.F.);
#19708=ORIENTED_EDGE('',*,*,#14563,.F.);
#19709=ORIENTED_EDGE('',*,*,#14585,.F.);
#19710=ORIENTED_EDGE('',*,*,#14568,.F.);
#19711=ORIENTED_EDGE('',*,*,#14584,.F.);
#19712=ORIENTED_EDGE('',*,*,#14571,.F.);
#19713=ORIENTED_EDGE('',*,*,#14583,.F.);
#19714=ORIENTED_EDGE('',*,*,#14581,.F.);
#19715=ORIENTED_EDGE('',*,*,#14573,.F.);
#19716=ORIENTED_EDGE('',*,*,#14576,.F.);
#19717=ORIENTED_EDGE('',*,*,#14578,.F.);
#19718=ORIENTED_EDGE('',*,*,#14580,.F.);
#19719=ORIENTED_EDGE('',*,*,#14496,.T.);
#19720=ORIENTED_EDGE('',*,*,#13986,.T.);
#19721=ORIENTED_EDGE('',*,*,#13984,.T.);
#19722=ORIENTED_EDGE('',*,*,#13982,.T.);
#19723=ORIENTED_EDGE('',*,*,#13980,.T.);
#19724=ORIENTED_EDGE('',*,*,#13978,.T.);
#19725=ORIENTED_EDGE('',*,*,#13976,.T.);
#19726=ORIENTED_EDGE('',*,*,#13974,.T.);
#19727=ORIENTED_EDGE('',*,*,#13972,.T.);
#19728=ORIENTED_EDGE('',*,*,#13970,.T.);
#19729=ORIENTED_EDGE('',*,*,#13968,.T.);
#19730=ORIENTED_EDGE('',*,*,#13966,.T.);
#19731=ORIENTED_EDGE('',*,*,#13964,.T.);
#19732=ORIENTED_EDGE('',*,*,#13962,.T.);
#19733=ORIENTED_EDGE('',*,*,#13960,.T.);
#19734=ORIENTED_EDGE('',*,*,#13958,.T.);
#19735=ORIENTED_EDGE('',*,*,#13956,.T.);
#19736=ORIENTED_EDGE('',*,*,#13954,.T.);
#19737=ORIENTED_EDGE('',*,*,#13952,.T.);
#19738=ORIENTED_EDGE('',*,*,#13950,.T.);
#19739=ORIENTED_EDGE('',*,*,#13948,.T.);
#19740=ORIENTED_EDGE('',*,*,#13946,.T.);
#19741=ORIENTED_EDGE('',*,*,#13944,.T.);
#19742=ORIENTED_EDGE('',*,*,#13942,.T.);
#19743=ORIENTED_EDGE('',*,*,#13940,.T.);
#19744=ORIENTED_EDGE('',*,*,#13938,.T.);
#19745=ORIENTED_EDGE('',*,*,#13936,.T.);
#19746=ORIENTED_EDGE('',*,*,#13934,.T.);
#19747=ORIENTED_EDGE('',*,*,#13932,.T.);
#19748=ORIENTED_EDGE('',*,*,#13930,.T.);
#19749=ORIENTED_EDGE('',*,*,#13928,.T.);
#19750=ORIENTED_EDGE('',*,*,#13926,.T.);
#19751=ORIENTED_EDGE('',*,*,#13924,.T.);
#19752=ORIENTED_EDGE('',*,*,#13922,.T.);
#19753=ORIENTED_EDGE('',*,*,#13920,.T.);
#19754=ORIENTED_EDGE('',*,*,#13918,.T.);
#19755=ORIENTED_EDGE('',*,*,#13916,.T.);
#19756=ORIENTED_EDGE('',*,*,#13914,.T.);
#19757=ORIENTED_EDGE('',*,*,#13912,.T.);
#19758=ORIENTED_EDGE('',*,*,#13910,.T.);
#19759=ORIENTED_EDGE('',*,*,#13908,.T.);
#19760=ORIENTED_EDGE('',*,*,#13906,.T.);
#19761=ORIENTED_EDGE('',*,*,#13904,.T.);
#19762=ORIENTED_EDGE('',*,*,#13902,.T.);
#19763=ORIENTED_EDGE('',*,*,#13899,.T.);
#19764=ORIENTED_EDGE('',*,*,#13991,.T.);
#19765=ORIENTED_EDGE('',*,*,#14056,.F.);
#19766=ORIENTED_EDGE('',*,*,#14592,.F.);
#19767=ORIENTED_EDGE('',*,*,#14593,.T.);
#19768=ORIENTED_EDGE('',*,*,#13992,.T.);
#19769=ORIENTED_EDGE('',*,*,#14593,.F.);
#19770=ORIENTED_EDGE('',*,*,#14594,.F.);
#19771=ORIENTED_EDGE('',*,*,#14595,.T.);
#19772=ORIENTED_EDGE('',*,*,#13993,.T.);
#19773=ORIENTED_EDGE('',*,*,#14595,.F.);
#19774=ORIENTED_EDGE('',*,*,#14596,.F.);
#19775=ORIENTED_EDGE('',*,*,#14059,.T.);
#19776=ORIENTED_EDGE('',*,*,#14055,.T.);
#19777=ORIENTED_EDGE('',*,*,#14596,.T.);
#19778=ORIENTED_EDGE('',*,*,#14594,.T.);
#19779=ORIENTED_EDGE('',*,*,#14592,.T.);
#19780=ORIENTED_EDGE('',*,*,#14247,.F.);
#19781=ORIENTED_EDGE('',*,*,#14158,.F.);
#19782=ORIENTED_EDGE('',*,*,#14231,.T.);
#19783=ORIENTED_EDGE('',*,*,#13705,.T.);
#19784=ORIENTED_EDGE('',*,*,#13707,.T.);
#19785=ORIENTED_EDGE('',*,*,#14239,.T.);
#19786=ORIENTED_EDGE('',*,*,#14243,.F.);
#19787=ORIENTED_EDGE('',*,*,#14415,.F.);
#19788=ORIENTED_EDGE('',*,*,#14419,.F.);
#19789=ORIENTED_EDGE('',*,*,#14421,.T.);
#19790=ORIENTED_EDGE('',*,*,#14432,.T.);
#19791=ORIENTED_EDGE('',*,*,#13703,.T.);
#19792=ORIENTED_EDGE('',*,*,#14230,.T.);
#19793=ORIENTED_EDGE('',*,*,#14222,.F.);
#19794=ORIENTED_EDGE('',*,*,#14232,.F.);
#19795=ORIENTED_EDGE('',*,*,#14237,.F.);
#19796=ORIENTED_EDGE('',*,*,#14248,.T.);
#19797=ORIENTED_EDGE('',*,*,#14444,.T.);
#19798=ORIENTED_EDGE('',*,*,#13701,.T.);
#19799=ORIENTED_EDGE('',*,*,#14252,.T.);
#19800=ORIENTED_EDGE('',*,*,#14161,.F.);
#19801=ORIENTED_EDGE('',*,*,#14251,.T.);
#19802=ORIENTED_EDGE('',*,*,#13699,.T.);
#19803=ORIENTED_EDGE('',*,*,#13695,.T.);
#19804=ORIENTED_EDGE('',*,*,#14424,.T.);
#19805=ORIENTED_EDGE('',*,*,#14428,.F.);
#19806=ORIENTED_EDGE('',*,*,#14431,.F.);
#19807=ORIENTED_EDGE('',*,*,#14228,.F.);
#19808=ORIENTED_EDGE('',*,*,#14597,.T.);
#19809=ORIENTED_EDGE('',*,*,#14598,.T.);
#19810=ORIENTED_EDGE('',*,*,#14599,.T.);
#19811=ORIENTED_EDGE('',*,*,#14598,.F.);
#19812=ORIENTED_EDGE('',*,*,#14599,.F.);
#19813=ORIENTED_EDGE('',*,*,#14600,.T.);
#19814=ORIENTED_EDGE('',*,*,#14601,.T.);
#19815=ORIENTED_EDGE('',*,*,#14600,.F.);
#19816=ORIENTED_EDGE('',*,*,#14601,.F.);
#19817=ORIENTED_EDGE('',*,*,#14602,.T.);
#19818=ORIENTED_EDGE('',*,*,#14603,.T.);
#19819=ORIENTED_EDGE('',*,*,#14602,.F.);
#19820=ORIENTED_EDGE('',*,*,#14604,.F.);
#19821=ORIENTED_EDGE('',*,*,#14605,.T.);
#19822=ORIENTED_EDGE('',*,*,#14606,.F.);
#19823=ORIENTED_EDGE('',*,*,#14607,.F.);
#19824=ORIENTED_EDGE('',*,*,#14608,.T.);
#19825=ORIENTED_EDGE('',*,*,#14609,.F.);
#19826=ORIENTED_EDGE('',*,*,#14610,.F.);
#19827=ORIENTED_EDGE('',*,*,#14611,.F.);
#19828=ORIENTED_EDGE('',*,*,#14612,.F.);
#19829=ORIENTED_EDGE('',*,*,#14613,.T.);
#19830=ORIENTED_EDGE('',*,*,#14614,.T.);
#19831=ORIENTED_EDGE('',*,*,#14613,.F.);
#19832=ORIENTED_EDGE('',*,*,#14615,.F.);
#19833=ORIENTED_EDGE('',*,*,#14616,.F.);
#19834=ORIENTED_EDGE('',*,*,#14615,.T.);
#19835=ORIENTED_EDGE('',*,*,#14612,.T.);
#19836=ORIENTED_EDGE('',*,*,#14617,.F.);
#19837=ORIENTED_EDGE('',*,*,#14618,.F.);
#19838=ORIENTED_EDGE('',*,*,#14619,.T.);
#19839=ORIENTED_EDGE('',*,*,#14620,.T.);
#19840=ORIENTED_EDGE('',*,*,#14621,.T.);
#19841=ORIENTED_EDGE('',*,*,#14622,.T.);
#19842=ORIENTED_EDGE('',*,*,#14623,.T.);
#19843=ORIENTED_EDGE('',*,*,#14624,.T.);
#19844=ORIENTED_EDGE('',*,*,#14625,.T.);
#19845=ORIENTED_EDGE('',*,*,#14619,.F.);
#19846=ORIENTED_EDGE('',*,*,#14616,.T.);
#19847=ORIENTED_EDGE('',*,*,#14618,.T.);
#19848=ORIENTED_EDGE('',*,*,#14626,.T.);
#19849=ORIENTED_EDGE('',*,*,#14626,.F.);
#19850=ORIENTED_EDGE('',*,*,#14617,.T.);
#19851=ORIENTED_EDGE('',*,*,#14611,.T.);
#19852=ORIENTED_EDGE('',*,*,#14627,.F.);
#19853=ORIENTED_EDGE('',*,*,#14605,.F.);
#19854=ORIENTED_EDGE('',*,*,#14628,.F.);
#19855=ORIENTED_EDGE('',*,*,#14629,.F.);
#19856=ORIENTED_EDGE('',*,*,#14630,.F.);
#19857=ORIENTED_EDGE('',*,*,#14631,.F.);
#19858=ORIENTED_EDGE('',*,*,#14597,.F.);
#19859=ORIENTED_EDGE('',*,*,#14632,.F.);
#19860=ORIENTED_EDGE('',*,*,#14608,.F.);
#19861=ORIENTED_EDGE('',*,*,#14633,.F.);
#19862=ORIENTED_EDGE('',*,*,#14634,.F.);
#19863=ORIENTED_EDGE('',*,*,#14635,.F.);
#19864=ORIENTED_EDGE('',*,*,#14636,.T.);
#19865=ORIENTED_EDGE('',*,*,#14614,.F.);
#19866=ORIENTED_EDGE('',*,*,#14623,.F.);
#19867=ORIENTED_EDGE('',*,*,#14637,.F.);
#19868=ORIENTED_EDGE('',*,*,#14638,.F.);
#19869=ORIENTED_EDGE('',*,*,#14624,.F.);
#19870=ORIENTED_EDGE('',*,*,#14639,.F.);
#19871=ORIENTED_EDGE('',*,*,#14640,.F.);
#19872=ORIENTED_EDGE('',*,*,#14625,.F.);
#19873=ORIENTED_EDGE('',*,*,#14641,.F.);
#19874=ORIENTED_EDGE('',*,*,#14642,.F.);
#19875=ORIENTED_EDGE('',*,*,#14620,.F.);
#19876=ORIENTED_EDGE('',*,*,#14643,.F.);
#19877=ORIENTED_EDGE('',*,*,#14644,.F.);
#19878=ORIENTED_EDGE('',*,*,#14621,.F.);
#19879=ORIENTED_EDGE('',*,*,#14645,.F.);
#19880=ORIENTED_EDGE('',*,*,#14646,.F.);
#19881=ORIENTED_EDGE('',*,*,#14622,.F.);
#19882=ORIENTED_EDGE('',*,*,#14647,.F.);
#19883=ORIENTED_EDGE('',*,*,#14648,.F.);
#19884=ORIENTED_EDGE('',*,*,#14649,.F.);
#19885=ORIENTED_EDGE('',*,*,#14650,.F.);
#19886=ORIENTED_EDGE('',*,*,#14641,.T.);
#19887=ORIENTED_EDGE('',*,*,#14640,.T.);
#19888=ORIENTED_EDGE('',*,*,#14651,.T.);
#19889=ORIENTED_EDGE('',*,*,#14652,.F.);
#19890=ORIENTED_EDGE('',*,*,#14653,.F.);
#19891=ORIENTED_EDGE('',*,*,#14643,.T.);
#19892=ORIENTED_EDGE('',*,*,#14642,.T.);
#19893=ORIENTED_EDGE('',*,*,#14650,.T.);
#19894=ORIENTED_EDGE('',*,*,#14654,.F.);
#19895=ORIENTED_EDGE('',*,*,#14655,.F.);
#19896=ORIENTED_EDGE('',*,*,#14645,.T.);
#19897=ORIENTED_EDGE('',*,*,#14644,.T.);
#19898=ORIENTED_EDGE('',*,*,#14653,.T.);
#19899=ORIENTED_EDGE('',*,*,#14656,.F.);
#19900=ORIENTED_EDGE('',*,*,#14657,.F.);
#19901=ORIENTED_EDGE('',*,*,#14647,.T.);
#19902=ORIENTED_EDGE('',*,*,#14646,.T.);
#19903=ORIENTED_EDGE('',*,*,#14655,.T.);
#19904=ORIENTED_EDGE('',*,*,#14658,.F.);
#19905=ORIENTED_EDGE('',*,*,#14659,.F.);
#19906=ORIENTED_EDGE('',*,*,#14637,.T.);
#19907=ORIENTED_EDGE('',*,*,#14648,.T.);
#19908=ORIENTED_EDGE('',*,*,#14657,.T.);
#19909=ORIENTED_EDGE('',*,*,#14660,.F.);
#19910=ORIENTED_EDGE('',*,*,#14651,.F.);
#19911=ORIENTED_EDGE('',*,*,#14639,.T.);
#19912=ORIENTED_EDGE('',*,*,#14638,.T.);
#19913=ORIENTED_EDGE('',*,*,#14659,.T.);
#19914=ORIENTED_EDGE('',*,*,#14649,.T.);
#19915=ORIENTED_EDGE('',*,*,#14660,.T.);
#19916=ORIENTED_EDGE('',*,*,#14658,.T.);
#19917=ORIENTED_EDGE('',*,*,#14656,.T.);
#19918=ORIENTED_EDGE('',*,*,#14654,.T.);
#19919=ORIENTED_EDGE('',*,*,#14652,.T.);
#19920=ORIENTED_EDGE('',*,*,#14661,.F.);
#19921=ORIENTED_EDGE('',*,*,#14633,.T.);
#19922=ORIENTED_EDGE('',*,*,#14662,.F.);
#19923=ORIENTED_EDGE('',*,*,#14663,.F.);
#19924=ORIENTED_EDGE('',*,*,#14634,.T.);
#19925=ORIENTED_EDGE('',*,*,#14664,.F.);
#19926=ORIENTED_EDGE('',*,*,#14635,.T.);
#19927=ORIENTED_EDGE('',*,*,#14665,.F.);
#19928=ORIENTED_EDGE('',*,*,#14666,.F.);
#19929=ORIENTED_EDGE('',*,*,#14636,.F.);
#19930=ORIENTED_EDGE('',*,*,#14667,.F.);
#19931=ORIENTED_EDGE('',*,*,#14668,.F.);
#19932=ORIENTED_EDGE('',*,*,#14632,.T.);
#19933=ORIENTED_EDGE('',*,*,#14669,.F.);
#19934=ORIENTED_EDGE('',*,*,#14670,.F.);
#19935=ORIENTED_EDGE('',*,*,#14627,.T.);
#19936=ORIENTED_EDGE('',*,*,#14671,.F.);
#19937=ORIENTED_EDGE('',*,*,#14672,.F.);
#19938=ORIENTED_EDGE('',*,*,#14631,.T.);
#19939=ORIENTED_EDGE('',*,*,#14673,.F.);
#19940=ORIENTED_EDGE('',*,*,#14674,.F.);
#19941=ORIENTED_EDGE('',*,*,#14630,.T.);
#19942=ORIENTED_EDGE('',*,*,#14675,.F.);
#19943=ORIENTED_EDGE('',*,*,#14676,.F.);
#19944=ORIENTED_EDGE('',*,*,#14629,.T.);
#19945=ORIENTED_EDGE('',*,*,#14677,.F.);
#19946=ORIENTED_EDGE('',*,*,#14678,.F.);
#19947=ORIENTED_EDGE('',*,*,#14628,.T.);
#19948=ORIENTED_EDGE('',*,*,#14679,.F.);
#19949=ORIENTED_EDGE('',*,*,#14680,.F.);
#19950=ORIENTED_EDGE('',*,*,#14681,.F.);
#19951=ORIENTED_EDGE('',*,*,#14665,.T.);
#19952=ORIENTED_EDGE('',*,*,#14663,.T.);
#19953=ORIENTED_EDGE('',*,*,#14682,.T.);
#19954=ORIENTED_EDGE('',*,*,#14679,.T.);
#19955=ORIENTED_EDGE('',*,*,#14607,.T.);
#19956=ORIENTED_EDGE('',*,*,#14682,.F.);
#19957=ORIENTED_EDGE('',*,*,#14664,.T.);
#19958=ORIENTED_EDGE('',*,*,#14661,.T.);
#19959=ORIENTED_EDGE('',*,*,#14683,.T.);
#19960=ORIENTED_EDGE('',*,*,#14677,.T.);
#19961=ORIENTED_EDGE('',*,*,#14680,.T.);
#19962=ORIENTED_EDGE('',*,*,#14683,.F.);
#19963=ORIENTED_EDGE('',*,*,#14662,.T.);
#19964=ORIENTED_EDGE('',*,*,#14610,.T.);
#19965=ORIENTED_EDGE('',*,*,#14684,.T.);
#19966=ORIENTED_EDGE('',*,*,#14675,.T.);
#19967=ORIENTED_EDGE('',*,*,#14678,.T.);
#19968=ORIENTED_EDGE('',*,*,#14684,.F.);
#19969=ORIENTED_EDGE('',*,*,#14609,.T.);
#19970=ORIENTED_EDGE('',*,*,#14670,.T.);
#19971=ORIENTED_EDGE('',*,*,#14685,.T.);
#19972=ORIENTED_EDGE('',*,*,#14673,.T.);
#19973=ORIENTED_EDGE('',*,*,#14676,.T.);
#19974=ORIENTED_EDGE('',*,*,#14685,.F.);
#19975=ORIENTED_EDGE('',*,*,#14669,.T.);
#19976=ORIENTED_EDGE('',*,*,#14668,.T.);
#19977=ORIENTED_EDGE('',*,*,#14686,.T.);
#19978=ORIENTED_EDGE('',*,*,#14671,.T.);
#19979=ORIENTED_EDGE('',*,*,#14674,.T.);
#19980=ORIENTED_EDGE('',*,*,#14686,.F.);
#19981=ORIENTED_EDGE('',*,*,#14667,.T.);
#19982=ORIENTED_EDGE('',*,*,#14666,.T.);
#19983=ORIENTED_EDGE('',*,*,#14681,.T.);
#19984=ORIENTED_EDGE('',*,*,#14606,.T.);
#19985=ORIENTED_EDGE('',*,*,#14672,.T.);
#19986=ORIENTED_EDGE('',*,*,#14603,.F.);
#19987=ORIENTED_EDGE('',*,*,#14604,.T.);
#19988=ORIENTED_EDGE('',*,*,#14687,.F.);
#19989=ORIENTED_EDGE('',*,*,#14688,.T.);
#19990=ORIENTED_EDGE('',*,*,#14689,.T.);
#19991=ORIENTED_EDGE('',*,*,#14690,.T.);
#19992=ORIENTED_EDGE('',*,*,#14691,.T.);
#19993=ORIENTED_EDGE('',*,*,#14692,.T.);
#19994=ORIENTED_EDGE('',*,*,#14693,.T.);
#19995=ORIENTED_EDGE('',*,*,#14688,.F.);
#19996=ORIENTED_EDGE('',*,*,#14694,.F.);
#19997=ORIENTED_EDGE('',*,*,#14695,.T.);
#19998=ORIENTED_EDGE('',*,*,#14687,.T.);
#19999=ORIENTED_EDGE('',*,*,#14695,.F.);
#20000=ORIENTED_EDGE('',*,*,#14696,.F.);
#20001=ORIENTED_EDGE('',*,*,#14697,.T.);
#20002=ORIENTED_EDGE('',*,*,#14698,.T.);
#20003=ORIENTED_EDGE('',*,*,#14697,.F.);
#20004=ORIENTED_EDGE('',*,*,#14699,.F.);
#20005=ORIENTED_EDGE('',*,*,#14700,.T.);
#20006=ORIENTED_EDGE('',*,*,#14696,.T.);
#20007=ORIENTED_EDGE('',*,*,#14700,.F.);
#20008=ORIENTED_EDGE('',*,*,#14701,.F.);
#20009=ORIENTED_EDGE('',*,*,#14702,.T.);
#20010=ORIENTED_EDGE('',*,*,#14699,.T.);
#20011=ORIENTED_EDGE('',*,*,#14702,.F.);
#20012=ORIENTED_EDGE('',*,*,#14703,.F.);
#20013=ORIENTED_EDGE('',*,*,#14704,.T.);
#20014=ORIENTED_EDGE('',*,*,#14705,.T.);
#20015=ORIENTED_EDGE('',*,*,#14704,.F.);
#20016=ORIENTED_EDGE('',*,*,#14706,.F.);
#20017=ORIENTED_EDGE('',*,*,#14707,.F.);
#20018=ORIENTED_EDGE('',*,*,#14708,.T.);
#20019=ORIENTED_EDGE('',*,*,#14703,.T.);
#20020=ORIENTED_EDGE('',*,*,#14708,.F.);
#20021=ORIENTED_EDGE('',*,*,#14706,.T.);
#20022=ORIENTED_EDGE('',*,*,#14707,.T.);
#20023=ORIENTED_EDGE('',*,*,#14709,.T.);
#20024=ORIENTED_EDGE('',*,*,#14710,.F.);
#20025=ORIENTED_EDGE('',*,*,#14709,.F.);
#20026=ORIENTED_EDGE('',*,*,#14711,.F.);
#20027=ORIENTED_EDGE('',*,*,#14712,.T.);
#20028=ORIENTED_EDGE('',*,*,#14713,.T.);
#20029=ORIENTED_EDGE('',*,*,#14712,.F.);
#20030=ORIENTED_EDGE('',*,*,#14714,.F.);
#20031=ORIENTED_EDGE('',*,*,#14715,.T.);
#20032=ORIENTED_EDGE('',*,*,#14711,.T.);
#20033=ORIENTED_EDGE('',*,*,#14715,.F.);
#20034=ORIENTED_EDGE('',*,*,#14716,.F.);
#20035=ORIENTED_EDGE('',*,*,#14717,.T.);
#20036=ORIENTED_EDGE('',*,*,#14718,.T.);
#20037=ORIENTED_EDGE('',*,*,#14717,.F.);
#20038=ORIENTED_EDGE('',*,*,#14719,.F.);
#20039=ORIENTED_EDGE('',*,*,#14720,.F.);
#20040=ORIENTED_EDGE('',*,*,#14721,.T.);
#20041=ORIENTED_EDGE('',*,*,#14722,.T.);
#20042=ORIENTED_EDGE('',*,*,#14721,.F.);
#20043=ORIENTED_EDGE('',*,*,#14719,.T.);
#20044=ORIENTED_EDGE('',*,*,#14720,.T.);
#20045=ORIENTED_EDGE('',*,*,#14723,.T.);
#20046=ORIENTED_EDGE('',*,*,#14724,.F.);
#20047=ORIENTED_EDGE('',*,*,#14723,.F.);
#20048=ORIENTED_EDGE('',*,*,#14722,.F.);
#20049=ORIENTED_EDGE('',*,*,#14716,.T.);
#20050=ORIENTED_EDGE('',*,*,#14714,.T.);
#20051=ORIENTED_EDGE('',*,*,#14718,.F.);
#20052=ORIENTED_EDGE('',*,*,#14710,.T.);
#20053=ORIENTED_EDGE('',*,*,#14713,.F.);
#20054=ORIENTED_EDGE('',*,*,#14705,.F.);
#20055=ORIENTED_EDGE('',*,*,#14701,.T.);
#20056=ORIENTED_EDGE('',*,*,#14698,.F.);
#20057=ORIENTED_EDGE('',*,*,#14694,.T.);
#20058=ORIENTED_EDGE('',*,*,#14693,.F.);
#20059=ORIENTED_EDGE('',*,*,#14725,.T.);
#20060=ORIENTED_EDGE('',*,*,#14726,.T.);
#20061=ORIENTED_EDGE('',*,*,#14727,.T.);
#20062=ORIENTED_EDGE('',*,*,#14689,.F.);
#20063=ORIENTED_EDGE('',*,*,#14726,.F.);
#20064=ORIENTED_EDGE('',*,*,#14728,.F.);
#20065=ORIENTED_EDGE('',*,*,#14729,.F.);
#20066=ORIENTED_EDGE('',*,*,#14730,.T.);
#20067=ORIENTED_EDGE('',*,*,#14724,.T.);
#20068=ORIENTED_EDGE('',*,*,#14692,.F.);
#20069=ORIENTED_EDGE('',*,*,#14731,.T.);
#20070=ORIENTED_EDGE('',*,*,#14732,.T.);
#20071=ORIENTED_EDGE('',*,*,#14728,.T.);
#20072=ORIENTED_EDGE('',*,*,#14725,.F.);
#20073=ORIENTED_EDGE('',*,*,#14733,.F.);
#20074=ORIENTED_EDGE('',*,*,#14734,.T.);
#20075=ORIENTED_EDGE('',*,*,#14690,.F.);
#20076=ORIENTED_EDGE('',*,*,#14727,.F.);
#20077=ORIENTED_EDGE('',*,*,#14730,.F.);
#20078=ORIENTED_EDGE('',*,*,#14735,.T.);
#20079=ORIENTED_EDGE('',*,*,#14733,.T.);
#20080=ORIENTED_EDGE('',*,*,#14729,.T.);
#20081=ORIENTED_EDGE('',*,*,#14732,.F.);
#20082=ORIENTED_EDGE('',*,*,#14731,.F.);
#20083=ORIENTED_EDGE('',*,*,#14691,.F.);
#20084=ORIENTED_EDGE('',*,*,#14734,.F.);
#20085=ORIENTED_EDGE('',*,*,#14735,.F.);
#20086=ORIENTED_EDGE('',*,*,#14736,.F.);
#20087=ORIENTED_EDGE('',*,*,#14737,.T.);
#20088=ORIENTED_EDGE('',*,*,#14738,.F.);
#20089=ORIENTED_EDGE('',*,*,#14737,.F.);
#20090=ORIENTED_EDGE('',*,*,#14739,.F.);
#20091=ORIENTED_EDGE('',*,*,#14740,.T.);
#20092=ORIENTED_EDGE('',*,*,#14741,.T.);
#20093=ORIENTED_EDGE('',*,*,#14740,.F.);
#20094=ORIENTED_EDGE('',*,*,#14742,.F.);
#20095=ORIENTED_EDGE('',*,*,#14743,.T.);
#20096=ORIENTED_EDGE('',*,*,#14744,.T.);
#20097=ORIENTED_EDGE('',*,*,#14743,.F.);
#20098=ORIENTED_EDGE('',*,*,#14745,.F.);
#20099=ORIENTED_EDGE('',*,*,#14746,.T.);
#20100=ORIENTED_EDGE('',*,*,#14747,.T.);
#20101=ORIENTED_EDGE('',*,*,#14746,.F.);
#20102=ORIENTED_EDGE('',*,*,#14748,.F.);
#20103=ORIENTED_EDGE('',*,*,#14749,.T.);
#20104=ORIENTED_EDGE('',*,*,#14750,.T.);
#20105=ORIENTED_EDGE('',*,*,#14749,.F.);
#20106=ORIENTED_EDGE('',*,*,#14751,.F.);
#20107=ORIENTED_EDGE('',*,*,#14752,.T.);
#20108=ORIENTED_EDGE('',*,*,#14753,.T.);
#20109=ORIENTED_EDGE('',*,*,#14752,.F.);
#20110=ORIENTED_EDGE('',*,*,#14754,.F.);
#20111=ORIENTED_EDGE('',*,*,#14755,.T.);
#20112=ORIENTED_EDGE('',*,*,#14756,.T.);
#20113=ORIENTED_EDGE('',*,*,#14755,.F.);
#20114=ORIENTED_EDGE('',*,*,#14757,.F.);
#20115=ORIENTED_EDGE('',*,*,#14758,.T.);
#20116=ORIENTED_EDGE('',*,*,#14759,.T.);
#20117=ORIENTED_EDGE('',*,*,#14758,.F.);
#20118=ORIENTED_EDGE('',*,*,#14760,.F.);
#20119=ORIENTED_EDGE('',*,*,#14761,.T.);
#20120=ORIENTED_EDGE('',*,*,#14762,.T.);
#20121=ORIENTED_EDGE('',*,*,#14761,.F.);
#20122=ORIENTED_EDGE('',*,*,#14763,.F.);
#20123=ORIENTED_EDGE('',*,*,#14764,.T.);
#20124=ORIENTED_EDGE('',*,*,#14765,.T.);
#20125=ORIENTED_EDGE('',*,*,#14764,.F.);
#20126=ORIENTED_EDGE('',*,*,#14766,.F.);
#20127=ORIENTED_EDGE('',*,*,#14767,.T.);
#20128=ORIENTED_EDGE('',*,*,#14768,.T.);
#20129=ORIENTED_EDGE('',*,*,#14767,.F.);
#20130=ORIENTED_EDGE('',*,*,#14738,.T.);
#20131=ORIENTED_EDGE('',*,*,#14769,.F.);
#20132=ORIENTED_EDGE('',*,*,#14770,.T.);
#20133=ORIENTED_EDGE('',*,*,#14771,.T.);
#20134=ORIENTED_EDGE('',*,*,#14770,.F.);
#20135=ORIENTED_EDGE('',*,*,#14772,.F.);
#20136=ORIENTED_EDGE('',*,*,#14773,.T.);
#20137=ORIENTED_EDGE('',*,*,#14774,.T.);
#20138=ORIENTED_EDGE('',*,*,#14773,.F.);
#20139=ORIENTED_EDGE('',*,*,#14775,.F.);
#20140=ORIENTED_EDGE('',*,*,#14776,.T.);
#20141=ORIENTED_EDGE('',*,*,#14757,.T.);
#20142=ORIENTED_EDGE('',*,*,#14776,.F.);
#20143=ORIENTED_EDGE('',*,*,#14777,.T.);
#20144=ORIENTED_EDGE('',*,*,#14778,.F.);
#20145=ORIENTED_EDGE('',*,*,#14779,.T.);
#20146=ORIENTED_EDGE('',*,*,#14780,.F.);
#20147=ORIENTED_EDGE('',*,*,#14753,.F.);
#20148=ORIENTED_EDGE('',*,*,#14750,.F.);
#20149=ORIENTED_EDGE('',*,*,#14747,.F.);
#20150=ORIENTED_EDGE('',*,*,#14744,.F.);
#20151=ORIENTED_EDGE('',*,*,#14741,.F.);
#20152=ORIENTED_EDGE('',*,*,#14756,.F.);
#20153=ORIENTED_EDGE('',*,*,#14760,.T.);
#20154=ORIENTED_EDGE('',*,*,#14781,.F.);
#20155=ORIENTED_EDGE('',*,*,#14782,.F.);
#20156=ORIENTED_EDGE('',*,*,#14783,.F.);
#20157=ORIENTED_EDGE('',*,*,#14778,.T.);
#20158=ORIENTED_EDGE('',*,*,#14784,.F.);
#20159=ORIENTED_EDGE('',*,*,#14780,.T.);
#20160=ORIENTED_EDGE('',*,*,#14785,.F.);
#20161=ORIENTED_EDGE('',*,*,#14786,.F.);
#20162=ORIENTED_EDGE('',*,*,#14787,.F.);
#20163=ORIENTED_EDGE('',*,*,#14788,.F.);
#20164=ORIENTED_EDGE('',*,*,#14789,.F.);
#20165=ORIENTED_EDGE('',*,*,#14786,.T.);
#20166=ORIENTED_EDGE('',*,*,#14736,.T.);
#20167=ORIENTED_EDGE('',*,*,#14790,.F.);
#20168=ORIENTED_EDGE('',*,*,#14782,.T.);
#20169=ORIENTED_EDGE('',*,*,#14791,.F.);
#20170=ORIENTED_EDGE('',*,*,#14792,.F.);
#20171=ORIENTED_EDGE('',*,*,#14793,.F.);
#20172=ORIENTED_EDGE('',*,*,#14794,.F.);
#20173=ORIENTED_EDGE('',*,*,#14795,.F.);
#20174=ORIENTED_EDGE('',*,*,#14792,.T.);
#20175=ORIENTED_EDGE('',*,*,#14796,.F.);
#20176=ORIENTED_EDGE('',*,*,#14788,.T.);
#20177=ORIENTED_EDGE('',*,*,#14797,.F.);
#20178=ORIENTED_EDGE('',*,*,#14798,.F.);
#20179=ORIENTED_EDGE('',*,*,#14799,.F.);
#20180=ORIENTED_EDGE('',*,*,#14798,.T.);
#20181=ORIENTED_EDGE('',*,*,#14800,.F.);
#20182=ORIENTED_EDGE('',*,*,#14794,.T.);
#20183=ORIENTED_EDGE('',*,*,#14739,.T.);
#20184=ORIENTED_EDGE('',*,*,#14742,.T.);
#20185=ORIENTED_EDGE('',*,*,#14745,.T.);
#20186=ORIENTED_EDGE('',*,*,#14748,.T.);
#20187=ORIENTED_EDGE('',*,*,#14751,.T.);
#20188=ORIENTED_EDGE('',*,*,#14754,.T.);
#20189=ORIENTED_EDGE('',*,*,#14759,.F.);
#20190=ORIENTED_EDGE('',*,*,#14775,.T.);
#20191=ORIENTED_EDGE('',*,*,#14774,.F.);
#20192=ORIENTED_EDGE('',*,*,#14772,.T.);
#20193=ORIENTED_EDGE('',*,*,#14771,.F.);
#20194=ORIENTED_EDGE('',*,*,#14769,.T.);
#20195=ORIENTED_EDGE('',*,*,#14768,.F.);
#20196=ORIENTED_EDGE('',*,*,#14765,.F.);
#20197=ORIENTED_EDGE('',*,*,#14766,.T.);
#20198=ORIENTED_EDGE('',*,*,#14762,.F.);
#20199=ORIENTED_EDGE('',*,*,#14763,.T.);
#20200=ORIENTED_EDGE('',*,*,#14783,.T.);
#20201=ORIENTED_EDGE('',*,*,#14790,.T.);
#20202=ORIENTED_EDGE('',*,*,#14795,.T.);
#20203=ORIENTED_EDGE('',*,*,#14800,.T.);
#20204=ORIENTED_EDGE('',*,*,#14797,.T.);
#20205=ORIENTED_EDGE('',*,*,#14787,.T.);
#20206=ORIENTED_EDGE('',*,*,#14785,.T.);
#20207=ORIENTED_EDGE('',*,*,#14779,.F.);
#20208=ORIENTED_EDGE('',*,*,#14781,.T.);
#20209=ORIENTED_EDGE('',*,*,#14777,.F.);
#20210=ORIENTED_EDGE('',*,*,#14784,.T.);
#20211=ORIENTED_EDGE('',*,*,#14789,.T.);
#20212=ORIENTED_EDGE('',*,*,#14796,.T.);
#20213=ORIENTED_EDGE('',*,*,#14799,.T.);
#20214=ORIENTED_EDGE('',*,*,#14793,.T.);
#20215=ORIENTED_EDGE('',*,*,#14791,.T.);
#20216=ORIENTED_EDGE('',*,*,#14801,.F.);
#20217=ORIENTED_EDGE('',*,*,#14802,.T.);
#20218=ORIENTED_EDGE('',*,*,#14803,.T.);
#20219=ORIENTED_EDGE('',*,*,#14802,.F.);
#20220=ORIENTED_EDGE('',*,*,#14804,.F.);
#20221=ORIENTED_EDGE('',*,*,#14805,.T.);
#20222=ORIENTED_EDGE('',*,*,#14806,.T.);
#20223=ORIENTED_EDGE('',*,*,#14805,.F.);
#20224=ORIENTED_EDGE('',*,*,#14807,.F.);
#20225=ORIENTED_EDGE('',*,*,#14808,.T.);
#20226=ORIENTED_EDGE('',*,*,#14809,.T.);
#20227=ORIENTED_EDGE('',*,*,#14808,.F.);
#20228=ORIENTED_EDGE('',*,*,#14810,.F.);
#20229=ORIENTED_EDGE('',*,*,#14811,.T.);
#20230=ORIENTED_EDGE('',*,*,#14812,.T.);
#20231=ORIENTED_EDGE('',*,*,#14811,.F.);
#20232=ORIENTED_EDGE('',*,*,#14813,.F.);
#20233=ORIENTED_EDGE('',*,*,#14814,.T.);
#20234=ORIENTED_EDGE('',*,*,#14815,.T.);
#20235=ORIENTED_EDGE('',*,*,#14814,.F.);
#20236=ORIENTED_EDGE('',*,*,#14816,.F.);
#20237=ORIENTED_EDGE('',*,*,#14817,.T.);
#20238=ORIENTED_EDGE('',*,*,#14818,.T.);
#20239=ORIENTED_EDGE('',*,*,#14817,.F.);
#20240=ORIENTED_EDGE('',*,*,#14819,.F.);
#20241=ORIENTED_EDGE('',*,*,#14820,.T.);
#20242=ORIENTED_EDGE('',*,*,#14821,.T.);
#20243=ORIENTED_EDGE('',*,*,#14820,.F.);
#20244=ORIENTED_EDGE('',*,*,#14822,.T.);
#20245=ORIENTED_EDGE('',*,*,#14823,.F.);
#20246=ORIENTED_EDGE('',*,*,#14824,.F.);
#20247=ORIENTED_EDGE('',*,*,#14825,.T.);
#20248=ORIENTED_EDGE('',*,*,#14818,.F.);
#20249=ORIENTED_EDGE('',*,*,#14826,.T.);
#20250=ORIENTED_EDGE('',*,*,#14827,.F.);
#20251=ORIENTED_EDGE('',*,*,#14828,.F.);
#20252=ORIENTED_EDGE('',*,*,#14823,.T.);
#20253=ORIENTED_EDGE('',*,*,#14829,.T.);
#20254=ORIENTED_EDGE('',*,*,#14830,.F.);
#20255=ORIENTED_EDGE('',*,*,#14831,.F.);
#20256=ORIENTED_EDGE('',*,*,#14827,.T.);
#20257=ORIENTED_EDGE('',*,*,#14832,.T.);
#20258=ORIENTED_EDGE('',*,*,#14833,.F.);
#20259=ORIENTED_EDGE('',*,*,#14834,.F.);
#20260=ORIENTED_EDGE('',*,*,#14830,.T.);
#20261=ORIENTED_EDGE('',*,*,#14813,.T.);
#20262=ORIENTED_EDGE('',*,*,#14819,.T.);
#20263=ORIENTED_EDGE('',*,*,#14835,.T.);
#20264=ORIENTED_EDGE('',*,*,#14836,.F.);
#20265=ORIENTED_EDGE('',*,*,#14837,.F.);
#20266=ORIENTED_EDGE('',*,*,#14833,.T.);
#20267=ORIENTED_EDGE('',*,*,#14838,.T.);
#20268=ORIENTED_EDGE('',*,*,#14839,.F.);
#20269=ORIENTED_EDGE('',*,*,#14840,.F.);
#20270=ORIENTED_EDGE('',*,*,#14836,.T.);
#20271=ORIENTED_EDGE('',*,*,#14841,.T.);
#20272=ORIENTED_EDGE('',*,*,#14842,.F.);
#20273=ORIENTED_EDGE('',*,*,#14843,.F.);
#20274=ORIENTED_EDGE('',*,*,#14839,.T.);
#20275=ORIENTED_EDGE('',*,*,#14812,.F.);
#20276=ORIENTED_EDGE('',*,*,#14844,.T.);
#20277=ORIENTED_EDGE('',*,*,#14845,.F.);
#20278=ORIENTED_EDGE('',*,*,#14846,.F.);
#20279=ORIENTED_EDGE('',*,*,#14842,.T.);
#20280=ORIENTED_EDGE('',*,*,#14847,.T.);
#20281=ORIENTED_EDGE('',*,*,#14848,.F.);
#20282=ORIENTED_EDGE('',*,*,#14849,.F.);
#20283=ORIENTED_EDGE('',*,*,#14845,.T.);
#20284=ORIENTED_EDGE('',*,*,#14850,.T.);
#20285=ORIENTED_EDGE('',*,*,#14851,.F.);
#20286=ORIENTED_EDGE('',*,*,#14852,.F.);
#20287=ORIENTED_EDGE('',*,*,#14848,.T.);
#20288=ORIENTED_EDGE('',*,*,#14853,.T.);
#20289=ORIENTED_EDGE('',*,*,#14854,.F.);
#20290=ORIENTED_EDGE('',*,*,#14855,.F.);
#20291=ORIENTED_EDGE('',*,*,#14851,.T.);
#20292=ORIENTED_EDGE('',*,*,#14856,.T.);
#20293=ORIENTED_EDGE('',*,*,#14825,.F.);
#20294=ORIENTED_EDGE('',*,*,#14857,.F.);
#20295=ORIENTED_EDGE('',*,*,#14854,.T.);
#20296=ORIENTED_EDGE('',*,*,#14824,.T.);
#20297=ORIENTED_EDGE('',*,*,#14828,.T.);
#20298=ORIENTED_EDGE('',*,*,#14831,.T.);
#20299=ORIENTED_EDGE('',*,*,#14834,.T.);
#20300=ORIENTED_EDGE('',*,*,#14837,.T.);
#20301=ORIENTED_EDGE('',*,*,#14840,.T.);
#20302=ORIENTED_EDGE('',*,*,#14843,.T.);
#20303=ORIENTED_EDGE('',*,*,#14846,.T.);
#20304=ORIENTED_EDGE('',*,*,#14849,.T.);
#20305=ORIENTED_EDGE('',*,*,#14852,.T.);
#20306=ORIENTED_EDGE('',*,*,#14855,.T.);
#20307=ORIENTED_EDGE('',*,*,#14857,.T.);
#20308=ORIENTED_EDGE('',*,*,#14803,.F.);
#20309=ORIENTED_EDGE('',*,*,#14822,.F.);
#20310=ORIENTED_EDGE('',*,*,#14856,.F.);
#20311=ORIENTED_EDGE('',*,*,#14853,.F.);
#20312=ORIENTED_EDGE('',*,*,#14850,.F.);
#20313=ORIENTED_EDGE('',*,*,#14847,.F.);
#20314=ORIENTED_EDGE('',*,*,#14844,.F.);
#20315=ORIENTED_EDGE('',*,*,#14841,.F.);
#20316=ORIENTED_EDGE('',*,*,#14838,.F.);
#20317=ORIENTED_EDGE('',*,*,#14835,.F.);
#20318=ORIENTED_EDGE('',*,*,#14832,.F.);
#20319=ORIENTED_EDGE('',*,*,#14829,.F.);
#20320=ORIENTED_EDGE('',*,*,#14826,.F.);
#20321=ORIENTED_EDGE('',*,*,#14807,.T.);
#20322=ORIENTED_EDGE('',*,*,#14816,.T.);
#20323=ORIENTED_EDGE('',*,*,#14821,.F.);
#20324=ORIENTED_EDGE('',*,*,#14810,.T.);
#20325=ORIENTED_EDGE('',*,*,#14815,.F.);
#20326=ORIENTED_EDGE('',*,*,#14809,.F.);
#20327=ORIENTED_EDGE('',*,*,#14804,.T.);
#20328=ORIENTED_EDGE('',*,*,#14801,.T.);
#20329=ORIENTED_EDGE('',*,*,#14806,.F.);
#20330=ORIENTED_EDGE('',*,*,#14858,.T.);
#20331=ORIENTED_EDGE('',*,*,#14859,.T.);
#20332=ORIENTED_EDGE('',*,*,#14860,.F.);
#20333=ORIENTED_EDGE('',*,*,#14859,.F.);
#20334=ORIENTED_EDGE('',*,*,#14861,.T.);
#20335=ORIENTED_EDGE('',*,*,#14862,.T.);
#20336=ORIENTED_EDGE('',*,*,#14863,.F.);
#20337=ORIENTED_EDGE('',*,*,#14862,.F.);
#20338=ORIENTED_EDGE('',*,*,#14864,.F.);
#20339=ORIENTED_EDGE('',*,*,#14865,.T.);
#20340=ORIENTED_EDGE('',*,*,#14866,.T.);
#20341=ORIENTED_EDGE('',*,*,#14867,.F.);
#20342=ORIENTED_EDGE('',*,*,#14868,.F.);
#20343=ORIENTED_EDGE('',*,*,#14869,.T.);
#20344=ORIENTED_EDGE('',*,*,#14870,.T.);
#20345=ORIENTED_EDGE('',*,*,#14871,.F.);
#20346=ORIENTED_EDGE('',*,*,#14872,.T.);
#20347=ORIENTED_EDGE('',*,*,#14873,.T.);
#20348=ORIENTED_EDGE('',*,*,#14874,.T.);
#20349=ORIENTED_EDGE('',*,*,#14875,.T.);
#20350=ORIENTED_EDGE('',*,*,#14868,.T.);
#20351=ORIENTED_EDGE('',*,*,#14876,.T.);
#20352=ORIENTED_EDGE('',*,*,#14877,.T.);
#20353=ORIENTED_EDGE('',*,*,#14878,.T.);
#20354=ORIENTED_EDGE('',*,*,#14879,.T.);
#20355=ORIENTED_EDGE('',*,*,#14880,.T.);
#20356=ORIENTED_EDGE('',*,*,#14864,.T.);
#20357=ORIENTED_EDGE('',*,*,#14881,.T.);
#20358=ORIENTED_EDGE('',*,*,#14858,.F.);
#20359=ORIENTED_EDGE('',*,*,#14861,.F.);
#20360=ORIENTED_EDGE('',*,*,#14882,.F.);
#20361=ORIENTED_EDGE('',*,*,#14883,.F.);
#20362=ORIENTED_EDGE('',*,*,#14866,.F.);
#20363=ORIENTED_EDGE('',*,*,#14884,.F.);
#20364=ORIENTED_EDGE('',*,*,#14885,.F.);
#20365=ORIENTED_EDGE('',*,*,#14886,.F.);
#20366=ORIENTED_EDGE('',*,*,#14887,.F.);
#20367=ORIENTED_EDGE('',*,*,#14888,.F.);
#20368=ORIENTED_EDGE('',*,*,#14870,.F.);
#20369=ORIENTED_EDGE('',*,*,#14889,.F.);
#20370=ORIENTED_EDGE('',*,*,#14890,.F.);
#20371=ORIENTED_EDGE('',*,*,#14891,.F.);
#20372=ORIENTED_EDGE('',*,*,#14863,.T.);
#20373=ORIENTED_EDGE('',*,*,#14860,.T.);
#20374=ORIENTED_EDGE('',*,*,#14882,.T.);
#20375=ORIENTED_EDGE('',*,*,#14892,.F.);
#20376=ORIENTED_EDGE('',*,*,#14872,.F.);
#20377=ORIENTED_EDGE('',*,*,#14893,.T.);
#20378=ORIENTED_EDGE('',*,*,#14891,.T.);
#20379=ORIENTED_EDGE('',*,*,#14894,.F.);
#20380=ORIENTED_EDGE('',*,*,#14873,.F.);
#20381=ORIENTED_EDGE('',*,*,#14892,.T.);
#20382=ORIENTED_EDGE('',*,*,#14890,.T.);
#20383=ORIENTED_EDGE('',*,*,#14895,.F.);
#20384=ORIENTED_EDGE('',*,*,#14874,.F.);
#20385=ORIENTED_EDGE('',*,*,#14894,.T.);
#20386=ORIENTED_EDGE('',*,*,#14889,.T.);
#20387=ORIENTED_EDGE('',*,*,#14869,.F.);
#20388=ORIENTED_EDGE('',*,*,#14875,.F.);
#20389=ORIENTED_EDGE('',*,*,#14895,.T.);
#20390=ORIENTED_EDGE('',*,*,#14888,.T.);
#20391=ORIENTED_EDGE('',*,*,#14896,.F.);
#20392=ORIENTED_EDGE('',*,*,#14876,.F.);
#20393=ORIENTED_EDGE('',*,*,#14871,.T.);
#20394=ORIENTED_EDGE('',*,*,#14887,.T.);
#20395=ORIENTED_EDGE('',*,*,#14897,.F.);
#20396=ORIENTED_EDGE('',*,*,#14877,.F.);
#20397=ORIENTED_EDGE('',*,*,#14896,.T.);
#20398=ORIENTED_EDGE('',*,*,#14886,.T.);
#20399=ORIENTED_EDGE('',*,*,#14898,.F.);
#20400=ORIENTED_EDGE('',*,*,#14878,.F.);
#20401=ORIENTED_EDGE('',*,*,#14897,.T.);
#20402=ORIENTED_EDGE('',*,*,#14885,.T.);
#20403=ORIENTED_EDGE('',*,*,#14899,.F.);
#20404=ORIENTED_EDGE('',*,*,#14879,.F.);
#20405=ORIENTED_EDGE('',*,*,#14898,.T.);
#20406=ORIENTED_EDGE('',*,*,#14884,.T.);
#20407=ORIENTED_EDGE('',*,*,#14865,.F.);
#20408=ORIENTED_EDGE('',*,*,#14880,.F.);
#20409=ORIENTED_EDGE('',*,*,#14899,.T.);
#20410=ORIENTED_EDGE('',*,*,#14883,.T.);
#20411=ORIENTED_EDGE('',*,*,#14893,.F.);
#20412=ORIENTED_EDGE('',*,*,#14881,.F.);
#20413=ORIENTED_EDGE('',*,*,#14867,.T.);
#20414=ORIENTED_EDGE('',*,*,#14900,.F.);
#20415=ORIENTED_EDGE('',*,*,#14901,.T.);
#20416=ORIENTED_EDGE('',*,*,#14902,.T.);
#20417=ORIENTED_EDGE('',*,*,#14901,.F.);
#20418=ORIENTED_EDGE('',*,*,#14903,.F.);
#20419=ORIENTED_EDGE('',*,*,#14904,.T.);
#20420=ORIENTED_EDGE('',*,*,#14905,.T.);
#20421=ORIENTED_EDGE('',*,*,#14904,.F.);
#20422=ORIENTED_EDGE('',*,*,#14906,.F.);
#20423=ORIENTED_EDGE('',*,*,#14907,.T.);
#20424=ORIENTED_EDGE('',*,*,#14908,.T.);
#20425=ORIENTED_EDGE('',*,*,#14907,.F.);
#20426=ORIENTED_EDGE('',*,*,#14909,.F.);
#20427=ORIENTED_EDGE('',*,*,#14910,.T.);
#20428=ORIENTED_EDGE('',*,*,#14911,.T.);
#20429=ORIENTED_EDGE('',*,*,#14910,.F.);
#20430=ORIENTED_EDGE('',*,*,#14912,.F.);
#20431=ORIENTED_EDGE('',*,*,#14913,.T.);
#20432=ORIENTED_EDGE('',*,*,#14914,.T.);
#20433=ORIENTED_EDGE('',*,*,#14913,.F.);
#20434=ORIENTED_EDGE('',*,*,#14915,.T.);
#20435=ORIENTED_EDGE('',*,*,#14916,.T.);
#20436=ORIENTED_EDGE('',*,*,#14917,.F.);
#20437=ORIENTED_EDGE('',*,*,#14916,.F.);
#20438=ORIENTED_EDGE('',*,*,#14918,.T.);
#20439=ORIENTED_EDGE('',*,*,#14919,.T.);
#20440=ORIENTED_EDGE('',*,*,#14920,.F.);
#20441=ORIENTED_EDGE('',*,*,#14919,.F.);
#20442=ORIENTED_EDGE('',*,*,#14921,.T.);
#20443=ORIENTED_EDGE('',*,*,#14922,.T.);
#20444=ORIENTED_EDGE('',*,*,#14923,.F.);
#20445=ORIENTED_EDGE('',*,*,#14922,.F.);
#20446=ORIENTED_EDGE('',*,*,#14924,.T.);
#20447=ORIENTED_EDGE('',*,*,#14925,.T.);
#20448=ORIENTED_EDGE('',*,*,#14926,.F.);
#20449=ORIENTED_EDGE('',*,*,#14925,.F.);
#20450=ORIENTED_EDGE('',*,*,#14927,.T.);
#20451=ORIENTED_EDGE('',*,*,#14928,.T.);
#20452=ORIENTED_EDGE('',*,*,#14929,.T.);
#20453=ORIENTED_EDGE('',*,*,#14928,.F.);
#20454=ORIENTED_EDGE('',*,*,#14930,.T.);
#20455=ORIENTED_EDGE('',*,*,#14931,.T.);
#20456=ORIENTED_EDGE('',*,*,#14932,.T.);
#20457=ORIENTED_EDGE('',*,*,#14931,.F.);
#20458=ORIENTED_EDGE('',*,*,#14933,.T.);
#20459=ORIENTED_EDGE('',*,*,#14934,.T.);
#20460=ORIENTED_EDGE('',*,*,#14935,.T.);
#20461=ORIENTED_EDGE('',*,*,#14934,.F.);
#20462=ORIENTED_EDGE('',*,*,#14936,.T.);
#20463=ORIENTED_EDGE('',*,*,#14937,.T.);
#20464=ORIENTED_EDGE('',*,*,#14938,.T.);
#20465=ORIENTED_EDGE('',*,*,#14937,.F.);
#20466=ORIENTED_EDGE('',*,*,#14939,.F.);
#20467=ORIENTED_EDGE('',*,*,#14940,.T.);
#20468=ORIENTED_EDGE('',*,*,#14941,.T.);
#20469=ORIENTED_EDGE('',*,*,#14940,.F.);
#20470=ORIENTED_EDGE('',*,*,#14942,.F.);
#20471=ORIENTED_EDGE('',*,*,#14943,.T.);
#20472=ORIENTED_EDGE('',*,*,#14944,.T.);
#20473=ORIENTED_EDGE('',*,*,#14943,.F.);
#20474=ORIENTED_EDGE('',*,*,#14945,.F.);
#20475=ORIENTED_EDGE('',*,*,#14946,.T.);
#20476=ORIENTED_EDGE('',*,*,#14947,.T.);
#20477=ORIENTED_EDGE('',*,*,#14946,.F.);
#20478=ORIENTED_EDGE('',*,*,#14948,.F.);
#20479=ORIENTED_EDGE('',*,*,#14949,.T.);
#20480=ORIENTED_EDGE('',*,*,#14950,.T.);
#20481=ORIENTED_EDGE('',*,*,#14949,.F.);
#20482=ORIENTED_EDGE('',*,*,#14951,.F.);
#20483=ORIENTED_EDGE('',*,*,#14952,.T.);
#20484=ORIENTED_EDGE('',*,*,#14953,.T.);
#20485=ORIENTED_EDGE('',*,*,#14952,.F.);
#20486=ORIENTED_EDGE('',*,*,#14954,.F.);
#20487=ORIENTED_EDGE('',*,*,#14955,.T.);
#20488=ORIENTED_EDGE('',*,*,#14956,.T.);
#20489=ORIENTED_EDGE('',*,*,#14955,.F.);
#20490=ORIENTED_EDGE('',*,*,#14957,.F.);
#20491=ORIENTED_EDGE('',*,*,#14958,.T.);
#20492=ORIENTED_EDGE('',*,*,#14959,.T.);
#20493=ORIENTED_EDGE('',*,*,#14958,.F.);
#20494=ORIENTED_EDGE('',*,*,#14960,.F.);
#20495=ORIENTED_EDGE('',*,*,#14961,.T.);
#20496=ORIENTED_EDGE('',*,*,#14962,.T.);
#20497=ORIENTED_EDGE('',*,*,#14961,.F.);
#20498=ORIENTED_EDGE('',*,*,#14932,.F.);
#20499=ORIENTED_EDGE('',*,*,#14915,.F.);
#20500=ORIENTED_EDGE('',*,*,#14929,.F.);
#20501=ORIENTED_EDGE('',*,*,#14918,.F.);
#20502=ORIENTED_EDGE('',*,*,#14935,.F.);
#20503=ORIENTED_EDGE('',*,*,#14921,.F.);
#20504=ORIENTED_EDGE('',*,*,#14938,.F.);
#20505=ORIENTED_EDGE('',*,*,#14924,.F.);
#20506=ORIENTED_EDGE('',*,*,#14963,.T.);
#20507=ORIENTED_EDGE('',*,*,#14964,.T.);
#20508=ORIENTED_EDGE('',*,*,#14965,.T.);
#20509=ORIENTED_EDGE('',*,*,#14966,.T.);
#20510=ORIENTED_EDGE('',*,*,#14967,.T.);
#20511=ORIENTED_EDGE('',*,*,#14968,.T.);
#20512=ORIENTED_EDGE('',*,*,#14969,.T.);
#20513=ORIENTED_EDGE('',*,*,#14970,.T.);
#20514=ORIENTED_EDGE('',*,*,#14971,.T.);
#20515=ORIENTED_EDGE('',*,*,#14972,.T.);
#20516=ORIENTED_EDGE('',*,*,#14973,.T.);
#20517=ORIENTED_EDGE('',*,*,#14974,.T.);
#20518=ORIENTED_EDGE('',*,*,#14975,.F.);
#20519=ORIENTED_EDGE('',*,*,#14976,.F.);
#20520=ORIENTED_EDGE('',*,*,#14977,.F.);
#20521=ORIENTED_EDGE('',*,*,#14978,.F.);
#20522=ORIENTED_EDGE('',*,*,#14979,.F.);
#20523=ORIENTED_EDGE('',*,*,#14980,.F.);
#20524=ORIENTED_EDGE('',*,*,#14981,.F.);
#20525=ORIENTED_EDGE('',*,*,#14982,.F.);
#20526=ORIENTED_EDGE('',*,*,#14983,.T.);
#20527=ORIENTED_EDGE('',*,*,#14984,.F.);
#20528=ORIENTED_EDGE('',*,*,#14963,.F.);
#20529=ORIENTED_EDGE('',*,*,#14985,.T.);
#20530=ORIENTED_EDGE('',*,*,#14947,.F.);
#20531=ORIENTED_EDGE('',*,*,#14959,.F.);
#20532=ORIENTED_EDGE('',*,*,#14986,.T.);
#20533=ORIENTED_EDGE('',*,*,#14987,.F.);
#20534=ORIENTED_EDGE('',*,*,#14964,.F.);
#20535=ORIENTED_EDGE('',*,*,#14984,.T.);
#20536=ORIENTED_EDGE('',*,*,#14988,.T.);
#20537=ORIENTED_EDGE('',*,*,#14989,.F.);
#20538=ORIENTED_EDGE('',*,*,#14965,.F.);
#20539=ORIENTED_EDGE('',*,*,#14987,.T.);
#20540=ORIENTED_EDGE('',*,*,#14990,.T.);
#20541=ORIENTED_EDGE('',*,*,#14991,.F.);
#20542=ORIENTED_EDGE('',*,*,#14966,.F.);
#20543=ORIENTED_EDGE('',*,*,#14989,.T.);
#20544=ORIENTED_EDGE('',*,*,#14942,.T.);
#20545=ORIENTED_EDGE('',*,*,#14948,.T.);
#20546=ORIENTED_EDGE('',*,*,#14954,.T.);
#20547=ORIENTED_EDGE('',*,*,#14960,.T.);
#20548=ORIENTED_EDGE('',*,*,#14992,.T.);
#20549=ORIENTED_EDGE('',*,*,#14993,.F.);
#20550=ORIENTED_EDGE('',*,*,#14967,.F.);
#20551=ORIENTED_EDGE('',*,*,#14991,.T.);
#20552=ORIENTED_EDGE('',*,*,#14994,.T.);
#20553=ORIENTED_EDGE('',*,*,#14995,.F.);
#20554=ORIENTED_EDGE('',*,*,#14968,.F.);
#20555=ORIENTED_EDGE('',*,*,#14993,.T.);
#20556=ORIENTED_EDGE('',*,*,#14996,.T.);
#20557=ORIENTED_EDGE('',*,*,#14997,.F.);
#20558=ORIENTED_EDGE('',*,*,#14969,.F.);
#20559=ORIENTED_EDGE('',*,*,#14995,.T.);
#20560=ORIENTED_EDGE('',*,*,#14941,.F.);
#20561=ORIENTED_EDGE('',*,*,#14953,.F.);
#20562=ORIENTED_EDGE('',*,*,#14998,.T.);
#20563=ORIENTED_EDGE('',*,*,#14999,.F.);
#20564=ORIENTED_EDGE('',*,*,#14970,.F.);
#20565=ORIENTED_EDGE('',*,*,#14997,.T.);
#20566=ORIENTED_EDGE('',*,*,#15000,.T.);
#20567=ORIENTED_EDGE('',*,*,#15001,.F.);
#20568=ORIENTED_EDGE('',*,*,#14971,.F.);
#20569=ORIENTED_EDGE('',*,*,#14999,.T.);
#20570=ORIENTED_EDGE('',*,*,#15002,.T.);
#20571=ORIENTED_EDGE('',*,*,#15003,.F.);
#20572=ORIENTED_EDGE('',*,*,#14972,.F.);
#20573=ORIENTED_EDGE('',*,*,#15001,.T.);
#20574=ORIENTED_EDGE('',*,*,#15004,.T.);
#20575=ORIENTED_EDGE('',*,*,#15005,.F.);
#20576=ORIENTED_EDGE('',*,*,#14973,.F.);
#20577=ORIENTED_EDGE('',*,*,#15003,.T.);
#20578=ORIENTED_EDGE('',*,*,#15006,.T.);
#20579=ORIENTED_EDGE('',*,*,#14985,.F.);
#20580=ORIENTED_EDGE('',*,*,#14974,.F.);
#20581=ORIENTED_EDGE('',*,*,#15005,.T.);
#20582=ORIENTED_EDGE('',*,*,#14983,.F.);
#20583=ORIENTED_EDGE('',*,*,#15006,.F.);
#20584=ORIENTED_EDGE('',*,*,#15004,.F.);
#20585=ORIENTED_EDGE('',*,*,#15002,.F.);
#20586=ORIENTED_EDGE('',*,*,#15000,.F.);
#20587=ORIENTED_EDGE('',*,*,#14998,.F.);
#20588=ORIENTED_EDGE('',*,*,#14996,.F.);
#20589=ORIENTED_EDGE('',*,*,#14994,.F.);
#20590=ORIENTED_EDGE('',*,*,#14992,.F.);
#20591=ORIENTED_EDGE('',*,*,#14990,.F.);
#20592=ORIENTED_EDGE('',*,*,#14988,.F.);
#20593=ORIENTED_EDGE('',*,*,#14986,.F.);
#20594=ORIENTED_EDGE('',*,*,#14912,.T.);
#20595=ORIENTED_EDGE('',*,*,#14957,.T.);
#20596=ORIENTED_EDGE('',*,*,#14962,.F.);
#20597=ORIENTED_EDGE('',*,*,#14951,.T.);
#20598=ORIENTED_EDGE('',*,*,#14956,.F.);
#20599=ORIENTED_EDGE('',*,*,#14945,.T.);
#20600=ORIENTED_EDGE('',*,*,#14950,.F.);
#20601=ORIENTED_EDGE('',*,*,#14939,.T.);
#20602=ORIENTED_EDGE('',*,*,#14944,.F.);
#20603=ORIENTED_EDGE('',*,*,#15007,.T.);
#20604=ORIENTED_EDGE('',*,*,#15008,.T.);
#20605=ORIENTED_EDGE('',*,*,#15009,.T.);
#20606=ORIENTED_EDGE('',*,*,#15010,.T.);
#20607=ORIENTED_EDGE('',*,*,#15011,.T.);
#20608=ORIENTED_EDGE('',*,*,#15012,.T.);
#20609=ORIENTED_EDGE('',*,*,#15013,.T.);
#20610=ORIENTED_EDGE('',*,*,#15014,.T.);
#20611=ORIENTED_EDGE('',*,*,#14936,.F.);
#20612=ORIENTED_EDGE('',*,*,#14933,.F.);
#20613=ORIENTED_EDGE('',*,*,#14930,.F.);
#20614=ORIENTED_EDGE('',*,*,#14927,.F.);
#20615=ORIENTED_EDGE('',*,*,#14902,.F.);
#20616=ORIENTED_EDGE('',*,*,#14976,.T.);
#20617=ORIENTED_EDGE('',*,*,#15015,.F.);
#20618=ORIENTED_EDGE('',*,*,#15007,.F.);
#20619=ORIENTED_EDGE('',*,*,#15016,.T.);
#20620=ORIENTED_EDGE('',*,*,#14975,.T.);
#20621=ORIENTED_EDGE('',*,*,#15017,.F.);
#20622=ORIENTED_EDGE('',*,*,#15008,.F.);
#20623=ORIENTED_EDGE('',*,*,#15015,.T.);
#20624=ORIENTED_EDGE('',*,*,#14982,.T.);
#20625=ORIENTED_EDGE('',*,*,#15018,.F.);
#20626=ORIENTED_EDGE('',*,*,#15009,.F.);
#20627=ORIENTED_EDGE('',*,*,#15017,.T.);
#20628=ORIENTED_EDGE('',*,*,#14981,.T.);
#20629=ORIENTED_EDGE('',*,*,#15019,.F.);
#20630=ORIENTED_EDGE('',*,*,#15010,.F.);
#20631=ORIENTED_EDGE('',*,*,#15018,.T.);
#20632=ORIENTED_EDGE('',*,*,#14980,.T.);
#20633=ORIENTED_EDGE('',*,*,#15020,.F.);
#20634=ORIENTED_EDGE('',*,*,#15011,.F.);
#20635=ORIENTED_EDGE('',*,*,#15019,.T.);
#20636=ORIENTED_EDGE('',*,*,#14979,.T.);
#20637=ORIENTED_EDGE('',*,*,#15021,.F.);
#20638=ORIENTED_EDGE('',*,*,#15012,.F.);
#20639=ORIENTED_EDGE('',*,*,#15020,.T.);
#20640=ORIENTED_EDGE('',*,*,#14978,.T.);
#20641=ORIENTED_EDGE('',*,*,#15022,.F.);
#20642=ORIENTED_EDGE('',*,*,#15013,.F.);
#20643=ORIENTED_EDGE('',*,*,#15021,.T.);
#20644=ORIENTED_EDGE('',*,*,#14977,.T.);
#20645=ORIENTED_EDGE('',*,*,#15016,.F.);
#20646=ORIENTED_EDGE('',*,*,#15014,.F.);
#20647=ORIENTED_EDGE('',*,*,#15022,.T.);
#20648=ORIENTED_EDGE('',*,*,#14926,.T.);
#20649=ORIENTED_EDGE('',*,*,#15023,.F.);
#20650=ORIENTED_EDGE('',*,*,#15024,.F.);
#20651=ORIENTED_EDGE('',*,*,#15025,.F.);
#20652=ORIENTED_EDGE('',*,*,#15026,.F.);
#20653=ORIENTED_EDGE('',*,*,#15027,.F.);
#20654=ORIENTED_EDGE('',*,*,#15028,.F.);
#20655=ORIENTED_EDGE('',*,*,#14923,.T.);
#20656=ORIENTED_EDGE('',*,*,#15029,.F.);
#20657=ORIENTED_EDGE('',*,*,#15030,.F.);
#20658=ORIENTED_EDGE('',*,*,#15031,.F.);
#20659=ORIENTED_EDGE('',*,*,#15032,.F.);
#20660=ORIENTED_EDGE('',*,*,#15033,.F.);
#20661=ORIENTED_EDGE('',*,*,#15034,.F.);
#20662=ORIENTED_EDGE('',*,*,#14920,.T.);
#20663=ORIENTED_EDGE('',*,*,#15035,.F.);
#20664=ORIENTED_EDGE('',*,*,#15036,.F.);
#20665=ORIENTED_EDGE('',*,*,#15037,.F.);
#20666=ORIENTED_EDGE('',*,*,#15038,.F.);
#20667=ORIENTED_EDGE('',*,*,#15039,.F.);
#20668=ORIENTED_EDGE('',*,*,#15040,.F.);
#20669=ORIENTED_EDGE('',*,*,#14917,.T.);
#20670=ORIENTED_EDGE('',*,*,#15041,.F.);
#20671=ORIENTED_EDGE('',*,*,#15042,.F.);
#20672=ORIENTED_EDGE('',*,*,#15043,.F.);
#20673=ORIENTED_EDGE('',*,*,#15044,.F.);
#20674=ORIENTED_EDGE('',*,*,#15045,.F.);
#20675=ORIENTED_EDGE('',*,*,#15046,.F.);
#20676=ORIENTED_EDGE('',*,*,#15023,.T.);
#20677=ORIENTED_EDGE('',*,*,#15047,.F.);
#20678=ORIENTED_EDGE('',*,*,#15048,.F.);
#20679=ORIENTED_EDGE('',*,*,#15049,.T.);
#20680=ORIENTED_EDGE('',*,*,#15024,.T.);
#20681=ORIENTED_EDGE('',*,*,#15049,.F.);
#20682=ORIENTED_EDGE('',*,*,#15050,.F.);
#20683=ORIENTED_EDGE('',*,*,#15051,.T.);
#20684=ORIENTED_EDGE('',*,*,#15025,.T.);
#20685=ORIENTED_EDGE('',*,*,#15051,.F.);
#20686=ORIENTED_EDGE('',*,*,#15052,.F.);
#20687=ORIENTED_EDGE('',*,*,#15053,.T.);
#20688=ORIENTED_EDGE('',*,*,#15026,.T.);
#20689=ORIENTED_EDGE('',*,*,#15053,.F.);
#20690=ORIENTED_EDGE('',*,*,#15054,.F.);
#20691=ORIENTED_EDGE('',*,*,#15055,.T.);
#20692=ORIENTED_EDGE('',*,*,#15027,.T.);
#20693=ORIENTED_EDGE('',*,*,#15055,.F.);
#20694=ORIENTED_EDGE('',*,*,#15056,.F.);
#20695=ORIENTED_EDGE('',*,*,#15057,.T.);
#20696=ORIENTED_EDGE('',*,*,#15028,.T.);
#20697=ORIENTED_EDGE('',*,*,#15057,.F.);
#20698=ORIENTED_EDGE('',*,*,#15058,.F.);
#20699=ORIENTED_EDGE('',*,*,#15047,.T.);
#20700=ORIENTED_EDGE('',*,*,#15048,.T.);
#20701=ORIENTED_EDGE('',*,*,#15058,.T.);
#20702=ORIENTED_EDGE('',*,*,#15056,.T.);
#20703=ORIENTED_EDGE('',*,*,#15054,.T.);
#20704=ORIENTED_EDGE('',*,*,#15052,.T.);
#20705=ORIENTED_EDGE('',*,*,#15050,.T.);
#20706=ORIENTED_EDGE('',*,*,#15029,.T.);
#20707=ORIENTED_EDGE('',*,*,#15059,.F.);
#20708=ORIENTED_EDGE('',*,*,#15060,.F.);
#20709=ORIENTED_EDGE('',*,*,#15061,.T.);
#20710=ORIENTED_EDGE('',*,*,#15030,.T.);
#20711=ORIENTED_EDGE('',*,*,#15061,.F.);
#20712=ORIENTED_EDGE('',*,*,#15062,.F.);
#20713=ORIENTED_EDGE('',*,*,#15063,.T.);
#20714=ORIENTED_EDGE('',*,*,#15031,.T.);
#20715=ORIENTED_EDGE('',*,*,#15063,.F.);
#20716=ORIENTED_EDGE('',*,*,#15064,.F.);
#20717=ORIENTED_EDGE('',*,*,#15065,.T.);
#20718=ORIENTED_EDGE('',*,*,#15032,.T.);
#20719=ORIENTED_EDGE('',*,*,#15065,.F.);
#20720=ORIENTED_EDGE('',*,*,#15066,.F.);
#20721=ORIENTED_EDGE('',*,*,#15067,.T.);
#20722=ORIENTED_EDGE('',*,*,#15033,.T.);
#20723=ORIENTED_EDGE('',*,*,#15067,.F.);
#20724=ORIENTED_EDGE('',*,*,#15068,.F.);
#20725=ORIENTED_EDGE('',*,*,#15069,.T.);
#20726=ORIENTED_EDGE('',*,*,#15034,.T.);
#20727=ORIENTED_EDGE('',*,*,#15069,.F.);
#20728=ORIENTED_EDGE('',*,*,#15070,.F.);
#20729=ORIENTED_EDGE('',*,*,#15059,.T.);
#20730=ORIENTED_EDGE('',*,*,#15060,.T.);
#20731=ORIENTED_EDGE('',*,*,#15070,.T.);
#20732=ORIENTED_EDGE('',*,*,#15068,.T.);
#20733=ORIENTED_EDGE('',*,*,#15066,.T.);
#20734=ORIENTED_EDGE('',*,*,#15064,.T.);
#20735=ORIENTED_EDGE('',*,*,#15062,.T.);
#20736=ORIENTED_EDGE('',*,*,#15041,.T.);
#20737=ORIENTED_EDGE('',*,*,#15071,.F.);
#20738=ORIENTED_EDGE('',*,*,#15072,.F.);
#20739=ORIENTED_EDGE('',*,*,#15073,.T.);
#20740=ORIENTED_EDGE('',*,*,#15042,.T.);
#20741=ORIENTED_EDGE('',*,*,#15073,.F.);
#20742=ORIENTED_EDGE('',*,*,#15074,.F.);
#20743=ORIENTED_EDGE('',*,*,#15075,.T.);
#20744=ORIENTED_EDGE('',*,*,#15043,.T.);
#20745=ORIENTED_EDGE('',*,*,#15075,.F.);
#20746=ORIENTED_EDGE('',*,*,#15076,.F.);
#20747=ORIENTED_EDGE('',*,*,#15077,.T.);
#20748=ORIENTED_EDGE('',*,*,#15044,.T.);
#20749=ORIENTED_EDGE('',*,*,#15077,.F.);
#20750=ORIENTED_EDGE('',*,*,#15078,.F.);
#20751=ORIENTED_EDGE('',*,*,#15079,.T.);
#20752=ORIENTED_EDGE('',*,*,#15045,.T.);
#20753=ORIENTED_EDGE('',*,*,#15079,.F.);
#20754=ORIENTED_EDGE('',*,*,#15080,.F.);
#20755=ORIENTED_EDGE('',*,*,#15081,.T.);
#20756=ORIENTED_EDGE('',*,*,#15046,.T.);
#20757=ORIENTED_EDGE('',*,*,#15081,.F.);
#20758=ORIENTED_EDGE('',*,*,#15082,.F.);
#20759=ORIENTED_EDGE('',*,*,#15071,.T.);
#20760=ORIENTED_EDGE('',*,*,#15072,.T.);
#20761=ORIENTED_EDGE('',*,*,#15082,.T.);
#20762=ORIENTED_EDGE('',*,*,#15080,.T.);
#20763=ORIENTED_EDGE('',*,*,#15078,.T.);
#20764=ORIENTED_EDGE('',*,*,#15076,.T.);
#20765=ORIENTED_EDGE('',*,*,#15074,.T.);
#20766=ORIENTED_EDGE('',*,*,#15035,.T.);
#20767=ORIENTED_EDGE('',*,*,#15083,.F.);
#20768=ORIENTED_EDGE('',*,*,#15084,.F.);
#20769=ORIENTED_EDGE('',*,*,#15085,.T.);
#20770=ORIENTED_EDGE('',*,*,#15036,.T.);
#20771=ORIENTED_EDGE('',*,*,#15085,.F.);
#20772=ORIENTED_EDGE('',*,*,#15086,.F.);
#20773=ORIENTED_EDGE('',*,*,#15087,.T.);
#20774=ORIENTED_EDGE('',*,*,#15037,.T.);
#20775=ORIENTED_EDGE('',*,*,#15087,.F.);
#20776=ORIENTED_EDGE('',*,*,#15088,.F.);
#20777=ORIENTED_EDGE('',*,*,#15089,.T.);
#20778=ORIENTED_EDGE('',*,*,#15038,.T.);
#20779=ORIENTED_EDGE('',*,*,#15089,.F.);
#20780=ORIENTED_EDGE('',*,*,#15090,.F.);
#20781=ORIENTED_EDGE('',*,*,#15091,.T.);
#20782=ORIENTED_EDGE('',*,*,#15039,.T.);
#20783=ORIENTED_EDGE('',*,*,#15091,.F.);
#20784=ORIENTED_EDGE('',*,*,#15092,.F.);
#20785=ORIENTED_EDGE('',*,*,#15093,.T.);
#20786=ORIENTED_EDGE('',*,*,#15040,.T.);
#20787=ORIENTED_EDGE('',*,*,#15093,.F.);
#20788=ORIENTED_EDGE('',*,*,#15094,.F.);
#20789=ORIENTED_EDGE('',*,*,#15083,.T.);
#20790=ORIENTED_EDGE('',*,*,#15084,.T.);
#20791=ORIENTED_EDGE('',*,*,#15094,.T.);
#20792=ORIENTED_EDGE('',*,*,#15092,.T.);
#20793=ORIENTED_EDGE('',*,*,#15090,.T.);
#20794=ORIENTED_EDGE('',*,*,#15088,.T.);
#20795=ORIENTED_EDGE('',*,*,#15086,.T.);
#20796=ORIENTED_EDGE('',*,*,#14914,.F.);
#20797=ORIENTED_EDGE('',*,*,#14909,.T.);
#20798=ORIENTED_EDGE('',*,*,#14911,.F.);
#20799=ORIENTED_EDGE('',*,*,#14906,.T.);
#20800=ORIENTED_EDGE('',*,*,#14903,.T.);
#20801=ORIENTED_EDGE('',*,*,#14908,.F.);
#20802=ORIENTED_EDGE('',*,*,#14900,.T.);
#20803=ORIENTED_EDGE('',*,*,#14905,.F.);
#20804=ORIENTED_EDGE('',*,*,#15095,.T.);
#20805=ORIENTED_EDGE('',*,*,#15096,.F.);
#20806=ORIENTED_EDGE('',*,*,#15097,.F.);
#20807=ORIENTED_EDGE('',*,*,#15098,.F.);
#20808=ORIENTED_EDGE('',*,*,#15099,.F.);
#20809=ORIENTED_EDGE('',*,*,#15100,.F.);
#20810=ORIENTED_EDGE('',*,*,#15101,.F.);
#20811=ORIENTED_EDGE('',*,*,#15095,.F.);
#20812=ORIENTED_EDGE('',*,*,#15102,.T.);
#20813=ORIENTED_EDGE('',*,*,#15103,.T.);
#20814=ORIENTED_EDGE('',*,*,#15104,.T.);
#20815=ORIENTED_EDGE('',*,*,#15103,.F.);
#20816=ORIENTED_EDGE('',*,*,#15105,.T.);
#20817=ORIENTED_EDGE('',*,*,#15104,.F.);
#20818=ORIENTED_EDGE('',*,*,#15106,.T.);
#20819=ORIENTED_EDGE('',*,*,#15107,.T.);
#20820=ORIENTED_EDGE('',*,*,#15108,.T.);
#20821=ORIENTED_EDGE('',*,*,#15106,.F.);
#20822=ORIENTED_EDGE('',*,*,#15109,.T.);
#20823=ORIENTED_EDGE('',*,*,#15110,.T.);
#20824=ORIENTED_EDGE('',*,*,#15111,.F.);
#20825=ORIENTED_EDGE('',*,*,#15110,.F.);
#20826=ORIENTED_EDGE('',*,*,#15112,.T.);
#20827=ORIENTED_EDGE('',*,*,#15109,.F.);
#20828=ORIENTED_EDGE('',*,*,#15113,.T.);
#20829=ORIENTED_EDGE('',*,*,#15114,.T.);
#20830=ORIENTED_EDGE('',*,*,#15115,.T.);
#20831=ORIENTED_EDGE('',*,*,#15113,.F.);
#20832=ORIENTED_EDGE('',*,*,#15112,.F.);
#20833=ORIENTED_EDGE('',*,*,#15116,.T.);
#20834=ORIENTED_EDGE('',*,*,#15117,.T.);
#20835=ORIENTED_EDGE('',*,*,#15118,.F.);
#20836=ORIENTED_EDGE('',*,*,#15117,.F.);
#20837=ORIENTED_EDGE('',*,*,#15119,.T.);
#20838=ORIENTED_EDGE('',*,*,#15120,.F.);
#20839=ORIENTED_EDGE('',*,*,#15121,.T.);
#20840=ORIENTED_EDGE('',*,*,#15122,.T.);
#20841=ORIENTED_EDGE('',*,*,#15121,.F.);
#20842=ORIENTED_EDGE('',*,*,#15123,.T.);
#20843=ORIENTED_EDGE('',*,*,#15124,.T.);
#20844=ORIENTED_EDGE('',*,*,#15125,.F.);
#20845=ORIENTED_EDGE('',*,*,#15126,.T.);
#20846=ORIENTED_EDGE('',*,*,#15127,.F.);
#20847=ORIENTED_EDGE('',*,*,#15128,.T.);
#20848=ORIENTED_EDGE('',*,*,#15129,.T.);
#20849=ORIENTED_EDGE('',*,*,#15128,.F.);
#20850=ORIENTED_EDGE('',*,*,#15116,.F.);
#20851=ORIENTED_EDGE('',*,*,#15130,.T.);
#20852=ORIENTED_EDGE('',*,*,#15120,.T.);
#20853=ORIENTED_EDGE('',*,*,#15130,.F.);
#20854=ORIENTED_EDGE('',*,*,#15119,.F.);
#20855=ORIENTED_EDGE('',*,*,#15115,.F.);
#20856=ORIENTED_EDGE('',*,*,#15114,.F.);
#20857=ORIENTED_EDGE('',*,*,#15108,.F.);
#20858=ORIENTED_EDGE('',*,*,#15107,.F.);
#20859=ORIENTED_EDGE('',*,*,#15131,.T.);
#20860=ORIENTED_EDGE('',*,*,#15132,.T.);
#20861=ORIENTED_EDGE('',*,*,#15133,.T.);
#20862=ORIENTED_EDGE('',*,*,#15134,.T.);
#20863=ORIENTED_EDGE('',*,*,#15135,.T.);
#20864=ORIENTED_EDGE('',*,*,#15136,.T.);
#20865=ORIENTED_EDGE('',*,*,#15137,.T.);
#20866=ORIENTED_EDGE('',*,*,#15138,.T.);
#20867=ORIENTED_EDGE('',*,*,#15139,.F.);
#20868=ORIENTED_EDGE('',*,*,#15140,.T.);
#20869=ORIENTED_EDGE('',*,*,#15102,.F.);
#20870=ORIENTED_EDGE('',*,*,#15105,.F.);
#20871=ORIENTED_EDGE('',*,*,#15141,.T.);
#20872=ORIENTED_EDGE('',*,*,#15142,.T.);
#20873=ORIENTED_EDGE('',*,*,#15143,.F.);
#20874=ORIENTED_EDGE('',*,*,#15144,.T.);
#20875=ORIENTED_EDGE('',*,*,#15145,.T.);
#20876=ORIENTED_EDGE('',*,*,#15146,.T.);
#20877=ORIENTED_EDGE('',*,*,#15147,.F.);
#20878=ORIENTED_EDGE('',*,*,#15148,.T.);
#20879=ORIENTED_EDGE('',*,*,#15127,.T.);
#20880=ORIENTED_EDGE('',*,*,#15122,.F.);
#20881=ORIENTED_EDGE('',*,*,#15143,.T.);
#20882=ORIENTED_EDGE('',*,*,#15149,.T.);
#20883=ORIENTED_EDGE('',*,*,#15125,.T.);
#20884=ORIENTED_EDGE('',*,*,#15150,.T.);
#20885=ORIENTED_EDGE('',*,*,#15139,.T.);
#20886=ORIENTED_EDGE('',*,*,#15151,.T.);
#20887=ORIENTED_EDGE('',*,*,#15147,.T.);
#20888=ORIENTED_EDGE('',*,*,#15152,.T.);
#20889=ORIENTED_EDGE('',*,*,#15129,.F.);
#20890=ORIENTED_EDGE('',*,*,#15123,.F.);
#20891=ORIENTED_EDGE('',*,*,#15153,.T.);
#20892=ORIENTED_EDGE('',*,*,#15141,.F.);
#20893=ORIENTED_EDGE('',*,*,#15154,.T.);
#20894=ORIENTED_EDGE('',*,*,#15145,.F.);
#20895=ORIENTED_EDGE('',*,*,#15155,.T.);
#20896=ORIENTED_EDGE('',*,*,#15137,.F.);
#20897=ORIENTED_EDGE('',*,*,#15156,.T.);
#20898=ORIENTED_EDGE('',*,*,#15118,.T.);
#20899=ORIENTED_EDGE('',*,*,#15156,.F.);
#20900=ORIENTED_EDGE('',*,*,#15140,.F.);
#20901=ORIENTED_EDGE('',*,*,#15150,.F.);
#20902=ORIENTED_EDGE('',*,*,#15124,.F.);
#20903=ORIENTED_EDGE('',*,*,#15155,.F.);
#20904=ORIENTED_EDGE('',*,*,#15148,.F.);
#20905=ORIENTED_EDGE('',*,*,#15151,.F.);
#20906=ORIENTED_EDGE('',*,*,#15138,.F.);
#20907=ORIENTED_EDGE('',*,*,#15154,.F.);
#20908=ORIENTED_EDGE('',*,*,#15144,.F.);
#20909=ORIENTED_EDGE('',*,*,#15152,.F.);
#20910=ORIENTED_EDGE('',*,*,#15146,.F.);
#20911=ORIENTED_EDGE('',*,*,#15153,.F.);
#20912=ORIENTED_EDGE('',*,*,#15126,.F.);
#20913=ORIENTED_EDGE('',*,*,#15149,.F.);
#20914=ORIENTED_EDGE('',*,*,#15142,.F.);
#20915=ORIENTED_EDGE('',*,*,#15111,.T.);
#20916=ORIENTED_EDGE('',*,*,#15157,.F.);
#20917=ORIENTED_EDGE('',*,*,#15158,.F.);
#20918=ORIENTED_EDGE('',*,*,#15159,.F.);
#20919=ORIENTED_EDGE('',*,*,#15160,.T.);
#20920=ORIENTED_EDGE('',*,*,#15132,.F.);
#20921=ORIENTED_EDGE('',*,*,#15160,.F.);
#20922=ORIENTED_EDGE('',*,*,#15161,.F.);
#20923=ORIENTED_EDGE('',*,*,#15162,.F.);
#20924=ORIENTED_EDGE('',*,*,#15163,.T.);
#20925=ORIENTED_EDGE('',*,*,#15133,.F.);
#20926=ORIENTED_EDGE('',*,*,#15163,.F.);
#20927=ORIENTED_EDGE('',*,*,#15164,.F.);
#20928=ORIENTED_EDGE('',*,*,#15165,.F.);
#20929=ORIENTED_EDGE('',*,*,#15166,.T.);
#20930=ORIENTED_EDGE('',*,*,#15134,.F.);
#20931=ORIENTED_EDGE('',*,*,#15166,.F.);
#20932=ORIENTED_EDGE('',*,*,#15167,.F.);
#20933=ORIENTED_EDGE('',*,*,#15168,.F.);
#20934=ORIENTED_EDGE('',*,*,#15169,.T.);
#20935=ORIENTED_EDGE('',*,*,#15135,.F.);
#20936=ORIENTED_EDGE('',*,*,#15169,.F.);
#20937=ORIENTED_EDGE('',*,*,#15170,.F.);
#20938=ORIENTED_EDGE('',*,*,#15171,.F.);
#20939=ORIENTED_EDGE('',*,*,#15172,.T.);
#20940=ORIENTED_EDGE('',*,*,#15136,.F.);
#20941=ORIENTED_EDGE('',*,*,#15172,.F.);
#20942=ORIENTED_EDGE('',*,*,#15173,.F.);
#20943=ORIENTED_EDGE('',*,*,#15174,.F.);
#20944=ORIENTED_EDGE('',*,*,#15157,.T.);
#20945=ORIENTED_EDGE('',*,*,#15131,.F.);
#20946=ORIENTED_EDGE('',*,*,#15158,.T.);
#20947=ORIENTED_EDGE('',*,*,#15174,.T.);
#20948=ORIENTED_EDGE('',*,*,#15101,.T.);
#20949=ORIENTED_EDGE('',*,*,#15173,.T.);
#20950=ORIENTED_EDGE('',*,*,#15171,.T.);
#20951=ORIENTED_EDGE('',*,*,#15096,.T.);
#20952=ORIENTED_EDGE('',*,*,#15170,.T.);
#20953=ORIENTED_EDGE('',*,*,#15168,.T.);
#20954=ORIENTED_EDGE('',*,*,#15097,.T.);
#20955=ORIENTED_EDGE('',*,*,#15167,.T.);
#20956=ORIENTED_EDGE('',*,*,#15165,.T.);
#20957=ORIENTED_EDGE('',*,*,#15098,.T.);
#20958=ORIENTED_EDGE('',*,*,#15164,.T.);
#20959=ORIENTED_EDGE('',*,*,#15162,.T.);
#20960=ORIENTED_EDGE('',*,*,#15099,.T.);
#20961=ORIENTED_EDGE('',*,*,#15161,.T.);
#20962=ORIENTED_EDGE('',*,*,#15159,.T.);
#20963=ORIENTED_EDGE('',*,*,#15100,.T.);
#20964=ORIENTED_EDGE('',*,*,#15175,.F.);
#20965=ORIENTED_EDGE('',*,*,#15176,.T.);
#20966=ORIENTED_EDGE('',*,*,#15177,.T.);
#20967=ORIENTED_EDGE('',*,*,#15176,.F.);
#20968=ORIENTED_EDGE('',*,*,#15178,.F.);
#20969=ORIENTED_EDGE('',*,*,#15179,.T.);
#20970=ORIENTED_EDGE('',*,*,#15180,.T.);
#20971=ORIENTED_EDGE('',*,*,#15179,.F.);
#20972=ORIENTED_EDGE('',*,*,#15175,.T.);
#20973=ORIENTED_EDGE('',*,*,#15180,.F.);
#20974=ORIENTED_EDGE('',*,*,#15177,.F.);
#20975=ORIENTED_EDGE('',*,*,#15178,.T.);
#20976=ORIENTED_EDGE('',*,*,#15181,.F.);
#20977=ORIENTED_EDGE('',*,*,#15182,.T.);
#20978=ORIENTED_EDGE('',*,*,#15183,.T.);
#20979=ORIENTED_EDGE('',*,*,#15182,.F.);
#20980=ORIENTED_EDGE('',*,*,#15184,.F.);
#20981=ORIENTED_EDGE('',*,*,#15185,.T.);
#20982=ORIENTED_EDGE('',*,*,#15186,.T.);
#20983=ORIENTED_EDGE('',*,*,#15185,.F.);
#20984=ORIENTED_EDGE('',*,*,#15187,.F.);
#20985=ORIENTED_EDGE('',*,*,#15188,.T.);
#20986=ORIENTED_EDGE('',*,*,#15189,.T.);
#20987=ORIENTED_EDGE('',*,*,#15188,.F.);
#20988=ORIENTED_EDGE('',*,*,#15190,.F.);
#20989=ORIENTED_EDGE('',*,*,#15191,.T.);
#20990=ORIENTED_EDGE('',*,*,#15192,.T.);
#20991=ORIENTED_EDGE('',*,*,#15191,.F.);
#20992=ORIENTED_EDGE('',*,*,#15193,.F.);
#20993=ORIENTED_EDGE('',*,*,#15194,.T.);
#20994=ORIENTED_EDGE('',*,*,#15195,.T.);
#20995=ORIENTED_EDGE('',*,*,#15194,.F.);
#20996=ORIENTED_EDGE('',*,*,#15196,.F.);
#20997=ORIENTED_EDGE('',*,*,#15197,.T.);
#20998=ORIENTED_EDGE('',*,*,#15198,.T.);
#20999=ORIENTED_EDGE('',*,*,#15197,.F.);
#21000=ORIENTED_EDGE('',*,*,#15199,.F.);
#21001=ORIENTED_EDGE('',*,*,#15200,.F.);
#21002=ORIENTED_EDGE('',*,*,#15201,.T.);
#21003=ORIENTED_EDGE('',*,*,#15202,.T.);
#21004=ORIENTED_EDGE('',*,*,#15201,.F.);
#21005=ORIENTED_EDGE('',*,*,#15203,.F.);
#21006=ORIENTED_EDGE('',*,*,#15204,.F.);
#21007=ORIENTED_EDGE('',*,*,#15205,.T.);
#21008=ORIENTED_EDGE('',*,*,#15206,.T.);
#21009=ORIENTED_EDGE('',*,*,#15207,.F.);
#21010=ORIENTED_EDGE('',*,*,#15208,.F.);
#21011=ORIENTED_EDGE('',*,*,#15209,.T.);
#21012=ORIENTED_EDGE('',*,*,#15202,.F.);
#21013=ORIENTED_EDGE('',*,*,#15207,.T.);
#21014=ORIENTED_EDGE('',*,*,#15210,.T.);
#21015=ORIENTED_EDGE('',*,*,#15211,.F.);
#21016=ORIENTED_EDGE('',*,*,#15212,.F.);
#21017=ORIENTED_EDGE('',*,*,#15213,.F.);
#21018=ORIENTED_EDGE('',*,*,#15214,.F.);
#21019=ORIENTED_EDGE('',*,*,#15211,.T.);
#21020=ORIENTED_EDGE('',*,*,#15215,.T.);
#21021=ORIENTED_EDGE('',*,*,#15216,.F.);
#21022=ORIENTED_EDGE('',*,*,#15217,.F.);
#21023=ORIENTED_EDGE('',*,*,#15218,.T.);
#21024=ORIENTED_EDGE('',*,*,#15219,.F.);
#21025=ORIENTED_EDGE('',*,*,#15216,.T.);
#21026=ORIENTED_EDGE('',*,*,#15220,.T.);
#21027=ORIENTED_EDGE('',*,*,#15205,.F.);
#21028=ORIENTED_EDGE('',*,*,#15221,.F.);
#21029=ORIENTED_EDGE('',*,*,#15222,.F.);
#21030=ORIENTED_EDGE('',*,*,#15212,.T.);
#21031=ORIENTED_EDGE('',*,*,#15219,.T.);
#21032=ORIENTED_EDGE('',*,*,#15206,.F.);
#21033=ORIENTED_EDGE('',*,*,#15220,.F.);
#21034=ORIENTED_EDGE('',*,*,#15215,.F.);
#21035=ORIENTED_EDGE('',*,*,#15210,.F.);
#21036=ORIENTED_EDGE('',*,*,#15181,.T.);
#21037=ORIENTED_EDGE('',*,*,#15184,.T.);
#21038=ORIENTED_EDGE('',*,*,#15187,.T.);
#21039=ORIENTED_EDGE('',*,*,#15190,.T.);
#21040=ORIENTED_EDGE('',*,*,#15193,.T.);
#21041=ORIENTED_EDGE('',*,*,#15196,.T.);
#21042=ORIENTED_EDGE('',*,*,#15199,.T.);
#21043=ORIENTED_EDGE('',*,*,#15209,.F.);
#21044=ORIENTED_EDGE('',*,*,#15223,.F.);
#21045=ORIENTED_EDGE('',*,*,#15224,.T.);
#21046=ORIENTED_EDGE('',*,*,#15200,.T.);
#21047=ORIENTED_EDGE('',*,*,#15224,.F.);
#21048=ORIENTED_EDGE('',*,*,#15225,.F.);
#21049=ORIENTED_EDGE('',*,*,#15203,.T.);
#21050=ORIENTED_EDGE('',*,*,#15221,.T.);
#21051=ORIENTED_EDGE('',*,*,#15218,.F.);
#21052=ORIENTED_EDGE('',*,*,#15226,.F.);
#21053=ORIENTED_EDGE('',*,*,#15227,.T.);
#21054=ORIENTED_EDGE('',*,*,#15222,.T.);
#21055=ORIENTED_EDGE('',*,*,#15227,.F.);
#21056=ORIENTED_EDGE('',*,*,#15228,.F.);
#21057=ORIENTED_EDGE('',*,*,#15213,.T.);
#21058=ORIENTED_EDGE('',*,*,#15214,.T.);
#21059=ORIENTED_EDGE('',*,*,#15228,.T.);
#21060=ORIENTED_EDGE('',*,*,#15226,.T.);
#21061=ORIENTED_EDGE('',*,*,#15217,.T.);
#21062=ORIENTED_EDGE('',*,*,#15204,.T.);
#21063=ORIENTED_EDGE('',*,*,#15225,.T.);
#21064=ORIENTED_EDGE('',*,*,#15223,.T.);
#21065=ORIENTED_EDGE('',*,*,#15208,.T.);
#21066=ORIENTED_EDGE('',*,*,#15183,.F.);
#21067=ORIENTED_EDGE('',*,*,#15186,.F.);
#21068=ORIENTED_EDGE('',*,*,#15189,.F.);
#21069=ORIENTED_EDGE('',*,*,#15192,.F.);
#21070=ORIENTED_EDGE('',*,*,#15195,.F.);
#21071=ORIENTED_EDGE('',*,*,#15198,.F.);
#21072=ORIENTED_EDGE('',*,*,#15229,.F.);
#21073=ORIENTED_EDGE('',*,*,#15229,.T.);
#21074=ORIENTED_EDGE('',*,*,#15230,.T.);
#21075=ORIENTED_EDGE('',*,*,#15231,.F.);
#21076=ORIENTED_EDGE('',*,*,#15230,.F.);
#21077=ORIENTED_EDGE('',*,*,#15232,.T.);
#21078=ORIENTED_EDGE('',*,*,#15233,.T.);
#21079=ORIENTED_EDGE('',*,*,#15234,.T.);
#21080=ORIENTED_EDGE('',*,*,#15232,.F.);
#21081=ORIENTED_EDGE('',*,*,#15234,.F.);
#21082=ORIENTED_EDGE('',*,*,#15235,.T.);
#21083=ORIENTED_EDGE('',*,*,#15236,.F.);
#21084=ORIENTED_EDGE('',*,*,#15237,.F.);
#21085=ORIENTED_EDGE('',*,*,#15238,.T.);
#21086=ORIENTED_EDGE('',*,*,#15239,.F.);
#21087=ORIENTED_EDGE('',*,*,#15240,.T.);
#21088=ORIENTED_EDGE('',*,*,#15241,.T.);
#21089=ORIENTED_EDGE('',*,*,#15238,.F.);
#21090=ORIENTED_EDGE('',*,*,#15242,.T.);
#21091=ORIENTED_EDGE('',*,*,#15243,.T.);
#21092=ORIENTED_EDGE('',*,*,#15244,.T.);
#21093=ORIENTED_EDGE('',*,*,#15245,.F.);
#21094=ORIENTED_EDGE('',*,*,#15240,.F.);
#21095=ORIENTED_EDGE('',*,*,#15244,.F.);
#21096=ORIENTED_EDGE('',*,*,#15246,.F.);
#21097=ORIENTED_EDGE('',*,*,#15246,.T.);
#21098=ORIENTED_EDGE('',*,*,#15247,.F.);
#21099=ORIENTED_EDGE('',*,*,#15248,.T.);
#21100=ORIENTED_EDGE('',*,*,#15249,.T.);
#21101=ORIENTED_EDGE('',*,*,#15241,.F.);
#21102=ORIENTED_EDGE('',*,*,#15249,.F.);
#21103=ORIENTED_EDGE('',*,*,#15250,.T.);
#21104=ORIENTED_EDGE('',*,*,#15251,.F.);
#21105=ORIENTED_EDGE('',*,*,#15252,.T.);
#21106=ORIENTED_EDGE('',*,*,#15253,.F.);
#21107=ORIENTED_EDGE('',*,*,#15235,.F.);
#21108=ORIENTED_EDGE('',*,*,#15251,.T.);
#21109=ORIENTED_EDGE('',*,*,#15254,.T.);
#21110=ORIENTED_EDGE('',*,*,#15255,.F.);
#21111=ORIENTED_EDGE('',*,*,#15252,.F.);
#21112=ORIENTED_EDGE('',*,*,#15256,.T.);
#21113=ORIENTED_EDGE('',*,*,#15250,.F.);
#21114=ORIENTED_EDGE('',*,*,#15257,.T.);
#21115=ORIENTED_EDGE('',*,*,#15258,.T.);
#21116=ORIENTED_EDGE('',*,*,#15256,.F.);
#21117=ORIENTED_EDGE('',*,*,#15248,.F.);
#21118=ORIENTED_EDGE('',*,*,#15259,.F.);
#21119=ORIENTED_EDGE('',*,*,#15257,.F.);
#21120=ORIENTED_EDGE('',*,*,#15260,.T.);
#21121=ORIENTED_EDGE('',*,*,#15261,.F.);
#21122=ORIENTED_EDGE('',*,*,#15262,.F.);
#21123=ORIENTED_EDGE('',*,*,#15263,.T.);
#21124=ORIENTED_EDGE('',*,*,#15264,.T.);
#21125=ORIENTED_EDGE('',*,*,#15265,.T.);
#21126=ORIENTED_EDGE('',*,*,#15266,.F.);
#21127=ORIENTED_EDGE('',*,*,#15263,.F.);
#21128=ORIENTED_EDGE('',*,*,#15267,.F.);
#21129=ORIENTED_EDGE('',*,*,#15265,.F.);
#21130=ORIENTED_EDGE('',*,*,#15268,.F.);
#21131=ORIENTED_EDGE('',*,*,#15259,.T.);
#21132=ORIENTED_EDGE('',*,*,#15269,.F.);
#21133=ORIENTED_EDGE('',*,*,#15268,.T.);
#21134=ORIENTED_EDGE('',*,*,#15270,.T.);
#21135=ORIENTED_EDGE('',*,*,#15247,.T.);
#21136=ORIENTED_EDGE('',*,*,#15243,.F.);
#21137=ORIENTED_EDGE('',*,*,#15271,.F.);
#21138=ORIENTED_EDGE('',*,*,#15269,.T.);
#21139=ORIENTED_EDGE('',*,*,#15272,.T.);
#21140=ORIENTED_EDGE('',*,*,#15273,.F.);
#21141=ORIENTED_EDGE('',*,*,#15267,.T.);
#21142=ORIENTED_EDGE('',*,*,#15271,.T.);
#21143=ORIENTED_EDGE('',*,*,#15274,.F.);
#21144=ORIENTED_EDGE('',*,*,#15272,.F.);
#21145=ORIENTED_EDGE('',*,*,#15242,.F.);
#21146=ORIENTED_EDGE('',*,*,#15275,.T.);
#21147=ORIENTED_EDGE('',*,*,#15276,.F.);
#21148=ORIENTED_EDGE('',*,*,#15277,.F.);
#21149=ORIENTED_EDGE('',*,*,#15278,.T.);
#21150=ORIENTED_EDGE('',*,*,#15279,.F.);
#21151=ORIENTED_EDGE('',*,*,#15278,.F.);
#21152=ORIENTED_EDGE('',*,*,#15280,.T.);
#21153=ORIENTED_EDGE('',*,*,#15274,.T.);
#21154=ORIENTED_EDGE('',*,*,#15266,.T.);
#21155=ORIENTED_EDGE('',*,*,#15273,.T.);
#21156=ORIENTED_EDGE('',*,*,#15280,.F.);
#21157=ORIENTED_EDGE('',*,*,#15281,.F.);
#21158=ORIENTED_EDGE('',*,*,#15277,.T.);
#21159=ORIENTED_EDGE('',*,*,#15282,.F.);
#21160=ORIENTED_EDGE('',*,*,#15260,.F.);
#21161=ORIENTED_EDGE('',*,*,#15281,.T.);
#21162=ORIENTED_EDGE('',*,*,#15283,.T.);
#21163=ORIENTED_EDGE('',*,*,#15284,.F.);
#21164=ORIENTED_EDGE('',*,*,#15285,.F.);
#21165=ORIENTED_EDGE('',*,*,#15286,.T.);
#21166=ORIENTED_EDGE('',*,*,#15287,.F.);
#21167=ORIENTED_EDGE('',*,*,#15288,.T.);
#21168=ORIENTED_EDGE('',*,*,#15289,.T.);
#21169=ORIENTED_EDGE('',*,*,#15286,.F.);
#21170=ORIENTED_EDGE('',*,*,#15290,.T.);
#21171=ORIENTED_EDGE('',*,*,#15291,.T.);
#21172=ORIENTED_EDGE('',*,*,#15292,.T.);
#21173=ORIENTED_EDGE('',*,*,#15293,.F.);
#21174=ORIENTED_EDGE('',*,*,#15288,.F.);
#21175=ORIENTED_EDGE('',*,*,#15292,.F.);
#21176=ORIENTED_EDGE('',*,*,#15294,.F.);
#21177=ORIENTED_EDGE('',*,*,#15294,.T.);
#21178=ORIENTED_EDGE('',*,*,#15295,.F.);
#21179=ORIENTED_EDGE('',*,*,#15296,.T.);
#21180=ORIENTED_EDGE('',*,*,#15297,.T.);
#21181=ORIENTED_EDGE('',*,*,#15289,.F.);
#21182=ORIENTED_EDGE('',*,*,#15297,.F.);
#21183=ORIENTED_EDGE('',*,*,#15298,.T.);
#21184=ORIENTED_EDGE('',*,*,#15299,.F.);
#21185=ORIENTED_EDGE('',*,*,#15300,.T.);
#21186=ORIENTED_EDGE('',*,*,#15301,.F.);
#21187=ORIENTED_EDGE('',*,*,#15283,.F.);
#21188=ORIENTED_EDGE('',*,*,#15299,.T.);
#21189=ORIENTED_EDGE('',*,*,#15302,.T.);
#21190=ORIENTED_EDGE('',*,*,#15303,.F.);
#21191=ORIENTED_EDGE('',*,*,#15300,.F.);
#21192=ORIENTED_EDGE('',*,*,#15304,.T.);
#21193=ORIENTED_EDGE('',*,*,#15298,.F.);
#21194=ORIENTED_EDGE('',*,*,#15305,.T.);
#21195=ORIENTED_EDGE('',*,*,#15306,.T.);
#21196=ORIENTED_EDGE('',*,*,#15304,.F.);
#21197=ORIENTED_EDGE('',*,*,#15296,.F.);
#21198=ORIENTED_EDGE('',*,*,#15307,.F.);
#21199=ORIENTED_EDGE('',*,*,#15305,.F.);
#21200=ORIENTED_EDGE('',*,*,#15308,.T.);
#21201=ORIENTED_EDGE('',*,*,#15309,.F.);
#21202=ORIENTED_EDGE('',*,*,#15310,.F.);
#21203=ORIENTED_EDGE('',*,*,#15311,.T.);
#21204=ORIENTED_EDGE('',*,*,#15312,.T.);
#21205=ORIENTED_EDGE('',*,*,#15313,.T.);
#21206=ORIENTED_EDGE('',*,*,#15314,.F.);
#21207=ORIENTED_EDGE('',*,*,#15311,.F.);
#21208=ORIENTED_EDGE('',*,*,#15315,.F.);
#21209=ORIENTED_EDGE('',*,*,#15313,.F.);
#21210=ORIENTED_EDGE('',*,*,#15316,.F.);
#21211=ORIENTED_EDGE('',*,*,#15307,.T.);
#21212=ORIENTED_EDGE('',*,*,#15317,.F.);
#21213=ORIENTED_EDGE('',*,*,#15316,.T.);
#21214=ORIENTED_EDGE('',*,*,#15318,.T.);
#21215=ORIENTED_EDGE('',*,*,#15295,.T.);
#21216=ORIENTED_EDGE('',*,*,#15291,.F.);
#21217=ORIENTED_EDGE('',*,*,#15319,.F.);
#21218=ORIENTED_EDGE('',*,*,#15317,.T.);
#21219=ORIENTED_EDGE('',*,*,#15320,.T.);
#21220=ORIENTED_EDGE('',*,*,#15321,.F.);
#21221=ORIENTED_EDGE('',*,*,#15315,.T.);
#21222=ORIENTED_EDGE('',*,*,#15319,.T.);
#21223=ORIENTED_EDGE('',*,*,#15322,.F.);
#21224=ORIENTED_EDGE('',*,*,#15320,.F.);
#21225=ORIENTED_EDGE('',*,*,#15290,.F.);
#21226=ORIENTED_EDGE('',*,*,#15323,.T.);
#21227=ORIENTED_EDGE('',*,*,#15324,.F.);
#21228=ORIENTED_EDGE('',*,*,#15325,.F.);
#21229=ORIENTED_EDGE('',*,*,#15326,.T.);
#21230=ORIENTED_EDGE('',*,*,#15327,.F.);
#21231=ORIENTED_EDGE('',*,*,#15326,.F.);
#21232=ORIENTED_EDGE('',*,*,#15328,.T.);
#21233=ORIENTED_EDGE('',*,*,#15322,.T.);
#21234=ORIENTED_EDGE('',*,*,#15314,.T.);
#21235=ORIENTED_EDGE('',*,*,#15321,.T.);
#21236=ORIENTED_EDGE('',*,*,#15328,.F.);
#21237=ORIENTED_EDGE('',*,*,#15329,.F.);
#21238=ORIENTED_EDGE('',*,*,#15325,.T.);
#21239=ORIENTED_EDGE('',*,*,#15330,.F.);
#21240=ORIENTED_EDGE('',*,*,#15308,.F.);
#21241=ORIENTED_EDGE('',*,*,#15329,.T.);
#21242=ORIENTED_EDGE('',*,*,#15331,.T.);
#21243=ORIENTED_EDGE('',*,*,#15332,.F.);
#21244=ORIENTED_EDGE('',*,*,#15333,.F.);
#21245=ORIENTED_EDGE('',*,*,#15334,.T.);
#21246=ORIENTED_EDGE('',*,*,#15335,.F.);
#21247=ORIENTED_EDGE('',*,*,#15336,.T.);
#21248=ORIENTED_EDGE('',*,*,#15337,.T.);
#21249=ORIENTED_EDGE('',*,*,#15334,.F.);
#21250=ORIENTED_EDGE('',*,*,#15338,.T.);
#21251=ORIENTED_EDGE('',*,*,#15339,.T.);
#21252=ORIENTED_EDGE('',*,*,#15340,.T.);
#21253=ORIENTED_EDGE('',*,*,#15341,.F.);
#21254=ORIENTED_EDGE('',*,*,#15336,.F.);
#21255=ORIENTED_EDGE('',*,*,#15340,.F.);
#21256=ORIENTED_EDGE('',*,*,#15342,.F.);
#21257=ORIENTED_EDGE('',*,*,#15342,.T.);
#21258=ORIENTED_EDGE('',*,*,#15343,.F.);
#21259=ORIENTED_EDGE('',*,*,#15344,.T.);
#21260=ORIENTED_EDGE('',*,*,#15345,.T.);
#21261=ORIENTED_EDGE('',*,*,#15337,.F.);
#21262=ORIENTED_EDGE('',*,*,#15345,.F.);
#21263=ORIENTED_EDGE('',*,*,#15346,.T.);
#21264=ORIENTED_EDGE('',*,*,#15347,.F.);
#21265=ORIENTED_EDGE('',*,*,#15348,.T.);
#21266=ORIENTED_EDGE('',*,*,#15349,.F.);
#21267=ORIENTED_EDGE('',*,*,#15331,.F.);
#21268=ORIENTED_EDGE('',*,*,#15347,.T.);
#21269=ORIENTED_EDGE('',*,*,#15350,.T.);
#21270=ORIENTED_EDGE('',*,*,#15351,.F.);
#21271=ORIENTED_EDGE('',*,*,#15348,.F.);
#21272=ORIENTED_EDGE('',*,*,#15352,.T.);
#21273=ORIENTED_EDGE('',*,*,#15346,.F.);
#21274=ORIENTED_EDGE('',*,*,#15353,.T.);
#21275=ORIENTED_EDGE('',*,*,#15354,.T.);
#21276=ORIENTED_EDGE('',*,*,#15352,.F.);
#21277=ORIENTED_EDGE('',*,*,#15344,.F.);
#21278=ORIENTED_EDGE('',*,*,#15355,.F.);
#21279=ORIENTED_EDGE('',*,*,#15353,.F.);
#21280=ORIENTED_EDGE('',*,*,#15356,.T.);
#21281=ORIENTED_EDGE('',*,*,#15357,.F.);
#21282=ORIENTED_EDGE('',*,*,#15358,.F.);
#21283=ORIENTED_EDGE('',*,*,#15359,.T.);
#21284=ORIENTED_EDGE('',*,*,#15360,.T.);
#21285=ORIENTED_EDGE('',*,*,#15361,.T.);
#21286=ORIENTED_EDGE('',*,*,#15362,.F.);
#21287=ORIENTED_EDGE('',*,*,#15359,.F.);
#21288=ORIENTED_EDGE('',*,*,#15363,.F.);
#21289=ORIENTED_EDGE('',*,*,#15361,.F.);
#21290=ORIENTED_EDGE('',*,*,#15364,.F.);
#21291=ORIENTED_EDGE('',*,*,#15355,.T.);
#21292=ORIENTED_EDGE('',*,*,#15365,.F.);
#21293=ORIENTED_EDGE('',*,*,#15364,.T.);
#21294=ORIENTED_EDGE('',*,*,#15366,.T.);
#21295=ORIENTED_EDGE('',*,*,#15343,.T.);
#21296=ORIENTED_EDGE('',*,*,#15339,.F.);
#21297=ORIENTED_EDGE('',*,*,#15367,.F.);
#21298=ORIENTED_EDGE('',*,*,#15365,.T.);
#21299=ORIENTED_EDGE('',*,*,#15368,.T.);
#21300=ORIENTED_EDGE('',*,*,#15369,.F.);
#21301=ORIENTED_EDGE('',*,*,#15363,.T.);
#21302=ORIENTED_EDGE('',*,*,#15367,.T.);
#21303=ORIENTED_EDGE('',*,*,#15370,.F.);
#21304=ORIENTED_EDGE('',*,*,#15368,.F.);
#21305=ORIENTED_EDGE('',*,*,#15338,.F.);
#21306=ORIENTED_EDGE('',*,*,#15371,.T.);
#21307=ORIENTED_EDGE('',*,*,#15372,.F.);
#21308=ORIENTED_EDGE('',*,*,#15373,.F.);
#21309=ORIENTED_EDGE('',*,*,#15374,.T.);
#21310=ORIENTED_EDGE('',*,*,#15375,.F.);
#21311=ORIENTED_EDGE('',*,*,#15374,.F.);
#21312=ORIENTED_EDGE('',*,*,#15376,.T.);
#21313=ORIENTED_EDGE('',*,*,#15370,.T.);
#21314=ORIENTED_EDGE('',*,*,#15362,.T.);
#21315=ORIENTED_EDGE('',*,*,#15369,.T.);
#21316=ORIENTED_EDGE('',*,*,#15376,.F.);
#21317=ORIENTED_EDGE('',*,*,#15377,.F.);
#21318=ORIENTED_EDGE('',*,*,#15373,.T.);
#21319=ORIENTED_EDGE('',*,*,#15378,.F.);
#21320=ORIENTED_EDGE('',*,*,#15356,.F.);
#21321=ORIENTED_EDGE('',*,*,#15377,.T.);
#21322=ORIENTED_EDGE('',*,*,#15379,.T.);
#21323=ORIENTED_EDGE('',*,*,#15380,.F.);
#21324=ORIENTED_EDGE('',*,*,#15381,.F.);
#21325=ORIENTED_EDGE('',*,*,#15382,.T.);
#21326=ORIENTED_EDGE('',*,*,#15383,.F.);
#21327=ORIENTED_EDGE('',*,*,#15384,.T.);
#21328=ORIENTED_EDGE('',*,*,#15385,.T.);
#21329=ORIENTED_EDGE('',*,*,#15382,.F.);
#21330=ORIENTED_EDGE('',*,*,#15386,.T.);
#21331=ORIENTED_EDGE('',*,*,#15387,.T.);
#21332=ORIENTED_EDGE('',*,*,#15388,.T.);
#21333=ORIENTED_EDGE('',*,*,#15389,.F.);
#21334=ORIENTED_EDGE('',*,*,#15384,.F.);
#21335=ORIENTED_EDGE('',*,*,#15388,.F.);
#21336=ORIENTED_EDGE('',*,*,#15390,.F.);
#21337=ORIENTED_EDGE('',*,*,#15390,.T.);
#21338=ORIENTED_EDGE('',*,*,#15391,.F.);
#21339=ORIENTED_EDGE('',*,*,#15392,.T.);
#21340=ORIENTED_EDGE('',*,*,#15393,.T.);
#21341=ORIENTED_EDGE('',*,*,#15385,.F.);
#21342=ORIENTED_EDGE('',*,*,#15393,.F.);
#21343=ORIENTED_EDGE('',*,*,#15394,.T.);
#21344=ORIENTED_EDGE('',*,*,#15395,.F.);
#21345=ORIENTED_EDGE('',*,*,#15396,.T.);
#21346=ORIENTED_EDGE('',*,*,#15397,.F.);
#21347=ORIENTED_EDGE('',*,*,#15379,.F.);
#21348=ORIENTED_EDGE('',*,*,#15395,.T.);
#21349=ORIENTED_EDGE('',*,*,#15398,.T.);
#21350=ORIENTED_EDGE('',*,*,#15399,.F.);
#21351=ORIENTED_EDGE('',*,*,#15396,.F.);
#21352=ORIENTED_EDGE('',*,*,#15400,.T.);
#21353=ORIENTED_EDGE('',*,*,#15394,.F.);
#21354=ORIENTED_EDGE('',*,*,#15401,.T.);
#21355=ORIENTED_EDGE('',*,*,#15402,.T.);
#21356=ORIENTED_EDGE('',*,*,#15400,.F.);
#21357=ORIENTED_EDGE('',*,*,#15392,.F.);
#21358=ORIENTED_EDGE('',*,*,#15403,.F.);
#21359=ORIENTED_EDGE('',*,*,#15401,.F.);
#21360=ORIENTED_EDGE('',*,*,#15404,.T.);
#21361=ORIENTED_EDGE('',*,*,#15405,.F.);
#21362=ORIENTED_EDGE('',*,*,#15406,.F.);
#21363=ORIENTED_EDGE('',*,*,#15407,.T.);
#21364=ORIENTED_EDGE('',*,*,#15408,.T.);
#21365=ORIENTED_EDGE('',*,*,#15409,.T.);
#21366=ORIENTED_EDGE('',*,*,#15410,.F.);
#21367=ORIENTED_EDGE('',*,*,#15407,.F.);
#21368=ORIENTED_EDGE('',*,*,#15411,.F.);
#21369=ORIENTED_EDGE('',*,*,#15409,.F.);
#21370=ORIENTED_EDGE('',*,*,#15412,.F.);
#21371=ORIENTED_EDGE('',*,*,#15403,.T.);
#21372=ORIENTED_EDGE('',*,*,#15413,.F.);
#21373=ORIENTED_EDGE('',*,*,#15412,.T.);
#21374=ORIENTED_EDGE('',*,*,#15414,.T.);
#21375=ORIENTED_EDGE('',*,*,#15391,.T.);
#21376=ORIENTED_EDGE('',*,*,#15387,.F.);
#21377=ORIENTED_EDGE('',*,*,#15415,.F.);
#21378=ORIENTED_EDGE('',*,*,#15413,.T.);
#21379=ORIENTED_EDGE('',*,*,#15416,.T.);
#21380=ORIENTED_EDGE('',*,*,#15417,.F.);
#21381=ORIENTED_EDGE('',*,*,#15411,.T.);
#21382=ORIENTED_EDGE('',*,*,#15415,.T.);
#21383=ORIENTED_EDGE('',*,*,#15418,.F.);
#21384=ORIENTED_EDGE('',*,*,#15416,.F.);
#21385=ORIENTED_EDGE('',*,*,#15386,.F.);
#21386=ORIENTED_EDGE('',*,*,#15419,.T.);
#21387=ORIENTED_EDGE('',*,*,#15420,.F.);
#21388=ORIENTED_EDGE('',*,*,#15421,.F.);
#21389=ORIENTED_EDGE('',*,*,#15422,.T.);
#21390=ORIENTED_EDGE('',*,*,#15423,.F.);
#21391=ORIENTED_EDGE('',*,*,#15422,.F.);
#21392=ORIENTED_EDGE('',*,*,#15424,.T.);
#21393=ORIENTED_EDGE('',*,*,#15418,.T.);
#21394=ORIENTED_EDGE('',*,*,#15410,.T.);
#21395=ORIENTED_EDGE('',*,*,#15417,.T.);
#21396=ORIENTED_EDGE('',*,*,#15424,.F.);
#21397=ORIENTED_EDGE('',*,*,#15425,.F.);
#21398=ORIENTED_EDGE('',*,*,#15421,.T.);
#21399=ORIENTED_EDGE('',*,*,#15426,.F.);
#21400=ORIENTED_EDGE('',*,*,#15404,.F.);
#21401=ORIENTED_EDGE('',*,*,#15425,.T.);
#21402=ORIENTED_EDGE('',*,*,#15427,.T.);
#21403=ORIENTED_EDGE('',*,*,#15428,.F.);
#21404=ORIENTED_EDGE('',*,*,#15429,.F.);
#21405=ORIENTED_EDGE('',*,*,#15430,.T.);
#21406=ORIENTED_EDGE('',*,*,#15431,.F.);
#21407=ORIENTED_EDGE('',*,*,#15432,.T.);
#21408=ORIENTED_EDGE('',*,*,#15433,.T.);
#21409=ORIENTED_EDGE('',*,*,#15430,.F.);
#21410=ORIENTED_EDGE('',*,*,#15434,.T.);
#21411=ORIENTED_EDGE('',*,*,#15435,.T.);
#21412=ORIENTED_EDGE('',*,*,#15436,.T.);
#21413=ORIENTED_EDGE('',*,*,#15437,.F.);
#21414=ORIENTED_EDGE('',*,*,#15432,.F.);
#21415=ORIENTED_EDGE('',*,*,#15436,.F.);
#21416=ORIENTED_EDGE('',*,*,#15438,.F.);
#21417=ORIENTED_EDGE('',*,*,#15438,.T.);
#21418=ORIENTED_EDGE('',*,*,#15439,.F.);
#21419=ORIENTED_EDGE('',*,*,#15440,.T.);
#21420=ORIENTED_EDGE('',*,*,#15441,.T.);
#21421=ORIENTED_EDGE('',*,*,#15433,.F.);
#21422=ORIENTED_EDGE('',*,*,#15441,.F.);
#21423=ORIENTED_EDGE('',*,*,#15442,.T.);
#21424=ORIENTED_EDGE('',*,*,#15443,.F.);
#21425=ORIENTED_EDGE('',*,*,#15444,.T.);
#21426=ORIENTED_EDGE('',*,*,#15445,.F.);
#21427=ORIENTED_EDGE('',*,*,#15427,.F.);
#21428=ORIENTED_EDGE('',*,*,#15443,.T.);
#21429=ORIENTED_EDGE('',*,*,#15446,.T.);
#21430=ORIENTED_EDGE('',*,*,#15447,.F.);
#21431=ORIENTED_EDGE('',*,*,#15444,.F.);
#21432=ORIENTED_EDGE('',*,*,#15448,.T.);
#21433=ORIENTED_EDGE('',*,*,#15442,.F.);
#21434=ORIENTED_EDGE('',*,*,#15449,.T.);
#21435=ORIENTED_EDGE('',*,*,#15450,.T.);
#21436=ORIENTED_EDGE('',*,*,#15448,.F.);
#21437=ORIENTED_EDGE('',*,*,#15440,.F.);
#21438=ORIENTED_EDGE('',*,*,#15451,.F.);
#21439=ORIENTED_EDGE('',*,*,#15449,.F.);
#21440=ORIENTED_EDGE('',*,*,#15452,.T.);
#21441=ORIENTED_EDGE('',*,*,#15453,.F.);
#21442=ORIENTED_EDGE('',*,*,#15454,.F.);
#21443=ORIENTED_EDGE('',*,*,#15455,.T.);
#21444=ORIENTED_EDGE('',*,*,#15456,.T.);
#21445=ORIENTED_EDGE('',*,*,#15457,.T.);
#21446=ORIENTED_EDGE('',*,*,#15458,.F.);
#21447=ORIENTED_EDGE('',*,*,#15455,.F.);
#21448=ORIENTED_EDGE('',*,*,#15459,.F.);
#21449=ORIENTED_EDGE('',*,*,#15457,.F.);
#21450=ORIENTED_EDGE('',*,*,#15460,.F.);
#21451=ORIENTED_EDGE('',*,*,#15451,.T.);
#21452=ORIENTED_EDGE('',*,*,#15461,.F.);
#21453=ORIENTED_EDGE('',*,*,#15460,.T.);
#21454=ORIENTED_EDGE('',*,*,#15462,.T.);
#21455=ORIENTED_EDGE('',*,*,#15439,.T.);
#21456=ORIENTED_EDGE('',*,*,#15435,.F.);
#21457=ORIENTED_EDGE('',*,*,#15463,.F.);
#21458=ORIENTED_EDGE('',*,*,#15461,.T.);
#21459=ORIENTED_EDGE('',*,*,#15464,.T.);
#21460=ORIENTED_EDGE('',*,*,#15465,.F.);
#21461=ORIENTED_EDGE('',*,*,#15459,.T.);
#21462=ORIENTED_EDGE('',*,*,#15463,.T.);
#21463=ORIENTED_EDGE('',*,*,#15466,.F.);
#21464=ORIENTED_EDGE('',*,*,#15464,.F.);
#21465=ORIENTED_EDGE('',*,*,#15434,.F.);
#21466=ORIENTED_EDGE('',*,*,#15467,.T.);
#21467=ORIENTED_EDGE('',*,*,#15468,.F.);
#21468=ORIENTED_EDGE('',*,*,#15469,.F.);
#21469=ORIENTED_EDGE('',*,*,#15470,.T.);
#21470=ORIENTED_EDGE('',*,*,#15471,.F.);
#21471=ORIENTED_EDGE('',*,*,#15470,.F.);
#21472=ORIENTED_EDGE('',*,*,#15472,.T.);
#21473=ORIENTED_EDGE('',*,*,#15466,.T.);
#21474=ORIENTED_EDGE('',*,*,#15458,.T.);
#21475=ORIENTED_EDGE('',*,*,#15465,.T.);
#21476=ORIENTED_EDGE('',*,*,#15472,.F.);
#21477=ORIENTED_EDGE('',*,*,#15473,.F.);
#21478=ORIENTED_EDGE('',*,*,#15469,.T.);
#21479=ORIENTED_EDGE('',*,*,#15474,.F.);
#21480=ORIENTED_EDGE('',*,*,#15452,.F.);
#21481=ORIENTED_EDGE('',*,*,#15473,.T.);
#21482=ORIENTED_EDGE('',*,*,#15475,.T.);
#21483=ORIENTED_EDGE('',*,*,#15476,.F.);
#21484=ORIENTED_EDGE('',*,*,#15477,.F.);
#21485=ORIENTED_EDGE('',*,*,#15478,.T.);
#21486=ORIENTED_EDGE('',*,*,#15479,.F.);
#21487=ORIENTED_EDGE('',*,*,#15480,.T.);
#21488=ORIENTED_EDGE('',*,*,#15481,.T.);
#21489=ORIENTED_EDGE('',*,*,#15478,.F.);
#21490=ORIENTED_EDGE('',*,*,#15482,.T.);
#21491=ORIENTED_EDGE('',*,*,#15483,.T.);
#21492=ORIENTED_EDGE('',*,*,#15484,.T.);
#21493=ORIENTED_EDGE('',*,*,#15485,.F.);
#21494=ORIENTED_EDGE('',*,*,#15480,.F.);
#21495=ORIENTED_EDGE('',*,*,#15484,.F.);
#21496=ORIENTED_EDGE('',*,*,#15486,.F.);
#21497=ORIENTED_EDGE('',*,*,#15486,.T.);
#21498=ORIENTED_EDGE('',*,*,#15487,.F.);
#21499=ORIENTED_EDGE('',*,*,#15488,.T.);
#21500=ORIENTED_EDGE('',*,*,#15489,.T.);
#21501=ORIENTED_EDGE('',*,*,#15481,.F.);
#21502=ORIENTED_EDGE('',*,*,#15489,.F.);
#21503=ORIENTED_EDGE('',*,*,#15490,.T.);
#21504=ORIENTED_EDGE('',*,*,#15491,.F.);
#21505=ORIENTED_EDGE('',*,*,#15492,.T.);
#21506=ORIENTED_EDGE('',*,*,#15493,.F.);
#21507=ORIENTED_EDGE('',*,*,#15475,.F.);
#21508=ORIENTED_EDGE('',*,*,#15491,.T.);
#21509=ORIENTED_EDGE('',*,*,#15494,.T.);
#21510=ORIENTED_EDGE('',*,*,#15495,.F.);
#21511=ORIENTED_EDGE('',*,*,#15492,.F.);
#21512=ORIENTED_EDGE('',*,*,#15496,.T.);
#21513=ORIENTED_EDGE('',*,*,#15490,.F.);
#21514=ORIENTED_EDGE('',*,*,#15497,.T.);
#21515=ORIENTED_EDGE('',*,*,#15498,.T.);
#21516=ORIENTED_EDGE('',*,*,#15496,.F.);
#21517=ORIENTED_EDGE('',*,*,#15488,.F.);
#21518=ORIENTED_EDGE('',*,*,#15499,.F.);
#21519=ORIENTED_EDGE('',*,*,#15497,.F.);
#21520=ORIENTED_EDGE('',*,*,#15500,.T.);
#21521=ORIENTED_EDGE('',*,*,#15501,.F.);
#21522=ORIENTED_EDGE('',*,*,#15502,.F.);
#21523=ORIENTED_EDGE('',*,*,#15503,.T.);
#21524=ORIENTED_EDGE('',*,*,#15504,.T.);
#21525=ORIENTED_EDGE('',*,*,#15505,.T.);
#21526=ORIENTED_EDGE('',*,*,#15506,.F.);
#21527=ORIENTED_EDGE('',*,*,#15503,.F.);
#21528=ORIENTED_EDGE('',*,*,#15507,.F.);
#21529=ORIENTED_EDGE('',*,*,#15505,.F.);
#21530=ORIENTED_EDGE('',*,*,#15508,.F.);
#21531=ORIENTED_EDGE('',*,*,#15499,.T.);
#21532=ORIENTED_EDGE('',*,*,#15509,.F.);
#21533=ORIENTED_EDGE('',*,*,#15508,.T.);
#21534=ORIENTED_EDGE('',*,*,#15510,.T.);
#21535=ORIENTED_EDGE('',*,*,#15487,.T.);
#21536=ORIENTED_EDGE('',*,*,#15483,.F.);
#21537=ORIENTED_EDGE('',*,*,#15511,.F.);
#21538=ORIENTED_EDGE('',*,*,#15509,.T.);
#21539=ORIENTED_EDGE('',*,*,#15512,.T.);
#21540=ORIENTED_EDGE('',*,*,#15513,.F.);
#21541=ORIENTED_EDGE('',*,*,#15507,.T.);
#21542=ORIENTED_EDGE('',*,*,#15511,.T.);
#21543=ORIENTED_EDGE('',*,*,#15514,.F.);
#21544=ORIENTED_EDGE('',*,*,#15512,.F.);
#21545=ORIENTED_EDGE('',*,*,#15482,.F.);
#21546=ORIENTED_EDGE('',*,*,#15515,.T.);
#21547=ORIENTED_EDGE('',*,*,#15516,.F.);
#21548=ORIENTED_EDGE('',*,*,#15517,.F.);
#21549=ORIENTED_EDGE('',*,*,#15518,.T.);
#21550=ORIENTED_EDGE('',*,*,#15519,.F.);
#21551=ORIENTED_EDGE('',*,*,#15518,.F.);
#21552=ORIENTED_EDGE('',*,*,#15520,.T.);
#21553=ORIENTED_EDGE('',*,*,#15514,.T.);
#21554=ORIENTED_EDGE('',*,*,#15506,.T.);
#21555=ORIENTED_EDGE('',*,*,#15513,.T.);
#21556=ORIENTED_EDGE('',*,*,#15520,.F.);
#21557=ORIENTED_EDGE('',*,*,#15521,.F.);
#21558=ORIENTED_EDGE('',*,*,#15517,.T.);
#21559=ORIENTED_EDGE('',*,*,#15522,.F.);
#21560=ORIENTED_EDGE('',*,*,#15500,.F.);
#21561=ORIENTED_EDGE('',*,*,#15521,.T.);
#21562=ORIENTED_EDGE('',*,*,#15523,.F.);
#21563=ORIENTED_EDGE('',*,*,#15524,.T.);
#21564=ORIENTED_EDGE('',*,*,#15525,.T.);
#21565=ORIENTED_EDGE('',*,*,#15526,.F.);
#21566=ORIENTED_EDGE('',*,*,#15527,.T.);
#21567=ORIENTED_EDGE('',*,*,#15528,.F.);
#21568=ORIENTED_EDGE('',*,*,#15529,.F.);
#21569=ORIENTED_EDGE('',*,*,#15526,.T.);
#21570=ORIENTED_EDGE('',*,*,#15530,.T.);
#21571=ORIENTED_EDGE('',*,*,#15531,.F.);
#21572=ORIENTED_EDGE('',*,*,#15527,.F.);
#21573=ORIENTED_EDGE('',*,*,#15532,.T.);
#21574=ORIENTED_EDGE('',*,*,#15525,.F.);
#21575=ORIENTED_EDGE('',*,*,#15533,.F.);
#21576=ORIENTED_EDGE('',*,*,#15534,.T.);
#21577=ORIENTED_EDGE('',*,*,#15532,.F.);
#21578=ORIENTED_EDGE('',*,*,#15535,.T.);
#21579=ORIENTED_EDGE('',*,*,#15536,.F.);
#21580=ORIENTED_EDGE('',*,*,#15537,.T.);
#21581=ORIENTED_EDGE('',*,*,#15533,.T.);
#21582=ORIENTED_EDGE('',*,*,#15524,.F.);
#21583=ORIENTED_EDGE('',*,*,#15538,.F.);
#21584=ORIENTED_EDGE('',*,*,#15535,.F.);
#21585=ORIENTED_EDGE('',*,*,#15539,.T.);
#21586=ORIENTED_EDGE('',*,*,#15540,.T.);
#21587=ORIENTED_EDGE('',*,*,#15538,.T.);
#21588=ORIENTED_EDGE('',*,*,#15541,.F.);
#21589=ORIENTED_EDGE('',*,*,#15536,.T.);
#21590=ORIENTED_EDGE('',*,*,#15540,.F.);
#21591=ORIENTED_EDGE('',*,*,#15542,.F.);
#21592=ORIENTED_EDGE('',*,*,#15543,.T.);
#21593=ORIENTED_EDGE('',*,*,#15544,.T.);
#21594=ORIENTED_EDGE('',*,*,#15545,.F.);
#21595=ORIENTED_EDGE('',*,*,#15546,.T.);
#21596=ORIENTED_EDGE('',*,*,#15542,.T.);
#21597=ORIENTED_EDGE('',*,*,#15547,.F.);
#21598=ORIENTED_EDGE('',*,*,#15544,.F.);
#21599=ORIENTED_EDGE('',*,*,#15539,.F.);
#21600=ORIENTED_EDGE('',*,*,#15548,.T.);
#21601=ORIENTED_EDGE('',*,*,#15549,.F.);
#21602=ORIENTED_EDGE('',*,*,#15550,.F.);
#21603=ORIENTED_EDGE('',*,*,#15551,.T.);
#21604=ORIENTED_EDGE('',*,*,#15552,.F.);
#21605=ORIENTED_EDGE('',*,*,#15551,.F.);
#21606=ORIENTED_EDGE('',*,*,#15553,.T.);
#21607=ORIENTED_EDGE('',*,*,#15547,.T.);
#21608=ORIENTED_EDGE('',*,*,#15554,.T.);
#21609=ORIENTED_EDGE('',*,*,#15545,.T.);
#21610=ORIENTED_EDGE('',*,*,#15553,.F.);
#21611=ORIENTED_EDGE('',*,*,#15555,.F.);
#21612=ORIENTED_EDGE('',*,*,#15550,.T.);
#21613=ORIENTED_EDGE('',*,*,#15556,.F.);
#21614=ORIENTED_EDGE('',*,*,#15557,.F.);
#21615=ORIENTED_EDGE('',*,*,#15555,.T.);
#21616=ORIENTED_EDGE('',*,*,#15557,.T.);
#21617=ORIENTED_EDGE('',*,*,#15558,.F.);
#21618=ORIENTED_EDGE('',*,*,#15559,.F.);
#21619=ORIENTED_EDGE('',*,*,#15560,.T.);
#21620=ORIENTED_EDGE('',*,*,#15561,.T.);
#21621=ORIENTED_EDGE('',*,*,#15562,.T.);
#21622=ORIENTED_EDGE('',*,*,#15554,.F.);
#21623=ORIENTED_EDGE('',*,*,#15560,.F.);
#21624=ORIENTED_EDGE('',*,*,#15546,.F.);
#21625=ORIENTED_EDGE('',*,*,#15562,.F.);
#21626=ORIENTED_EDGE('',*,*,#15563,.F.);
#21627=ORIENTED_EDGE('',*,*,#15564,.T.);
#21628=ORIENTED_EDGE('',*,*,#15543,.F.);
#21629=ORIENTED_EDGE('',*,*,#15563,.T.);
#21630=ORIENTED_EDGE('',*,*,#15565,.T.);
#21631=ORIENTED_EDGE('',*,*,#15537,.F.);
#21632=ORIENTED_EDGE('',*,*,#15564,.F.);
#21633=ORIENTED_EDGE('',*,*,#15566,.F.);
#21634=ORIENTED_EDGE('',*,*,#15534,.F.);
#21635=ORIENTED_EDGE('',*,*,#15566,.T.);
#21636=ORIENTED_EDGE('',*,*,#15567,.T.);
#21637=ORIENTED_EDGE('',*,*,#15568,.F.);
#21638=ORIENTED_EDGE('',*,*,#15569,.T.);
#21639=ORIENTED_EDGE('',*,*,#15570,.F.);
#21640=ORIENTED_EDGE('',*,*,#15530,.F.);
#21641=ORIENTED_EDGE('',*,*,#15568,.T.);
#21642=ORIENTED_EDGE('',*,*,#15571,.T.);
#21643=ORIENTED_EDGE('',*,*,#15572,.F.);
#21644=ORIENTED_EDGE('',*,*,#15573,.F.);
#21645=ORIENTED_EDGE('',*,*,#15574,.T.);
#21646=ORIENTED_EDGE('',*,*,#15575,.F.);
#21647=ORIENTED_EDGE('',*,*,#15576,.T.);
#21648=ORIENTED_EDGE('',*,*,#15577,.T.);
#21649=ORIENTED_EDGE('',*,*,#15574,.F.);
#21650=ORIENTED_EDGE('',*,*,#15578,.T.);
#21651=ORIENTED_EDGE('',*,*,#15579,.T.);
#21652=ORIENTED_EDGE('',*,*,#15580,.T.);
#21653=ORIENTED_EDGE('',*,*,#15581,.F.);
#21654=ORIENTED_EDGE('',*,*,#15576,.F.);
#21655=ORIENTED_EDGE('',*,*,#15580,.F.);
#21656=ORIENTED_EDGE('',*,*,#15582,.F.);
#21657=ORIENTED_EDGE('',*,*,#15582,.T.);
#21658=ORIENTED_EDGE('',*,*,#15583,.F.);
#21659=ORIENTED_EDGE('',*,*,#15584,.T.);
#21660=ORIENTED_EDGE('',*,*,#15585,.T.);
#21661=ORIENTED_EDGE('',*,*,#15577,.F.);
#21662=ORIENTED_EDGE('',*,*,#15585,.F.);
#21663=ORIENTED_EDGE('',*,*,#15586,.T.);
#21664=ORIENTED_EDGE('',*,*,#15587,.F.);
#21665=ORIENTED_EDGE('',*,*,#15588,.T.);
#21666=ORIENTED_EDGE('',*,*,#15589,.F.);
#21667=ORIENTED_EDGE('',*,*,#15571,.F.);
#21668=ORIENTED_EDGE('',*,*,#15587,.T.);
#21669=ORIENTED_EDGE('',*,*,#15590,.T.);
#21670=ORIENTED_EDGE('',*,*,#15591,.F.);
#21671=ORIENTED_EDGE('',*,*,#15588,.F.);
#21672=ORIENTED_EDGE('',*,*,#15592,.T.);
#21673=ORIENTED_EDGE('',*,*,#15586,.F.);
#21674=ORIENTED_EDGE('',*,*,#15593,.T.);
#21675=ORIENTED_EDGE('',*,*,#15594,.T.);
#21676=ORIENTED_EDGE('',*,*,#15592,.F.);
#21677=ORIENTED_EDGE('',*,*,#15584,.F.);
#21678=ORIENTED_EDGE('',*,*,#15595,.F.);
#21679=ORIENTED_EDGE('',*,*,#15593,.F.);
#21680=ORIENTED_EDGE('',*,*,#15596,.T.);
#21681=ORIENTED_EDGE('',*,*,#15597,.F.);
#21682=ORIENTED_EDGE('',*,*,#15598,.F.);
#21683=ORIENTED_EDGE('',*,*,#15599,.T.);
#21684=ORIENTED_EDGE('',*,*,#15600,.T.);
#21685=ORIENTED_EDGE('',*,*,#15601,.T.);
#21686=ORIENTED_EDGE('',*,*,#15602,.F.);
#21687=ORIENTED_EDGE('',*,*,#15599,.F.);
#21688=ORIENTED_EDGE('',*,*,#15603,.F.);
#21689=ORIENTED_EDGE('',*,*,#15601,.F.);
#21690=ORIENTED_EDGE('',*,*,#15604,.F.);
#21691=ORIENTED_EDGE('',*,*,#15595,.T.);
#21692=ORIENTED_EDGE('',*,*,#15605,.F.);
#21693=ORIENTED_EDGE('',*,*,#15604,.T.);
#21694=ORIENTED_EDGE('',*,*,#15606,.T.);
#21695=ORIENTED_EDGE('',*,*,#15583,.T.);
#21696=ORIENTED_EDGE('',*,*,#15579,.F.);
#21697=ORIENTED_EDGE('',*,*,#15607,.F.);
#21698=ORIENTED_EDGE('',*,*,#15605,.T.);
#21699=ORIENTED_EDGE('',*,*,#15608,.T.);
#21700=ORIENTED_EDGE('',*,*,#15609,.F.);
#21701=ORIENTED_EDGE('',*,*,#15603,.T.);
#21702=ORIENTED_EDGE('',*,*,#15607,.T.);
#21703=ORIENTED_EDGE('',*,*,#15610,.F.);
#21704=ORIENTED_EDGE('',*,*,#15608,.F.);
#21705=ORIENTED_EDGE('',*,*,#15578,.F.);
#21706=ORIENTED_EDGE('',*,*,#15611,.T.);
#21707=ORIENTED_EDGE('',*,*,#15612,.F.);
#21708=ORIENTED_EDGE('',*,*,#15613,.F.);
#21709=ORIENTED_EDGE('',*,*,#15614,.T.);
#21710=ORIENTED_EDGE('',*,*,#15615,.F.);
#21711=ORIENTED_EDGE('',*,*,#15614,.F.);
#21712=ORIENTED_EDGE('',*,*,#15616,.T.);
#21713=ORIENTED_EDGE('',*,*,#15610,.T.);
#21714=ORIENTED_EDGE('',*,*,#15602,.T.);
#21715=ORIENTED_EDGE('',*,*,#15609,.T.);
#21716=ORIENTED_EDGE('',*,*,#15616,.F.);
#21717=ORIENTED_EDGE('',*,*,#15617,.F.);
#21718=ORIENTED_EDGE('',*,*,#15613,.T.);
#21719=ORIENTED_EDGE('',*,*,#15618,.F.);
#21720=ORIENTED_EDGE('',*,*,#15596,.F.);
#21721=ORIENTED_EDGE('',*,*,#15617,.T.);
#21722=ORIENTED_EDGE('',*,*,#15549,.T.);
#21723=ORIENTED_EDGE('',*,*,#15619,.F.);
#21724=ORIENTED_EDGE('',*,*,#15236,.T.);
#21725=ORIENTED_EDGE('',*,*,#15253,.T.);
#21726=ORIENTED_EDGE('',*,*,#15255,.T.);
#21727=ORIENTED_EDGE('',*,*,#15620,.F.);
#21728=ORIENTED_EDGE('',*,*,#15558,.T.);
#21729=ORIENTED_EDGE('',*,*,#15556,.T.);
#21730=ORIENTED_EDGE('',*,*,#15276,.T.);
#21731=ORIENTED_EDGE('',*,*,#15621,.F.);
#21732=ORIENTED_EDGE('',*,*,#15284,.T.);
#21733=ORIENTED_EDGE('',*,*,#15301,.T.);
#21734=ORIENTED_EDGE('',*,*,#15303,.T.);
#21735=ORIENTED_EDGE('',*,*,#15622,.F.);
#21736=ORIENTED_EDGE('',*,*,#15261,.T.);
#21737=ORIENTED_EDGE('',*,*,#15282,.T.);
#21738=ORIENTED_EDGE('',*,*,#15324,.T.);
#21739=ORIENTED_EDGE('',*,*,#15623,.F.);
#21740=ORIENTED_EDGE('',*,*,#15332,.T.);
#21741=ORIENTED_EDGE('',*,*,#15349,.T.);
#21742=ORIENTED_EDGE('',*,*,#15351,.T.);
#21743=ORIENTED_EDGE('',*,*,#15624,.F.);
#21744=ORIENTED_EDGE('',*,*,#15309,.T.);
#21745=ORIENTED_EDGE('',*,*,#15330,.T.);
#21746=ORIENTED_EDGE('',*,*,#15372,.T.);
#21747=ORIENTED_EDGE('',*,*,#15625,.F.);
#21748=ORIENTED_EDGE('',*,*,#15380,.T.);
#21749=ORIENTED_EDGE('',*,*,#15397,.T.);
#21750=ORIENTED_EDGE('',*,*,#15399,.T.);
#21751=ORIENTED_EDGE('',*,*,#15626,.F.);
#21752=ORIENTED_EDGE('',*,*,#15357,.T.);
#21753=ORIENTED_EDGE('',*,*,#15378,.T.);
#21754=ORIENTED_EDGE('',*,*,#15420,.T.);
#21755=ORIENTED_EDGE('',*,*,#15627,.F.);
#21756=ORIENTED_EDGE('',*,*,#15428,.T.);
#21757=ORIENTED_EDGE('',*,*,#15445,.T.);
#21758=ORIENTED_EDGE('',*,*,#15447,.T.);
#21759=ORIENTED_EDGE('',*,*,#15628,.F.);
#21760=ORIENTED_EDGE('',*,*,#15405,.T.);
#21761=ORIENTED_EDGE('',*,*,#15426,.T.);
#21762=ORIENTED_EDGE('',*,*,#15468,.T.);
#21763=ORIENTED_EDGE('',*,*,#15629,.F.);
#21764=ORIENTED_EDGE('',*,*,#15476,.T.);
#21765=ORIENTED_EDGE('',*,*,#15493,.T.);
#21766=ORIENTED_EDGE('',*,*,#15495,.T.);
#21767=ORIENTED_EDGE('',*,*,#15630,.F.);
#21768=ORIENTED_EDGE('',*,*,#15453,.T.);
#21769=ORIENTED_EDGE('',*,*,#15474,.T.);
#21770=ORIENTED_EDGE('',*,*,#15516,.T.);
#21771=ORIENTED_EDGE('',*,*,#15631,.F.);
#21772=ORIENTED_EDGE('',*,*,#15572,.T.);
#21773=ORIENTED_EDGE('',*,*,#15589,.T.);
#21774=ORIENTED_EDGE('',*,*,#15591,.T.);
#21775=ORIENTED_EDGE('',*,*,#15632,.F.);
#21776=ORIENTED_EDGE('',*,*,#15501,.T.);
#21777=ORIENTED_EDGE('',*,*,#15522,.T.);
#21778=ORIENTED_EDGE('',*,*,#15612,.T.);
#21779=ORIENTED_EDGE('',*,*,#15633,.F.);
#21780=ORIENTED_EDGE('',*,*,#15528,.T.);
#21781=ORIENTED_EDGE('',*,*,#15531,.T.);
#21782=ORIENTED_EDGE('',*,*,#15570,.T.);
#21783=ORIENTED_EDGE('',*,*,#15634,.F.);
#21784=ORIENTED_EDGE('',*,*,#15597,.T.);
#21785=ORIENTED_EDGE('',*,*,#15618,.T.);
#21786=ORIENTED_EDGE('',*,*,#15635,.T.);
#21787=ORIENTED_EDGE('',*,*,#15636,.T.);
#21788=ORIENTED_EDGE('',*,*,#15637,.T.);
#21789=ORIENTED_EDGE('',*,*,#15635,.F.);
#21790=ORIENTED_EDGE('',*,*,#15637,.F.);
#21791=ORIENTED_EDGE('',*,*,#15638,.T.);
#21792=ORIENTED_EDGE('',*,*,#15639,.T.);
#21793=ORIENTED_EDGE('',*,*,#15640,.T.);
#21794=ORIENTED_EDGE('',*,*,#15638,.F.);
#21795=ORIENTED_EDGE('',*,*,#15640,.F.);
#21796=ORIENTED_EDGE('',*,*,#15641,.T.);
#21797=ORIENTED_EDGE('',*,*,#15642,.T.);
#21798=ORIENTED_EDGE('',*,*,#15643,.T.);
#21799=ORIENTED_EDGE('',*,*,#15641,.F.);
#21800=ORIENTED_EDGE('',*,*,#15643,.F.);
#21801=ORIENTED_EDGE('',*,*,#15254,.F.);
#21802=ORIENTED_EDGE('',*,*,#15258,.F.);
#21803=ORIENTED_EDGE('',*,*,#15270,.F.);
#21804=ORIENTED_EDGE('',*,*,#15264,.F.);
#21805=ORIENTED_EDGE('',*,*,#15262,.T.);
#21806=ORIENTED_EDGE('',*,*,#15622,.T.);
#21807=ORIENTED_EDGE('',*,*,#15302,.F.);
#21808=ORIENTED_EDGE('',*,*,#15306,.F.);
#21809=ORIENTED_EDGE('',*,*,#15318,.F.);
#21810=ORIENTED_EDGE('',*,*,#15312,.F.);
#21811=ORIENTED_EDGE('',*,*,#15310,.T.);
#21812=ORIENTED_EDGE('',*,*,#15624,.T.);
#21813=ORIENTED_EDGE('',*,*,#15350,.F.);
#21814=ORIENTED_EDGE('',*,*,#15354,.F.);
#21815=ORIENTED_EDGE('',*,*,#15366,.F.);
#21816=ORIENTED_EDGE('',*,*,#15360,.F.);
#21817=ORIENTED_EDGE('',*,*,#15358,.T.);
#21818=ORIENTED_EDGE('',*,*,#15626,.T.);
#21819=ORIENTED_EDGE('',*,*,#15398,.F.);
#21820=ORIENTED_EDGE('',*,*,#15402,.F.);
#21821=ORIENTED_EDGE('',*,*,#15414,.F.);
#21822=ORIENTED_EDGE('',*,*,#15408,.F.);
#21823=ORIENTED_EDGE('',*,*,#15406,.T.);
#21824=ORIENTED_EDGE('',*,*,#15628,.T.);
#21825=ORIENTED_EDGE('',*,*,#15446,.F.);
#21826=ORIENTED_EDGE('',*,*,#15450,.F.);
#21827=ORIENTED_EDGE('',*,*,#15462,.F.);
#21828=ORIENTED_EDGE('',*,*,#15456,.F.);
#21829=ORIENTED_EDGE('',*,*,#15454,.T.);
#21830=ORIENTED_EDGE('',*,*,#15630,.T.);
#21831=ORIENTED_EDGE('',*,*,#15494,.F.);
#21832=ORIENTED_EDGE('',*,*,#15498,.F.);
#21833=ORIENTED_EDGE('',*,*,#15510,.F.);
#21834=ORIENTED_EDGE('',*,*,#15504,.F.);
#21835=ORIENTED_EDGE('',*,*,#15502,.T.);
#21836=ORIENTED_EDGE('',*,*,#15632,.T.);
#21837=ORIENTED_EDGE('',*,*,#15590,.F.);
#21838=ORIENTED_EDGE('',*,*,#15594,.F.);
#21839=ORIENTED_EDGE('',*,*,#15606,.F.);
#21840=ORIENTED_EDGE('',*,*,#15600,.F.);
#21841=ORIENTED_EDGE('',*,*,#15598,.T.);
#21842=ORIENTED_EDGE('',*,*,#15634,.T.);
#21843=ORIENTED_EDGE('',*,*,#15569,.F.);
#21844=ORIENTED_EDGE('',*,*,#15567,.F.);
#21845=ORIENTED_EDGE('',*,*,#15565,.F.);
#21846=ORIENTED_EDGE('',*,*,#15561,.F.);
#21847=ORIENTED_EDGE('',*,*,#15559,.T.);
#21848=ORIENTED_EDGE('',*,*,#15620,.T.);
#21849=ORIENTED_EDGE('',*,*,#15233,.F.);
#21850=ORIENTED_EDGE('',*,*,#15642,.F.);
#21851=ORIENTED_EDGE('',*,*,#15644,.F.);
#21852=ORIENTED_EDGE('',*,*,#15636,.F.);
#21853=ORIENTED_EDGE('',*,*,#15639,.F.);
#21854=ORIENTED_EDGE('',*,*,#15645,.T.);
#21855=ORIENTED_EDGE('',*,*,#15646,.T.);
#21856=ORIENTED_EDGE('',*,*,#15644,.T.);
#21857=ORIENTED_EDGE('',*,*,#15646,.F.);
#21858=ORIENTED_EDGE('',*,*,#15647,.F.);
#21859=ORIENTED_EDGE('',*,*,#15647,.T.);
#21860=ORIENTED_EDGE('',*,*,#15648,.T.);
#21861=ORIENTED_EDGE('',*,*,#15649,.F.);
#21862=ORIENTED_EDGE('',*,*,#15648,.F.);
#21863=ORIENTED_EDGE('',*,*,#15650,.F.);
#21864=ORIENTED_EDGE('',*,*,#15650,.T.);
#21865=ORIENTED_EDGE('',*,*,#15651,.T.);
#21866=ORIENTED_EDGE('',*,*,#15652,.F.);
#21867=ORIENTED_EDGE('',*,*,#15651,.F.);
#21868=ORIENTED_EDGE('',*,*,#15653,.F.);
#21869=ORIENTED_EDGE('',*,*,#15653,.T.);
#21870=ORIENTED_EDGE('',*,*,#15654,.T.);
#21871=ORIENTED_EDGE('',*,*,#15655,.F.);
#21872=ORIENTED_EDGE('',*,*,#15654,.F.);
#21873=ORIENTED_EDGE('',*,*,#15541,.T.);
#21874=ORIENTED_EDGE('',*,*,#15523,.T.);
#21875=ORIENTED_EDGE('',*,*,#15529,.T.);
#21876=ORIENTED_EDGE('',*,*,#15633,.T.);
#21877=ORIENTED_EDGE('',*,*,#15611,.F.);
#21878=ORIENTED_EDGE('',*,*,#15615,.T.);
#21879=ORIENTED_EDGE('',*,*,#15581,.T.);
#21880=ORIENTED_EDGE('',*,*,#15575,.T.);
#21881=ORIENTED_EDGE('',*,*,#15573,.T.);
#21882=ORIENTED_EDGE('',*,*,#15631,.T.);
#21883=ORIENTED_EDGE('',*,*,#15515,.F.);
#21884=ORIENTED_EDGE('',*,*,#15519,.T.);
#21885=ORIENTED_EDGE('',*,*,#15485,.T.);
#21886=ORIENTED_EDGE('',*,*,#15479,.T.);
#21887=ORIENTED_EDGE('',*,*,#15477,.T.);
#21888=ORIENTED_EDGE('',*,*,#15629,.T.);
#21889=ORIENTED_EDGE('',*,*,#15467,.F.);
#21890=ORIENTED_EDGE('',*,*,#15471,.T.);
#21891=ORIENTED_EDGE('',*,*,#15437,.T.);
#21892=ORIENTED_EDGE('',*,*,#15431,.T.);
#21893=ORIENTED_EDGE('',*,*,#15429,.T.);
#21894=ORIENTED_EDGE('',*,*,#15627,.T.);
#21895=ORIENTED_EDGE('',*,*,#15419,.F.);
#21896=ORIENTED_EDGE('',*,*,#15423,.T.);
#21897=ORIENTED_EDGE('',*,*,#15389,.T.);
#21898=ORIENTED_EDGE('',*,*,#15383,.T.);
#21899=ORIENTED_EDGE('',*,*,#15381,.T.);
#21900=ORIENTED_EDGE('',*,*,#15625,.T.);
#21901=ORIENTED_EDGE('',*,*,#15371,.F.);
#21902=ORIENTED_EDGE('',*,*,#15375,.T.);
#21903=ORIENTED_EDGE('',*,*,#15341,.T.);
#21904=ORIENTED_EDGE('',*,*,#15335,.T.);
#21905=ORIENTED_EDGE('',*,*,#15333,.T.);
#21906=ORIENTED_EDGE('',*,*,#15623,.T.);
#21907=ORIENTED_EDGE('',*,*,#15323,.F.);
#21908=ORIENTED_EDGE('',*,*,#15327,.T.);
#21909=ORIENTED_EDGE('',*,*,#15293,.T.);
#21910=ORIENTED_EDGE('',*,*,#15287,.T.);
#21911=ORIENTED_EDGE('',*,*,#15285,.T.);
#21912=ORIENTED_EDGE('',*,*,#15621,.T.);
#21913=ORIENTED_EDGE('',*,*,#15275,.F.);
#21914=ORIENTED_EDGE('',*,*,#15279,.T.);
#21915=ORIENTED_EDGE('',*,*,#15245,.T.);
#21916=ORIENTED_EDGE('',*,*,#15239,.T.);
#21917=ORIENTED_EDGE('',*,*,#15237,.T.);
#21918=ORIENTED_EDGE('',*,*,#15619,.T.);
#21919=ORIENTED_EDGE('',*,*,#15548,.F.);
#21920=ORIENTED_EDGE('',*,*,#15552,.T.);
#21921=ORIENTED_EDGE('',*,*,#15231,.T.);
#21922=ORIENTED_EDGE('',*,*,#15655,.T.);
#21923=ORIENTED_EDGE('',*,*,#15645,.F.);
#21924=ORIENTED_EDGE('',*,*,#15649,.T.);
#21925=ORIENTED_EDGE('',*,*,#15652,.T.);
#21926=ORIENTED_EDGE('',*,*,#15656,.T.);
#21927=ORIENTED_EDGE('',*,*,#15657,.T.);
#21928=ORIENTED_EDGE('',*,*,#15658,.T.);
#21929=ORIENTED_EDGE('',*,*,#15659,.T.);
#21930=ORIENTED_EDGE('',*,*,#15660,.T.);
#21931=ORIENTED_EDGE('',*,*,#15661,.T.);
#21932=ORIENTED_EDGE('',*,*,#15662,.T.);
#21933=ORIENTED_EDGE('',*,*,#15663,.T.);
#21934=ORIENTED_EDGE('',*,*,#15656,.F.);
#21935=ORIENTED_EDGE('',*,*,#15664,.T.);
#21936=ORIENTED_EDGE('',*,*,#15663,.F.);
#21937=ORIENTED_EDGE('',*,*,#15664,.F.);
#21938=ORIENTED_EDGE('',*,*,#15665,.F.);
#21939=ORIENTED_EDGE('',*,*,#15666,.F.);
#21940=ORIENTED_EDGE('',*,*,#15667,.F.);
#21941=ORIENTED_EDGE('',*,*,#15668,.F.);
#21942=ORIENTED_EDGE('',*,*,#15669,.F.);
#21943=ORIENTED_EDGE('',*,*,#15670,.F.);
#21944=ORIENTED_EDGE('',*,*,#15662,.F.);
#21945=ORIENTED_EDGE('',*,*,#15671,.F.);
#21946=ORIENTED_EDGE('',*,*,#15665,.T.);
#21947=ORIENTED_EDGE('',*,*,#15672,.T.);
#21948=ORIENTED_EDGE('',*,*,#15661,.F.);
#21949=ORIENTED_EDGE('',*,*,#15673,.F.);
#21950=ORIENTED_EDGE('',*,*,#15666,.T.);
#21951=ORIENTED_EDGE('',*,*,#15671,.T.);
#21952=ORIENTED_EDGE('',*,*,#15660,.F.);
#21953=ORIENTED_EDGE('',*,*,#15674,.F.);
#21954=ORIENTED_EDGE('',*,*,#15667,.T.);
#21955=ORIENTED_EDGE('',*,*,#15673,.T.);
#21956=ORIENTED_EDGE('',*,*,#15659,.F.);
#21957=ORIENTED_EDGE('',*,*,#15675,.F.);
#21958=ORIENTED_EDGE('',*,*,#15668,.T.);
#21959=ORIENTED_EDGE('',*,*,#15674,.T.);
#21960=ORIENTED_EDGE('',*,*,#15658,.F.);
#21961=ORIENTED_EDGE('',*,*,#15676,.F.);
#21962=ORIENTED_EDGE('',*,*,#15669,.T.);
#21963=ORIENTED_EDGE('',*,*,#15675,.T.);
#21964=ORIENTED_EDGE('',*,*,#15657,.F.);
#21965=ORIENTED_EDGE('',*,*,#15672,.F.);
#21966=ORIENTED_EDGE('',*,*,#15670,.T.);
#21967=ORIENTED_EDGE('',*,*,#15676,.T.);
#21968=ORIENTED_EDGE('',*,*,#15677,.T.);
#21969=ORIENTED_EDGE('',*,*,#15678,.T.);
#21970=ORIENTED_EDGE('',*,*,#15677,.F.);
#21971=ORIENTED_EDGE('',*,*,#15679,.T.);
#21972=ORIENTED_EDGE('',*,*,#15680,.T.);
#21973=ORIENTED_EDGE('',*,*,#15679,.F.);
#21974=ORIENTED_EDGE('',*,*,#15680,.F.);
#21975=ORIENTED_EDGE('',*,*,#15681,.T.);
#21976=ORIENTED_EDGE('',*,*,#15682,.T.);
#21977=ORIENTED_EDGE('',*,*,#15681,.F.);
#21978=ORIENTED_EDGE('',*,*,#15682,.F.);
#21979=ORIENTED_EDGE('',*,*,#15683,.T.);
#21980=ORIENTED_EDGE('',*,*,#15684,.T.);
#21981=ORIENTED_EDGE('',*,*,#15685,.T.);
#21982=ORIENTED_EDGE('',*,*,#15686,.T.);
#21983=ORIENTED_EDGE('',*,*,#15687,.T.);
#21984=ORIENTED_EDGE('',*,*,#15688,.T.);
#21985=ORIENTED_EDGE('',*,*,#15689,.T.);
#21986=ORIENTED_EDGE('',*,*,#15690,.T.);
#21987=ORIENTED_EDGE('',*,*,#15691,.T.);
#21988=ORIENTED_EDGE('',*,*,#15692,.T.);
#21989=ORIENTED_EDGE('',*,*,#15693,.T.);
#21990=ORIENTED_EDGE('',*,*,#15694,.T.);
#21991=ORIENTED_EDGE('',*,*,#15694,.F.);
#21992=ORIENTED_EDGE('',*,*,#15695,.F.);
#21993=ORIENTED_EDGE('',*,*,#15684,.F.);
#21994=ORIENTED_EDGE('',*,*,#15696,.T.);
#21995=ORIENTED_EDGE('',*,*,#15693,.F.);
#21996=ORIENTED_EDGE('',*,*,#15697,.F.);
#21997=ORIENTED_EDGE('',*,*,#15685,.F.);
#21998=ORIENTED_EDGE('',*,*,#15695,.T.);
#21999=ORIENTED_EDGE('',*,*,#15692,.F.);
#22000=ORIENTED_EDGE('',*,*,#15698,.F.);
#22001=ORIENTED_EDGE('',*,*,#15686,.F.);
#22002=ORIENTED_EDGE('',*,*,#15697,.T.);
#22003=ORIENTED_EDGE('',*,*,#15691,.F.);
#22004=ORIENTED_EDGE('',*,*,#15699,.F.);
#22005=ORIENTED_EDGE('',*,*,#15687,.F.);
#22006=ORIENTED_EDGE('',*,*,#15698,.T.);
#22007=ORIENTED_EDGE('',*,*,#15690,.F.);
#22008=ORIENTED_EDGE('',*,*,#15700,.F.);
#22009=ORIENTED_EDGE('',*,*,#15688,.F.);
#22010=ORIENTED_EDGE('',*,*,#15699,.T.);
#22011=ORIENTED_EDGE('',*,*,#15689,.F.);
#22012=ORIENTED_EDGE('',*,*,#15696,.F.);
#22013=ORIENTED_EDGE('',*,*,#15683,.F.);
#22014=ORIENTED_EDGE('',*,*,#15700,.T.);
#22015=ORIENTED_EDGE('',*,*,#15701,.T.);
#22016=ORIENTED_EDGE('',*,*,#15702,.T.);
#22017=ORIENTED_EDGE('',*,*,#15703,.T.);
#22018=ORIENTED_EDGE('',*,*,#15701,.F.);
#22019=ORIENTED_EDGE('',*,*,#15703,.F.);
#22020=ORIENTED_EDGE('',*,*,#15702,.F.);
#22021=ORIENTED_EDGE('',*,*,#15704,.T.);
#22022=ORIENTED_EDGE('',*,*,#15678,.F.);
#22023=ORIENTED_EDGE('',*,*,#15704,.F.);
#22024=ORIENTED_EDGE('',*,*,#15705,.T.);
#22025=ORIENTED_EDGE('',*,*,#15706,.T.);
#22026=ORIENTED_EDGE('',*,*,#15705,.F.);
#22027=ORIENTED_EDGE('',*,*,#15707,.T.);
#22028=ORIENTED_EDGE('',*,*,#15708,.T.);
#22029=ORIENTED_EDGE('',*,*,#15707,.F.);
#22030=ORIENTED_EDGE('',*,*,#15708,.F.);
#22031=ORIENTED_EDGE('',*,*,#15709,.T.);
#22032=ORIENTED_EDGE('',*,*,#15710,.T.);
#22033=ORIENTED_EDGE('',*,*,#15709,.F.);
#22034=ORIENTED_EDGE('',*,*,#15710,.F.);
#22035=ORIENTED_EDGE('',*,*,#15711,.T.);
#22036=ORIENTED_EDGE('',*,*,#15712,.T.);
#22037=ORIENTED_EDGE('',*,*,#15713,.T.);
#22038=ORIENTED_EDGE('',*,*,#15714,.T.);
#22039=ORIENTED_EDGE('',*,*,#15715,.T.);
#22040=ORIENTED_EDGE('',*,*,#15716,.T.);
#22041=ORIENTED_EDGE('',*,*,#15717,.T.);
#22042=ORIENTED_EDGE('',*,*,#15718,.T.);
#22043=ORIENTED_EDGE('',*,*,#15719,.T.);
#22044=ORIENTED_EDGE('',*,*,#15720,.T.);
#22045=ORIENTED_EDGE('',*,*,#15721,.T.);
#22046=ORIENTED_EDGE('',*,*,#15722,.T.);
#22047=ORIENTED_EDGE('',*,*,#15722,.F.);
#22048=ORIENTED_EDGE('',*,*,#15723,.F.);
#22049=ORIENTED_EDGE('',*,*,#15712,.F.);
#22050=ORIENTED_EDGE('',*,*,#15724,.T.);
#22051=ORIENTED_EDGE('',*,*,#15721,.F.);
#22052=ORIENTED_EDGE('',*,*,#15725,.F.);
#22053=ORIENTED_EDGE('',*,*,#15713,.F.);
#22054=ORIENTED_EDGE('',*,*,#15723,.T.);
#22055=ORIENTED_EDGE('',*,*,#15720,.F.);
#22056=ORIENTED_EDGE('',*,*,#15726,.F.);
#22057=ORIENTED_EDGE('',*,*,#15714,.F.);
#22058=ORIENTED_EDGE('',*,*,#15725,.T.);
#22059=ORIENTED_EDGE('',*,*,#15719,.F.);
#22060=ORIENTED_EDGE('',*,*,#15727,.F.);
#22061=ORIENTED_EDGE('',*,*,#15715,.F.);
#22062=ORIENTED_EDGE('',*,*,#15726,.T.);
#22063=ORIENTED_EDGE('',*,*,#15718,.F.);
#22064=ORIENTED_EDGE('',*,*,#15728,.F.);
#22065=ORIENTED_EDGE('',*,*,#15716,.F.);
#22066=ORIENTED_EDGE('',*,*,#15727,.T.);
#22067=ORIENTED_EDGE('',*,*,#15717,.F.);
#22068=ORIENTED_EDGE('',*,*,#15724,.F.);
#22069=ORIENTED_EDGE('',*,*,#15711,.F.);
#22070=ORIENTED_EDGE('',*,*,#15728,.T.);
#22071=ORIENTED_EDGE('',*,*,#15729,.T.);
#22072=ORIENTED_EDGE('',*,*,#15730,.T.);
#22073=ORIENTED_EDGE('',*,*,#15731,.T.);
#22074=ORIENTED_EDGE('',*,*,#15729,.F.);
#22075=ORIENTED_EDGE('',*,*,#15731,.F.);
#22076=ORIENTED_EDGE('',*,*,#15730,.F.);
#22077=ORIENTED_EDGE('',*,*,#15732,.T.);
#22078=ORIENTED_EDGE('',*,*,#15706,.F.);
#22079=ORIENTED_EDGE('',*,*,#15732,.F.);
#22080=ORIENTED_EDGE('',*,*,#15733,.T.);
#22081=ORIENTED_EDGE('',*,*,#15734,.T.);
#22082=ORIENTED_EDGE('',*,*,#15735,.T.);
#22083=ORIENTED_EDGE('',*,*,#15736,.T.);
#22084=ORIENTED_EDGE('',*,*,#15737,.T.);
#22085=ORIENTED_EDGE('',*,*,#15738,.T.);
#22086=ORIENTED_EDGE('',*,*,#15734,.F.);
#22087=ORIENTED_EDGE('',*,*,#15739,.T.);
#22088=ORIENTED_EDGE('',*,*,#15740,.T.);
#22089=ORIENTED_EDGE('',*,*,#15741,.F.);
#22090=ORIENTED_EDGE('',*,*,#15742,.T.);
#22091=ORIENTED_EDGE('',*,*,#15743,.T.);
#22092=ORIENTED_EDGE('',*,*,#15744,.T.);
#22093=ORIENTED_EDGE('',*,*,#15745,.F.);
#22094=ORIENTED_EDGE('',*,*,#15746,.T.);
#22095=ORIENTED_EDGE('',*,*,#15747,.T.);
#22096=ORIENTED_EDGE('',*,*,#15748,.T.);
#22097=ORIENTED_EDGE('',*,*,#15749,.T.);
#22098=ORIENTED_EDGE('',*,*,#15747,.F.);
#22099=ORIENTED_EDGE('',*,*,#15750,.T.);
#22100=ORIENTED_EDGE('',*,*,#15751,.T.);
#22101=ORIENTED_EDGE('',*,*,#15743,.F.);
#22102=ORIENTED_EDGE('',*,*,#15752,.T.);
#22103=ORIENTED_EDGE('',*,*,#15753,.T.);
#22104=ORIENTED_EDGE('',*,*,#15746,.F.);
#22105=ORIENTED_EDGE('',*,*,#15754,.F.);
#22106=ORIENTED_EDGE('',*,*,#15755,.T.);
#22107=ORIENTED_EDGE('',*,*,#15750,.F.);
#22108=ORIENTED_EDGE('',*,*,#15742,.F.);
#22109=ORIENTED_EDGE('',*,*,#15756,.F.);
#22110=ORIENTED_EDGE('',*,*,#15757,.T.);
#22111=ORIENTED_EDGE('',*,*,#15752,.F.);
#22112=ORIENTED_EDGE('',*,*,#15758,.T.);
#22113=ORIENTED_EDGE('',*,*,#15759,.F.);
#22114=ORIENTED_EDGE('',*,*,#15744,.F.);
#22115=ORIENTED_EDGE('',*,*,#15749,.F.);
#22116=ORIENTED_EDGE('',*,*,#15760,.T.);
#22117=ORIENTED_EDGE('',*,*,#15761,.F.);
#22118=ORIENTED_EDGE('',*,*,#15740,.F.);
#22119=ORIENTED_EDGE('',*,*,#15751,.F.);
#22120=ORIENTED_EDGE('',*,*,#15745,.T.);
#22121=ORIENTED_EDGE('',*,*,#15759,.T.);
#22122=ORIENTED_EDGE('',*,*,#15762,.T.);
#22123=ORIENTED_EDGE('',*,*,#15756,.T.);
#22124=ORIENTED_EDGE('',*,*,#15741,.T.);
#22125=ORIENTED_EDGE('',*,*,#15761,.T.);
#22126=ORIENTED_EDGE('',*,*,#15763,.T.);
#22127=ORIENTED_EDGE('',*,*,#15764,.T.);
#22128=ORIENTED_EDGE('',*,*,#15737,.F.);
#22129=ORIENTED_EDGE('',*,*,#15765,.T.);
#22130=ORIENTED_EDGE('',*,*,#15766,.T.);
#22131=ORIENTED_EDGE('',*,*,#15754,.T.);
#22132=ORIENTED_EDGE('',*,*,#15767,.T.);
#22133=ORIENTED_EDGE('',*,*,#15768,.T.);
#22134=ORIENTED_EDGE('',*,*,#15769,.T.);
#22135=ORIENTED_EDGE('',*,*,#15770,.T.);
#22136=ORIENTED_EDGE('',*,*,#15736,.F.);
#22137=ORIENTED_EDGE('',*,*,#15771,.T.);
#22138=ORIENTED_EDGE('',*,*,#15772,.F.);
#22139=ORIENTED_EDGE('',*,*,#15773,.T.);
#22140=ORIENTED_EDGE('',*,*,#15774,.T.);
#22141=ORIENTED_EDGE('',*,*,#15772,.T.);
#22142=ORIENTED_EDGE('',*,*,#15775,.T.);
#22143=ORIENTED_EDGE('',*,*,#15763,.F.);
#22144=ORIENTED_EDGE('',*,*,#15760,.F.);
#22145=ORIENTED_EDGE('',*,*,#15753,.F.);
#22146=ORIENTED_EDGE('',*,*,#15757,.F.);
#22147=ORIENTED_EDGE('',*,*,#15762,.F.);
#22148=ORIENTED_EDGE('',*,*,#15758,.F.);
#22149=ORIENTED_EDGE('',*,*,#15748,.F.);
#22150=ORIENTED_EDGE('',*,*,#15755,.F.);
#22151=ORIENTED_EDGE('',*,*,#15766,.F.);
#22152=ORIENTED_EDGE('',*,*,#15767,.F.);
#22153=ORIENTED_EDGE('',*,*,#15768,.F.);
#22154=ORIENTED_EDGE('',*,*,#15776,.T.);
#22155=ORIENTED_EDGE('',*,*,#15777,.T.);
#22156=ORIENTED_EDGE('',*,*,#15776,.F.);
#22157=ORIENTED_EDGE('',*,*,#15769,.F.);
#22158=ORIENTED_EDGE('',*,*,#15778,.T.);
#22159=ORIENTED_EDGE('',*,*,#15779,.F.);
#22160=ORIENTED_EDGE('',*,*,#15780,.F.);
#22161=ORIENTED_EDGE('',*,*,#15781,.T.);
#22162=ORIENTED_EDGE('',*,*,#15779,.T.);
#22163=ORIENTED_EDGE('',*,*,#15781,.F.);
#22164=ORIENTED_EDGE('',*,*,#15780,.T.);
#22165=ORIENTED_EDGE('',*,*,#15782,.F.);
#22166=ORIENTED_EDGE('',*,*,#15783,.T.);
#22167=ORIENTED_EDGE('',*,*,#15784,.T.);
#22168=ORIENTED_EDGE('',*,*,#15782,.T.);
#22169=ORIENTED_EDGE('',*,*,#15784,.F.);
#22170=ORIENTED_EDGE('',*,*,#15739,.F.);
#22171=ORIENTED_EDGE('',*,*,#15733,.F.);
#22172=ORIENTED_EDGE('',*,*,#15773,.F.);
#22173=ORIENTED_EDGE('',*,*,#15774,.F.);
#22174=ORIENTED_EDGE('',*,*,#15765,.F.);
#22175=ORIENTED_EDGE('',*,*,#15777,.F.);
#22176=ORIENTED_EDGE('',*,*,#15738,.F.);
#22177=ORIENTED_EDGE('',*,*,#15764,.F.);
#22178=ORIENTED_EDGE('',*,*,#15775,.F.);
#22179=ORIENTED_EDGE('',*,*,#15771,.F.);
#22180=ORIENTED_EDGE('',*,*,#15735,.F.);
#22181=ORIENTED_EDGE('',*,*,#15783,.F.);
#22182=ORIENTED_EDGE('',*,*,#15778,.F.);
#22183=ORIENTED_EDGE('',*,*,#15770,.F.);
#22184=ORIENTED_EDGE('',*,*,#15785,.F.);
#22185=ORIENTED_EDGE('',*,*,#15786,.F.);
#22186=ORIENTED_EDGE('',*,*,#15787,.F.);
#22187=ORIENTED_EDGE('',*,*,#15788,.F.);
#22188=ORIENTED_EDGE('',*,*,#15789,.F.);
#22189=ORIENTED_EDGE('',*,*,#15790,.F.);
#22190=ORIENTED_EDGE('',*,*,#15791,.F.);
#22191=ORIENTED_EDGE('',*,*,#15792,.F.);
#22192=ORIENTED_EDGE('',*,*,#15793,.F.);
#22193=ORIENTED_EDGE('',*,*,#15794,.F.);
#22194=ORIENTED_EDGE('',*,*,#15795,.T.);
#22195=ORIENTED_EDGE('',*,*,#15792,.T.);
#22196=ORIENTED_EDGE('',*,*,#15795,.F.);
#22197=ORIENTED_EDGE('',*,*,#15796,.T.);
#22198=ORIENTED_EDGE('',*,*,#15797,.T.);
#22199=ORIENTED_EDGE('',*,*,#15798,.T.);
#22200=ORIENTED_EDGE('',*,*,#15797,.F.);
#22201=ORIENTED_EDGE('',*,*,#15799,.T.);
#22202=ORIENTED_EDGE('',*,*,#15798,.F.);
#22203=ORIENTED_EDGE('',*,*,#15799,.F.);
#22204=ORIENTED_EDGE('',*,*,#15800,.T.);
#22205=ORIENTED_EDGE('',*,*,#15801,.T.);
#22206=ORIENTED_EDGE('',*,*,#15800,.F.);
#22207=ORIENTED_EDGE('',*,*,#15802,.F.);
#22208=ORIENTED_EDGE('',*,*,#15785,.T.);
#22209=ORIENTED_EDGE('',*,*,#15801,.F.);
#22210=ORIENTED_EDGE('',*,*,#15803,.F.);
#22211=ORIENTED_EDGE('',*,*,#15804,.F.);
#22212=ORIENTED_EDGE('',*,*,#15805,.F.);
#22213=ORIENTED_EDGE('',*,*,#15806,.F.);
#22214=ORIENTED_EDGE('',*,*,#15807,.F.);
#22215=ORIENTED_EDGE('',*,*,#15796,.F.);
#22216=ORIENTED_EDGE('',*,*,#15807,.T.);
#22217=ORIENTED_EDGE('',*,*,#15808,.T.);
#22218=ORIENTED_EDGE('',*,*,#15809,.T.);
#22219=ORIENTED_EDGE('',*,*,#15810,.T.);
#22220=ORIENTED_EDGE('',*,*,#15811,.T.);
#22221=ORIENTED_EDGE('',*,*,#15812,.T.);
#22222=ORIENTED_EDGE('',*,*,#15788,.T.);
#22223=ORIENTED_EDGE('',*,*,#15813,.T.);
#22224=ORIENTED_EDGE('',*,*,#15813,.F.);
#22225=ORIENTED_EDGE('',*,*,#15787,.T.);
#22226=ORIENTED_EDGE('',*,*,#15814,.T.);
#22227=ORIENTED_EDGE('',*,*,#15803,.T.);
#22228=ORIENTED_EDGE('',*,*,#15805,.T.);
#22229=ORIENTED_EDGE('',*,*,#15815,.F.);
#22230=ORIENTED_EDGE('',*,*,#15816,.F.);
#22231=ORIENTED_EDGE('',*,*,#15817,.F.);
#22232=ORIENTED_EDGE('',*,*,#15818,.F.);
#22233=ORIENTED_EDGE('',*,*,#15819,.F.);
#22234=ORIENTED_EDGE('',*,*,#15820,.F.);
#22235=ORIENTED_EDGE('',*,*,#15821,.F.);
#22236=ORIENTED_EDGE('',*,*,#15822,.F.);
#22237=ORIENTED_EDGE('',*,*,#15823,.F.);
#22238=ORIENTED_EDGE('',*,*,#15790,.T.);
#22239=ORIENTED_EDGE('',*,*,#15824,.T.);
#22240=ORIENTED_EDGE('',*,*,#15825,.T.);
#22241=ORIENTED_EDGE('',*,*,#15826,.T.);
#22242=ORIENTED_EDGE('',*,*,#15827,.T.);
#22243=ORIENTED_EDGE('',*,*,#15828,.T.);
#22244=ORIENTED_EDGE('',*,*,#15824,.F.);
#22245=ORIENTED_EDGE('',*,*,#15789,.T.);
#22246=ORIENTED_EDGE('',*,*,#15812,.F.);
#22247=ORIENTED_EDGE('',*,*,#15829,.F.);
#22248=ORIENTED_EDGE('',*,*,#15830,.F.);
#22249=ORIENTED_EDGE('',*,*,#15831,.F.);
#22250=ORIENTED_EDGE('',*,*,#15806,.T.);
#22251=ORIENTED_EDGE('',*,*,#15828,.F.);
#22252=ORIENTED_EDGE('',*,*,#15832,.F.);
#22253=ORIENTED_EDGE('',*,*,#15833,.F.);
#22254=ORIENTED_EDGE('',*,*,#15834,.F.);
#22255=ORIENTED_EDGE('',*,*,#15808,.F.);
#22256=ORIENTED_EDGE('',*,*,#15835,.T.);
#22257=ORIENTED_EDGE('',*,*,#15836,.T.);
#22258=ORIENTED_EDGE('',*,*,#15837,.T.);
#22259=ORIENTED_EDGE('',*,*,#15838,.T.);
#22260=ORIENTED_EDGE('',*,*,#15839,.T.);
#22261=ORIENTED_EDGE('',*,*,#15840,.T.);
#22262=ORIENTED_EDGE('',*,*,#15841,.F.);
#22263=ORIENTED_EDGE('',*,*,#15842,.F.);
#22264=ORIENTED_EDGE('',*,*,#15843,.F.);
#22265=ORIENTED_EDGE('',*,*,#15840,.F.);
#22266=ORIENTED_EDGE('',*,*,#15844,.T.);
#22267=ORIENTED_EDGE('',*,*,#15845,.T.);
#22268=ORIENTED_EDGE('',*,*,#15833,.T.);
#22269=ORIENTED_EDGE('',*,*,#15846,.T.);
#22270=ORIENTED_EDGE('',*,*,#15847,.T.);
#22271=ORIENTED_EDGE('',*,*,#15848,.T.);
#22272=ORIENTED_EDGE('',*,*,#15830,.T.);
#22273=ORIENTED_EDGE('',*,*,#15849,.T.);
#22274=ORIENTED_EDGE('',*,*,#15845,.F.);
#22275=ORIENTED_EDGE('',*,*,#15850,.T.);
#22276=ORIENTED_EDGE('',*,*,#15809,.F.);
#22277=ORIENTED_EDGE('',*,*,#15834,.T.);
#22278=ORIENTED_EDGE('',*,*,#15846,.F.);
#22279=ORIENTED_EDGE('',*,*,#15832,.T.);
#22280=ORIENTED_EDGE('',*,*,#15827,.F.);
#22281=ORIENTED_EDGE('',*,*,#15851,.T.);
#22282=ORIENTED_EDGE('',*,*,#15839,.F.);
#22283=ORIENTED_EDGE('',*,*,#15852,.F.);
#22284=ORIENTED_EDGE('',*,*,#15810,.F.);
#22285=ORIENTED_EDGE('',*,*,#15850,.F.);
#22286=ORIENTED_EDGE('',*,*,#15844,.F.);
#22287=ORIENTED_EDGE('',*,*,#15847,.F.);
#22288=ORIENTED_EDGE('',*,*,#15851,.F.);
#22289=ORIENTED_EDGE('',*,*,#15826,.F.);
#22290=ORIENTED_EDGE('',*,*,#15853,.F.);
#22291=ORIENTED_EDGE('',*,*,#15849,.F.);
#22292=ORIENTED_EDGE('',*,*,#15829,.T.);
#22293=ORIENTED_EDGE('',*,*,#15811,.F.);
#22294=ORIENTED_EDGE('',*,*,#15852,.T.);
#22295=ORIENTED_EDGE('',*,*,#15848,.F.);
#22296=ORIENTED_EDGE('',*,*,#15853,.T.);
#22297=ORIENTED_EDGE('',*,*,#15825,.F.);
#22298=ORIENTED_EDGE('',*,*,#15831,.T.);
#22299=ORIENTED_EDGE('',*,*,#15854,.F.);
#22300=ORIENTED_EDGE('',*,*,#15855,.F.);
#22301=ORIENTED_EDGE('',*,*,#15822,.T.);
#22302=ORIENTED_EDGE('',*,*,#15856,.F.);
#22303=ORIENTED_EDGE('',*,*,#15857,.F.);
#22304=ORIENTED_EDGE('',*,*,#15858,.F.);
#22305=ORIENTED_EDGE('',*,*,#15818,.T.);
#22306=ORIENTED_EDGE('',*,*,#15859,.F.);
#22307=ORIENTED_EDGE('',*,*,#15816,.T.);
#22308=ORIENTED_EDGE('',*,*,#15860,.F.);
#22309=ORIENTED_EDGE('',*,*,#15861,.F.);
#22310=ORIENTED_EDGE('',*,*,#15862,.F.);
#22311=ORIENTED_EDGE('',*,*,#15863,.F.);
#22312=ORIENTED_EDGE('',*,*,#15856,.T.);
#22313=ORIENTED_EDGE('',*,*,#15821,.T.);
#22314=ORIENTED_EDGE('',*,*,#15864,.T.);
#22315=ORIENTED_EDGE('',*,*,#15862,.T.);
#22316=ORIENTED_EDGE('',*,*,#15865,.F.);
#22317=ORIENTED_EDGE('',*,*,#15859,.T.);
#22318=ORIENTED_EDGE('',*,*,#15817,.T.);
#22319=ORIENTED_EDGE('',*,*,#15820,.T.);
#22320=ORIENTED_EDGE('',*,*,#15866,.F.);
#22321=ORIENTED_EDGE('',*,*,#15867,.F.);
#22322=ORIENTED_EDGE('',*,*,#15864,.F.);
#22323=ORIENTED_EDGE('',*,*,#15857,.T.);
#22324=ORIENTED_EDGE('',*,*,#15865,.T.);
#22325=ORIENTED_EDGE('',*,*,#15861,.T.);
#22326=ORIENTED_EDGE('',*,*,#15868,.F.);
#22327=ORIENTED_EDGE('',*,*,#15854,.T.);
#22328=ORIENTED_EDGE('',*,*,#15863,.T.);
#22329=ORIENTED_EDGE('',*,*,#15867,.T.);
#22330=ORIENTED_EDGE('',*,*,#15869,.F.);
#22331=ORIENTED_EDGE('',*,*,#15814,.F.);
#22332=ORIENTED_EDGE('',*,*,#15791,.T.);
#22333=ORIENTED_EDGE('',*,*,#15823,.T.);
#22334=ORIENTED_EDGE('',*,*,#15855,.T.);
#22335=ORIENTED_EDGE('',*,*,#15869,.T.);
#22336=ORIENTED_EDGE('',*,*,#15866,.T.);
#22337=ORIENTED_EDGE('',*,*,#15819,.T.);
#22338=ORIENTED_EDGE('',*,*,#15858,.T.);
#22339=ORIENTED_EDGE('',*,*,#15868,.T.);
#22340=ORIENTED_EDGE('',*,*,#15860,.T.);
#22341=ORIENTED_EDGE('',*,*,#15815,.T.);
#22342=ORIENTED_EDGE('',*,*,#15804,.T.);
#22343=ORIENTED_EDGE('',*,*,#15793,.T.);
#22344=ORIENTED_EDGE('',*,*,#15794,.T.);
#22345=ORIENTED_EDGE('',*,*,#15870,.T.);
#22346=ORIENTED_EDGE('',*,*,#15871,.T.);
#22347=ORIENTED_EDGE('',*,*,#15872,.T.);
#22348=ORIENTED_EDGE('',*,*,#15873,.T.);
#22349=ORIENTED_EDGE('',*,*,#15874,.T.);
#22350=ORIENTED_EDGE('',*,*,#15875,.T.);
#22351=ORIENTED_EDGE('',*,*,#15876,.T.);
#22352=ORIENTED_EDGE('',*,*,#15877,.T.);
#22353=ORIENTED_EDGE('',*,*,#15878,.T.);
#22354=ORIENTED_EDGE('',*,*,#15879,.T.);
#22355=ORIENTED_EDGE('',*,*,#15880,.T.);
#22356=ORIENTED_EDGE('',*,*,#15881,.T.);
#22357=ORIENTED_EDGE('',*,*,#15882,.T.);
#22358=ORIENTED_EDGE('',*,*,#15883,.T.);
#22359=ORIENTED_EDGE('',*,*,#15884,.T.);
#22360=ORIENTED_EDGE('',*,*,#15885,.T.);
#22361=ORIENTED_EDGE('',*,*,#15886,.T.);
#22362=ORIENTED_EDGE('',*,*,#15841,.T.);
#22363=ORIENTED_EDGE('',*,*,#15843,.T.);
#22364=ORIENTED_EDGE('',*,*,#15842,.T.);
#22365=ORIENTED_EDGE('',*,*,#15802,.T.);
#22366=ORIENTED_EDGE('',*,*,#15786,.T.);
#22367=ORIENTED_EDGE('',*,*,#15887,.T.);
#22368=ORIENTED_EDGE('',*,*,#15888,.T.);
#22369=ORIENTED_EDGE('',*,*,#15889,.T.);
#22370=ORIENTED_EDGE('',*,*,#15890,.T.);
#22371=ORIENTED_EDGE('',*,*,#15891,.T.);
#22372=ORIENTED_EDGE('',*,*,#15892,.T.);
#22373=ORIENTED_EDGE('',*,*,#15893,.T.);
#22374=ORIENTED_EDGE('',*,*,#15894,.T.);
#22375=ORIENTED_EDGE('',*,*,#15895,.T.);
#22376=ORIENTED_EDGE('',*,*,#15896,.T.);
#22377=ORIENTED_EDGE('',*,*,#15897,.T.);
#22378=ORIENTED_EDGE('',*,*,#15898,.T.);
#22379=ORIENTED_EDGE('',*,*,#15899,.T.);
#22380=ORIENTED_EDGE('',*,*,#15900,.T.);
#22381=ORIENTED_EDGE('',*,*,#15901,.T.);
#22382=ORIENTED_EDGE('',*,*,#15902,.T.);
#22383=ORIENTED_EDGE('',*,*,#15903,.T.);
#22384=ORIENTED_EDGE('',*,*,#15904,.T.);
#22385=ORIENTED_EDGE('',*,*,#15905,.T.);
#22386=ORIENTED_EDGE('',*,*,#15906,.T.);
#22387=ORIENTED_EDGE('',*,*,#15907,.T.);
#22388=ORIENTED_EDGE('',*,*,#15908,.T.);
#22389=ORIENTED_EDGE('',*,*,#15909,.T.);
#22390=ORIENTED_EDGE('',*,*,#15910,.T.);
#22391=ORIENTED_EDGE('',*,*,#15911,.T.);
#22392=ORIENTED_EDGE('',*,*,#15912,.T.);
#22393=ORIENTED_EDGE('',*,*,#15913,.T.);
#22394=ORIENTED_EDGE('',*,*,#15914,.T.);
#22395=ORIENTED_EDGE('',*,*,#15915,.T.);
#22396=ORIENTED_EDGE('',*,*,#15916,.T.);
#22397=ORIENTED_EDGE('',*,*,#15917,.T.);
#22398=ORIENTED_EDGE('',*,*,#15881,.F.);
#22399=ORIENTED_EDGE('',*,*,#15918,.F.);
#22400=ORIENTED_EDGE('',*,*,#15916,.F.);
#22401=ORIENTED_EDGE('',*,*,#15919,.T.);
#22402=ORIENTED_EDGE('',*,*,#15880,.F.);
#22403=ORIENTED_EDGE('',*,*,#15920,.F.);
#22404=ORIENTED_EDGE('',*,*,#15917,.F.);
#22405=ORIENTED_EDGE('',*,*,#15918,.T.);
#22406=ORIENTED_EDGE('',*,*,#15882,.F.);
#22407=ORIENTED_EDGE('',*,*,#15919,.F.);
#22408=ORIENTED_EDGE('',*,*,#15915,.F.);
#22409=ORIENTED_EDGE('',*,*,#15921,.T.);
#22410=ORIENTED_EDGE('',*,*,#15883,.F.);
#22411=ORIENTED_EDGE('',*,*,#15921,.F.);
#22412=ORIENTED_EDGE('',*,*,#15914,.F.);
#22413=ORIENTED_EDGE('',*,*,#15922,.T.);
#22414=ORIENTED_EDGE('',*,*,#15884,.F.);
#22415=ORIENTED_EDGE('',*,*,#15922,.F.);
#22416=ORIENTED_EDGE('',*,*,#15913,.F.);
#22417=ORIENTED_EDGE('',*,*,#15923,.T.);
#22418=ORIENTED_EDGE('',*,*,#15885,.F.);
#22419=ORIENTED_EDGE('',*,*,#15923,.F.);
#22420=ORIENTED_EDGE('',*,*,#15912,.F.);
#22421=ORIENTED_EDGE('',*,*,#15924,.T.);
#22422=ORIENTED_EDGE('',*,*,#15886,.F.);
#22423=ORIENTED_EDGE('',*,*,#15924,.F.);
#22424=ORIENTED_EDGE('',*,*,#15911,.F.);
#22425=ORIENTED_EDGE('',*,*,#15925,.T.);
#22426=ORIENTED_EDGE('',*,*,#15879,.F.);
#22427=ORIENTED_EDGE('',*,*,#15925,.F.);
#22428=ORIENTED_EDGE('',*,*,#15910,.F.);
#22429=ORIENTED_EDGE('',*,*,#15920,.T.);
#22430=ORIENTED_EDGE('',*,*,#15895,.F.);
#22431=ORIENTED_EDGE('',*,*,#15926,.F.);
#22432=ORIENTED_EDGE('',*,*,#15927,.F.);
#22433=ORIENTED_EDGE('',*,*,#15928,.T.);
#22434=ORIENTED_EDGE('',*,*,#15894,.F.);
#22435=ORIENTED_EDGE('',*,*,#15929,.F.);
#22436=ORIENTED_EDGE('',*,*,#15930,.F.);
#22437=ORIENTED_EDGE('',*,*,#15926,.T.);
#22438=ORIENTED_EDGE('',*,*,#15893,.F.);
#22439=ORIENTED_EDGE('',*,*,#15931,.F.);
#22440=ORIENTED_EDGE('',*,*,#15932,.F.);
#22441=ORIENTED_EDGE('',*,*,#15929,.T.);
#22442=ORIENTED_EDGE('',*,*,#15902,.F.);
#22443=ORIENTED_EDGE('',*,*,#15933,.F.);
#22444=ORIENTED_EDGE('',*,*,#15934,.F.);
#22445=ORIENTED_EDGE('',*,*,#15935,.T.);
#22446=ORIENTED_EDGE('',*,*,#15901,.F.);
#22447=ORIENTED_EDGE('',*,*,#15936,.F.);
#22448=ORIENTED_EDGE('',*,*,#15937,.F.);
#22449=ORIENTED_EDGE('',*,*,#15933,.T.);
#22450=ORIENTED_EDGE('',*,*,#15900,.F.);
#22451=ORIENTED_EDGE('',*,*,#15938,.F.);
#22452=ORIENTED_EDGE('',*,*,#15939,.F.);
#22453=ORIENTED_EDGE('',*,*,#15936,.T.);
#22454=ORIENTED_EDGE('',*,*,#15899,.F.);
#22455=ORIENTED_EDGE('',*,*,#15940,.F.);
#22456=ORIENTED_EDGE('',*,*,#15941,.F.);
#22457=ORIENTED_EDGE('',*,*,#15938,.T.);
#22458=ORIENTED_EDGE('',*,*,#15898,.F.);
#22459=ORIENTED_EDGE('',*,*,#15942,.F.);
#22460=ORIENTED_EDGE('',*,*,#15943,.F.);
#22461=ORIENTED_EDGE('',*,*,#15940,.T.);
#22462=ORIENTED_EDGE('',*,*,#15897,.F.);
#22463=ORIENTED_EDGE('',*,*,#15944,.F.);
#22464=ORIENTED_EDGE('',*,*,#15945,.F.);
#22465=ORIENTED_EDGE('',*,*,#15942,.T.);
#22466=ORIENTED_EDGE('',*,*,#15896,.F.);
#22467=ORIENTED_EDGE('',*,*,#15928,.F.);
#22468=ORIENTED_EDGE('',*,*,#15946,.F.);
#22469=ORIENTED_EDGE('',*,*,#15944,.T.);
#22470=ORIENTED_EDGE('',*,*,#15903,.F.);
#22471=ORIENTED_EDGE('',*,*,#15935,.F.);
#22472=ORIENTED_EDGE('',*,*,#15947,.F.);
#22473=ORIENTED_EDGE('',*,*,#15931,.T.);
#22474=ORIENTED_EDGE('',*,*,#15932,.T.);
#22475=ORIENTED_EDGE('',*,*,#15947,.T.);
#22476=ORIENTED_EDGE('',*,*,#15934,.T.);
#22477=ORIENTED_EDGE('',*,*,#15937,.T.);
#22478=ORIENTED_EDGE('',*,*,#15939,.T.);
#22479=ORIENTED_EDGE('',*,*,#15941,.T.);
#22480=ORIENTED_EDGE('',*,*,#15943,.T.);
#22481=ORIENTED_EDGE('',*,*,#15945,.T.);
#22482=ORIENTED_EDGE('',*,*,#15946,.T.);
#22483=ORIENTED_EDGE('',*,*,#15927,.T.);
#22484=ORIENTED_EDGE('',*,*,#15930,.T.);
#22485=ORIENTED_EDGE('',*,*,#15948,.T.);
#22486=ORIENTED_EDGE('',*,*,#15949,.T.);
#22487=ORIENTED_EDGE('',*,*,#15950,.T.);
#22488=ORIENTED_EDGE('',*,*,#15951,.T.);
#22489=ORIENTED_EDGE('',*,*,#15952,.T.);
#22490=ORIENTED_EDGE('',*,*,#15953,.T.);
#22491=ORIENTED_EDGE('',*,*,#15889,.F.);
#22492=ORIENTED_EDGE('',*,*,#15954,.F.);
#22493=ORIENTED_EDGE('',*,*,#15950,.F.);
#22494=ORIENTED_EDGE('',*,*,#15955,.T.);
#22495=ORIENTED_EDGE('',*,*,#15888,.F.);
#22496=ORIENTED_EDGE('',*,*,#15956,.F.);
#22497=ORIENTED_EDGE('',*,*,#15951,.F.);
#22498=ORIENTED_EDGE('',*,*,#15954,.T.);
#22499=ORIENTED_EDGE('',*,*,#15890,.F.);
#22500=ORIENTED_EDGE('',*,*,#15955,.F.);
#22501=ORIENTED_EDGE('',*,*,#15949,.F.);
#22502=ORIENTED_EDGE('',*,*,#15957,.T.);
#22503=ORIENTED_EDGE('',*,*,#15891,.F.);
#22504=ORIENTED_EDGE('',*,*,#15957,.F.);
#22505=ORIENTED_EDGE('',*,*,#15948,.F.);
#22506=ORIENTED_EDGE('',*,*,#15958,.T.);
#22507=ORIENTED_EDGE('',*,*,#15892,.F.);
#22508=ORIENTED_EDGE('',*,*,#15958,.F.);
#22509=ORIENTED_EDGE('',*,*,#15953,.F.);
#22510=ORIENTED_EDGE('',*,*,#15959,.T.);
#22511=ORIENTED_EDGE('',*,*,#15887,.F.);
#22512=ORIENTED_EDGE('',*,*,#15959,.F.);
#22513=ORIENTED_EDGE('',*,*,#15952,.F.);
#22514=ORIENTED_EDGE('',*,*,#15956,.T.);
#22515=ORIENTED_EDGE('',*,*,#15908,.F.);
#22516=ORIENTED_EDGE('',*,*,#15960,.F.);
#22517=ORIENTED_EDGE('',*,*,#15961,.F.);
#22518=ORIENTED_EDGE('',*,*,#15962,.T.);
#22519=ORIENTED_EDGE('',*,*,#15907,.F.);
#22520=ORIENTED_EDGE('',*,*,#15963,.F.);
#22521=ORIENTED_EDGE('',*,*,#15964,.F.);
#22522=ORIENTED_EDGE('',*,*,#15960,.T.);
#22523=ORIENTED_EDGE('',*,*,#15906,.F.);
#22524=ORIENTED_EDGE('',*,*,#15965,.F.);
#22525=ORIENTED_EDGE('',*,*,#15966,.F.);
#22526=ORIENTED_EDGE('',*,*,#15963,.T.);
#22527=ORIENTED_EDGE('',*,*,#15905,.F.);
#22528=ORIENTED_EDGE('',*,*,#15967,.F.);
#22529=ORIENTED_EDGE('',*,*,#15968,.F.);
#22530=ORIENTED_EDGE('',*,*,#15965,.T.);
#22531=ORIENTED_EDGE('',*,*,#15909,.F.);
#22532=ORIENTED_EDGE('',*,*,#15962,.F.);
#22533=ORIENTED_EDGE('',*,*,#15969,.F.);
#22534=ORIENTED_EDGE('',*,*,#15970,.T.);
#22535=ORIENTED_EDGE('',*,*,#15904,.F.);
#22536=ORIENTED_EDGE('',*,*,#15970,.F.);
#22537=ORIENTED_EDGE('',*,*,#15971,.F.);
#22538=ORIENTED_EDGE('',*,*,#15967,.T.);
#22539=ORIENTED_EDGE('',*,*,#15966,.T.);
#22540=ORIENTED_EDGE('',*,*,#15968,.T.);
#22541=ORIENTED_EDGE('',*,*,#15971,.T.);
#22542=ORIENTED_EDGE('',*,*,#15969,.T.);
#22543=ORIENTED_EDGE('',*,*,#15961,.T.);
#22544=ORIENTED_EDGE('',*,*,#15964,.T.);
#22545=ORIENTED_EDGE('',*,*,#15873,.F.);
#22546=ORIENTED_EDGE('',*,*,#15972,.F.);
#22547=ORIENTED_EDGE('',*,*,#15973,.F.);
#22548=ORIENTED_EDGE('',*,*,#15974,.T.);
#22549=ORIENTED_EDGE('',*,*,#15872,.F.);
#22550=ORIENTED_EDGE('',*,*,#15975,.F.);
#22551=ORIENTED_EDGE('',*,*,#15976,.F.);
#22552=ORIENTED_EDGE('',*,*,#15972,.T.);
#22553=ORIENTED_EDGE('',*,*,#15871,.F.);
#22554=ORIENTED_EDGE('',*,*,#15977,.F.);
#22555=ORIENTED_EDGE('',*,*,#15978,.F.);
#22556=ORIENTED_EDGE('',*,*,#15975,.T.);
#22557=ORIENTED_EDGE('',*,*,#15870,.F.);
#22558=ORIENTED_EDGE('',*,*,#15979,.F.);
#22559=ORIENTED_EDGE('',*,*,#15980,.F.);
#22560=ORIENTED_EDGE('',*,*,#15977,.T.);
#22561=ORIENTED_EDGE('',*,*,#15878,.F.);
#22562=ORIENTED_EDGE('',*,*,#15981,.F.);
#22563=ORIENTED_EDGE('',*,*,#15982,.F.);
#22564=ORIENTED_EDGE('',*,*,#15979,.T.);
#22565=ORIENTED_EDGE('',*,*,#15838,.F.);
#22566=ORIENTED_EDGE('',*,*,#15983,.F.);
#22567=ORIENTED_EDGE('',*,*,#15984,.F.);
#22568=ORIENTED_EDGE('',*,*,#15985,.T.);
#22569=ORIENTED_EDGE('',*,*,#15837,.F.);
#22570=ORIENTED_EDGE('',*,*,#15986,.F.);
#22571=ORIENTED_EDGE('',*,*,#15987,.F.);
#22572=ORIENTED_EDGE('',*,*,#15983,.T.);
#22573=ORIENTED_EDGE('',*,*,#15877,.F.);
#22574=ORIENTED_EDGE('',*,*,#15988,.F.);
#22575=ORIENTED_EDGE('',*,*,#15989,.F.);
#22576=ORIENTED_EDGE('',*,*,#15981,.T.);
#22577=ORIENTED_EDGE('',*,*,#15876,.F.);
#22578=ORIENTED_EDGE('',*,*,#15990,.F.);
#22579=ORIENTED_EDGE('',*,*,#15991,.F.);
#22580=ORIENTED_EDGE('',*,*,#15988,.T.);
#22581=ORIENTED_EDGE('',*,*,#15875,.F.);
#22582=ORIENTED_EDGE('',*,*,#15992,.F.);
#22583=ORIENTED_EDGE('',*,*,#15993,.F.);
#22584=ORIENTED_EDGE('',*,*,#15990,.T.);
#22585=ORIENTED_EDGE('',*,*,#15874,.F.);
#22586=ORIENTED_EDGE('',*,*,#15974,.F.);
#22587=ORIENTED_EDGE('',*,*,#15994,.F.);
#22588=ORIENTED_EDGE('',*,*,#15992,.T.);
#22589=ORIENTED_EDGE('',*,*,#15836,.F.);
#22590=ORIENTED_EDGE('',*,*,#15995,.F.);
#22591=ORIENTED_EDGE('',*,*,#15996,.F.);
#22592=ORIENTED_EDGE('',*,*,#15986,.T.);
#22593=ORIENTED_EDGE('',*,*,#15835,.F.);
#22594=ORIENTED_EDGE('',*,*,#15985,.F.);
#22595=ORIENTED_EDGE('',*,*,#15997,.F.);
#22596=ORIENTED_EDGE('',*,*,#15995,.T.);
#22597=ORIENTED_EDGE('',*,*,#15980,.T.);
#22598=ORIENTED_EDGE('',*,*,#15982,.T.);
#22599=ORIENTED_EDGE('',*,*,#15989,.T.);
#22600=ORIENTED_EDGE('',*,*,#15991,.T.);
#22601=ORIENTED_EDGE('',*,*,#15993,.T.);
#22602=ORIENTED_EDGE('',*,*,#15994,.T.);
#22603=ORIENTED_EDGE('',*,*,#15973,.T.);
#22604=ORIENTED_EDGE('',*,*,#15976,.T.);
#22605=ORIENTED_EDGE('',*,*,#15978,.T.);
#22606=ORIENTED_EDGE('',*,*,#15987,.T.);
#22607=ORIENTED_EDGE('',*,*,#15996,.T.);
#22608=ORIENTED_EDGE('',*,*,#15997,.T.);
#22609=ORIENTED_EDGE('',*,*,#15984,.T.);
#22610=ORIENTED_EDGE('',*,*,#15998,.T.);
#22611=ORIENTED_EDGE('',*,*,#15999,.T.);
#22612=ORIENTED_EDGE('',*,*,#16000,.T.);
#22613=ORIENTED_EDGE('',*,*,#16001,.T.);
#22614=ORIENTED_EDGE('',*,*,#16002,.T.);
#22615=ORIENTED_EDGE('',*,*,#16003,.T.);
#22616=ORIENTED_EDGE('',*,*,#16004,.T.);
#22617=ORIENTED_EDGE('',*,*,#16005,.T.);
#22618=ORIENTED_EDGE('',*,*,#15998,.F.);
#22619=ORIENTED_EDGE('',*,*,#16006,.T.);
#22620=ORIENTED_EDGE('',*,*,#16005,.F.);
#22621=ORIENTED_EDGE('',*,*,#16006,.F.);
#22622=ORIENTED_EDGE('',*,*,#16007,.F.);
#22623=ORIENTED_EDGE('',*,*,#16008,.F.);
#22624=ORIENTED_EDGE('',*,*,#16009,.F.);
#22625=ORIENTED_EDGE('',*,*,#16010,.F.);
#22626=ORIENTED_EDGE('',*,*,#16011,.F.);
#22627=ORIENTED_EDGE('',*,*,#16012,.F.);
#22628=ORIENTED_EDGE('',*,*,#16004,.F.);
#22629=ORIENTED_EDGE('',*,*,#16013,.F.);
#22630=ORIENTED_EDGE('',*,*,#16007,.T.);
#22631=ORIENTED_EDGE('',*,*,#16014,.T.);
#22632=ORIENTED_EDGE('',*,*,#16003,.F.);
#22633=ORIENTED_EDGE('',*,*,#16015,.F.);
#22634=ORIENTED_EDGE('',*,*,#16008,.T.);
#22635=ORIENTED_EDGE('',*,*,#16013,.T.);
#22636=ORIENTED_EDGE('',*,*,#16002,.F.);
#22637=ORIENTED_EDGE('',*,*,#16016,.F.);
#22638=ORIENTED_EDGE('',*,*,#16009,.T.);
#22639=ORIENTED_EDGE('',*,*,#16015,.T.);
#22640=ORIENTED_EDGE('',*,*,#16001,.F.);
#22641=ORIENTED_EDGE('',*,*,#16017,.F.);
#22642=ORIENTED_EDGE('',*,*,#16010,.T.);
#22643=ORIENTED_EDGE('',*,*,#16016,.T.);
#22644=ORIENTED_EDGE('',*,*,#16000,.F.);
#22645=ORIENTED_EDGE('',*,*,#16018,.F.);
#22646=ORIENTED_EDGE('',*,*,#16011,.T.);
#22647=ORIENTED_EDGE('',*,*,#16017,.T.);
#22648=ORIENTED_EDGE('',*,*,#15999,.F.);
#22649=ORIENTED_EDGE('',*,*,#16014,.F.);
#22650=ORIENTED_EDGE('',*,*,#16012,.T.);
#22651=ORIENTED_EDGE('',*,*,#16018,.T.);
#22652=ORIENTED_EDGE('',*,*,#16019,.T.);
#22653=ORIENTED_EDGE('',*,*,#16020,.T.);
#22654=ORIENTED_EDGE('',*,*,#16019,.F.);
#22655=ORIENTED_EDGE('',*,*,#16021,.T.);
#22656=ORIENTED_EDGE('',*,*,#16022,.T.);
#22657=ORIENTED_EDGE('',*,*,#16021,.F.);
#22658=ORIENTED_EDGE('',*,*,#16022,.F.);
#22659=ORIENTED_EDGE('',*,*,#16023,.T.);
#22660=ORIENTED_EDGE('',*,*,#16024,.T.);
#22661=ORIENTED_EDGE('',*,*,#16023,.F.);
#22662=ORIENTED_EDGE('',*,*,#16024,.F.);
#22663=ORIENTED_EDGE('',*,*,#16025,.T.);
#22664=ORIENTED_EDGE('',*,*,#16026,.T.);
#22665=ORIENTED_EDGE('',*,*,#16027,.T.);
#22666=ORIENTED_EDGE('',*,*,#16028,.T.);
#22667=ORIENTED_EDGE('',*,*,#16029,.T.);
#22668=ORIENTED_EDGE('',*,*,#16030,.T.);
#22669=ORIENTED_EDGE('',*,*,#16031,.T.);
#22670=ORIENTED_EDGE('',*,*,#16032,.T.);
#22671=ORIENTED_EDGE('',*,*,#16033,.T.);
#22672=ORIENTED_EDGE('',*,*,#16034,.T.);
#22673=ORIENTED_EDGE('',*,*,#16035,.T.);
#22674=ORIENTED_EDGE('',*,*,#16036,.T.);
#22675=ORIENTED_EDGE('',*,*,#16036,.F.);
#22676=ORIENTED_EDGE('',*,*,#16037,.F.);
#22677=ORIENTED_EDGE('',*,*,#16026,.F.);
#22678=ORIENTED_EDGE('',*,*,#16038,.T.);
#22679=ORIENTED_EDGE('',*,*,#16035,.F.);
#22680=ORIENTED_EDGE('',*,*,#16039,.F.);
#22681=ORIENTED_EDGE('',*,*,#16027,.F.);
#22682=ORIENTED_EDGE('',*,*,#16037,.T.);
#22683=ORIENTED_EDGE('',*,*,#16034,.F.);
#22684=ORIENTED_EDGE('',*,*,#16040,.F.);
#22685=ORIENTED_EDGE('',*,*,#16028,.F.);
#22686=ORIENTED_EDGE('',*,*,#16039,.T.);
#22687=ORIENTED_EDGE('',*,*,#16033,.F.);
#22688=ORIENTED_EDGE('',*,*,#16041,.F.);
#22689=ORIENTED_EDGE('',*,*,#16029,.F.);
#22690=ORIENTED_EDGE('',*,*,#16040,.T.);
#22691=ORIENTED_EDGE('',*,*,#16032,.F.);
#22692=ORIENTED_EDGE('',*,*,#16042,.F.);
#22693=ORIENTED_EDGE('',*,*,#16030,.F.);
#22694=ORIENTED_EDGE('',*,*,#16041,.T.);
#22695=ORIENTED_EDGE('',*,*,#16031,.F.);
#22696=ORIENTED_EDGE('',*,*,#16038,.F.);
#22697=ORIENTED_EDGE('',*,*,#16025,.F.);
#22698=ORIENTED_EDGE('',*,*,#16042,.T.);
#22699=ORIENTED_EDGE('',*,*,#16043,.T.);
#22700=ORIENTED_EDGE('',*,*,#16044,.T.);
#22701=ORIENTED_EDGE('',*,*,#16045,.T.);
#22702=ORIENTED_EDGE('',*,*,#16043,.F.);
#22703=ORIENTED_EDGE('',*,*,#16045,.F.);
#22704=ORIENTED_EDGE('',*,*,#16044,.F.);
#22705=ORIENTED_EDGE('',*,*,#16046,.T.);
#22706=ORIENTED_EDGE('',*,*,#16020,.F.);
#22707=ORIENTED_EDGE('',*,*,#16046,.F.);
#22708=ORIENTED_EDGE('',*,*,#16047,.T.);
#22709=ORIENTED_EDGE('',*,*,#16048,.T.);
#22710=ORIENTED_EDGE('',*,*,#16047,.F.);
#22711=ORIENTED_EDGE('',*,*,#16049,.T.);
#22712=ORIENTED_EDGE('',*,*,#16050,.T.);
#22713=ORIENTED_EDGE('',*,*,#16049,.F.);
#22714=ORIENTED_EDGE('',*,*,#16050,.F.);
#22715=ORIENTED_EDGE('',*,*,#16051,.T.);
#22716=ORIENTED_EDGE('',*,*,#16052,.T.);
#22717=ORIENTED_EDGE('',*,*,#16051,.F.);
#22718=ORIENTED_EDGE('',*,*,#16052,.F.);
#22719=ORIENTED_EDGE('',*,*,#16053,.T.);
#22720=ORIENTED_EDGE('',*,*,#16054,.T.);
#22721=ORIENTED_EDGE('',*,*,#16055,.T.);
#22722=ORIENTED_EDGE('',*,*,#16056,.T.);
#22723=ORIENTED_EDGE('',*,*,#16057,.T.);
#22724=ORIENTED_EDGE('',*,*,#16058,.T.);
#22725=ORIENTED_EDGE('',*,*,#16059,.T.);
#22726=ORIENTED_EDGE('',*,*,#16060,.T.);
#22727=ORIENTED_EDGE('',*,*,#16061,.T.);
#22728=ORIENTED_EDGE('',*,*,#16062,.T.);
#22729=ORIENTED_EDGE('',*,*,#16063,.T.);
#22730=ORIENTED_EDGE('',*,*,#16064,.T.);
#22731=ORIENTED_EDGE('',*,*,#16064,.F.);
#22732=ORIENTED_EDGE('',*,*,#16065,.F.);
#22733=ORIENTED_EDGE('',*,*,#16054,.F.);
#22734=ORIENTED_EDGE('',*,*,#16066,.T.);
#22735=ORIENTED_EDGE('',*,*,#16063,.F.);
#22736=ORIENTED_EDGE('',*,*,#16067,.F.);
#22737=ORIENTED_EDGE('',*,*,#16055,.F.);
#22738=ORIENTED_EDGE('',*,*,#16065,.T.);
#22739=ORIENTED_EDGE('',*,*,#16062,.F.);
#22740=ORIENTED_EDGE('',*,*,#16068,.F.);
#22741=ORIENTED_EDGE('',*,*,#16056,.F.);
#22742=ORIENTED_EDGE('',*,*,#16067,.T.);
#22743=ORIENTED_EDGE('',*,*,#16061,.F.);
#22744=ORIENTED_EDGE('',*,*,#16069,.F.);
#22745=ORIENTED_EDGE('',*,*,#16057,.F.);
#22746=ORIENTED_EDGE('',*,*,#16068,.T.);
#22747=ORIENTED_EDGE('',*,*,#16060,.F.);
#22748=ORIENTED_EDGE('',*,*,#16070,.F.);
#22749=ORIENTED_EDGE('',*,*,#16058,.F.);
#22750=ORIENTED_EDGE('',*,*,#16069,.T.);
#22751=ORIENTED_EDGE('',*,*,#16059,.F.);
#22752=ORIENTED_EDGE('',*,*,#16066,.F.);
#22753=ORIENTED_EDGE('',*,*,#16053,.F.);
#22754=ORIENTED_EDGE('',*,*,#16070,.T.);
#22755=ORIENTED_EDGE('',*,*,#16071,.T.);
#22756=ORIENTED_EDGE('',*,*,#16072,.T.);
#22757=ORIENTED_EDGE('',*,*,#16073,.T.);
#22758=ORIENTED_EDGE('',*,*,#16071,.F.);
#22759=ORIENTED_EDGE('',*,*,#16073,.F.);
#22760=ORIENTED_EDGE('',*,*,#16072,.F.);
#22761=ORIENTED_EDGE('',*,*,#16074,.T.);
#22762=ORIENTED_EDGE('',*,*,#16048,.F.);
#22763=ORIENTED_EDGE('',*,*,#16074,.F.);
#22764=ORIENTED_EDGE('',*,*,#16075,.T.);
#22765=ORIENTED_EDGE('',*,*,#16076,.T.);
#22766=ORIENTED_EDGE('',*,*,#16077,.T.);
#22767=ORIENTED_EDGE('',*,*,#16078,.T.);
#22768=ORIENTED_EDGE('',*,*,#16079,.T.);
#22769=ORIENTED_EDGE('',*,*,#16080,.T.);
#22770=ORIENTED_EDGE('',*,*,#16076,.F.);
#22771=ORIENTED_EDGE('',*,*,#16081,.T.);
#22772=ORIENTED_EDGE('',*,*,#16082,.T.);
#22773=ORIENTED_EDGE('',*,*,#16083,.F.);
#22774=ORIENTED_EDGE('',*,*,#16084,.T.);
#22775=ORIENTED_EDGE('',*,*,#16085,.T.);
#22776=ORIENTED_EDGE('',*,*,#16086,.T.);
#22777=ORIENTED_EDGE('',*,*,#16087,.F.);
#22778=ORIENTED_EDGE('',*,*,#16088,.T.);
#22779=ORIENTED_EDGE('',*,*,#16089,.T.);
#22780=ORIENTED_EDGE('',*,*,#16090,.T.);
#22781=ORIENTED_EDGE('',*,*,#16091,.T.);
#22782=ORIENTED_EDGE('',*,*,#16089,.F.);
#22783=ORIENTED_EDGE('',*,*,#16092,.T.);
#22784=ORIENTED_EDGE('',*,*,#16093,.T.);
#22785=ORIENTED_EDGE('',*,*,#16085,.F.);
#22786=ORIENTED_EDGE('',*,*,#16094,.T.);
#22787=ORIENTED_EDGE('',*,*,#16095,.T.);
#22788=ORIENTED_EDGE('',*,*,#16088,.F.);
#22789=ORIENTED_EDGE('',*,*,#16096,.F.);
#22790=ORIENTED_EDGE('',*,*,#16097,.T.);
#22791=ORIENTED_EDGE('',*,*,#16092,.F.);
#22792=ORIENTED_EDGE('',*,*,#16084,.F.);
#22793=ORIENTED_EDGE('',*,*,#16098,.F.);
#22794=ORIENTED_EDGE('',*,*,#16099,.T.);
#22795=ORIENTED_EDGE('',*,*,#16094,.F.);
#22796=ORIENTED_EDGE('',*,*,#16100,.T.);
#22797=ORIENTED_EDGE('',*,*,#16101,.F.);
#22798=ORIENTED_EDGE('',*,*,#16086,.F.);
#22799=ORIENTED_EDGE('',*,*,#16091,.F.);
#22800=ORIENTED_EDGE('',*,*,#16102,.T.);
#22801=ORIENTED_EDGE('',*,*,#16103,.F.);
#22802=ORIENTED_EDGE('',*,*,#16082,.F.);
#22803=ORIENTED_EDGE('',*,*,#16093,.F.);
#22804=ORIENTED_EDGE('',*,*,#16087,.T.);
#22805=ORIENTED_EDGE('',*,*,#16101,.T.);
#22806=ORIENTED_EDGE('',*,*,#16104,.T.);
#22807=ORIENTED_EDGE('',*,*,#16098,.T.);
#22808=ORIENTED_EDGE('',*,*,#16083,.T.);
#22809=ORIENTED_EDGE('',*,*,#16103,.T.);
#22810=ORIENTED_EDGE('',*,*,#16105,.T.);
#22811=ORIENTED_EDGE('',*,*,#16106,.T.);
#22812=ORIENTED_EDGE('',*,*,#16079,.F.);
#22813=ORIENTED_EDGE('',*,*,#16107,.T.);
#22814=ORIENTED_EDGE('',*,*,#16108,.T.);
#22815=ORIENTED_EDGE('',*,*,#16096,.T.);
#22816=ORIENTED_EDGE('',*,*,#16109,.T.);
#22817=ORIENTED_EDGE('',*,*,#16110,.T.);
#22818=ORIENTED_EDGE('',*,*,#16111,.T.);
#22819=ORIENTED_EDGE('',*,*,#16112,.T.);
#22820=ORIENTED_EDGE('',*,*,#16078,.F.);
#22821=ORIENTED_EDGE('',*,*,#16113,.T.);
#22822=ORIENTED_EDGE('',*,*,#16114,.F.);
#22823=ORIENTED_EDGE('',*,*,#16115,.T.);
#22824=ORIENTED_EDGE('',*,*,#16116,.T.);
#22825=ORIENTED_EDGE('',*,*,#16114,.T.);
#22826=ORIENTED_EDGE('',*,*,#16117,.T.);
#22827=ORIENTED_EDGE('',*,*,#16105,.F.);
#22828=ORIENTED_EDGE('',*,*,#16102,.F.);
#22829=ORIENTED_EDGE('',*,*,#16095,.F.);
#22830=ORIENTED_EDGE('',*,*,#16099,.F.);
#22831=ORIENTED_EDGE('',*,*,#16104,.F.);
#22832=ORIENTED_EDGE('',*,*,#16100,.F.);
#22833=ORIENTED_EDGE('',*,*,#16090,.F.);
#22834=ORIENTED_EDGE('',*,*,#16097,.F.);
#22835=ORIENTED_EDGE('',*,*,#16108,.F.);
#22836=ORIENTED_EDGE('',*,*,#16109,.F.);
#22837=ORIENTED_EDGE('',*,*,#16110,.F.);
#22838=ORIENTED_EDGE('',*,*,#16118,.T.);
#22839=ORIENTED_EDGE('',*,*,#16119,.T.);
#22840=ORIENTED_EDGE('',*,*,#16118,.F.);
#22841=ORIENTED_EDGE('',*,*,#16111,.F.);
#22842=ORIENTED_EDGE('',*,*,#16120,.T.);
#22843=ORIENTED_EDGE('',*,*,#16121,.F.);
#22844=ORIENTED_EDGE('',*,*,#16122,.F.);
#22845=ORIENTED_EDGE('',*,*,#16123,.T.);
#22846=ORIENTED_EDGE('',*,*,#16121,.T.);
#22847=ORIENTED_EDGE('',*,*,#16123,.F.);
#22848=ORIENTED_EDGE('',*,*,#16122,.T.);
#22849=ORIENTED_EDGE('',*,*,#16124,.F.);
#22850=ORIENTED_EDGE('',*,*,#16125,.T.);
#22851=ORIENTED_EDGE('',*,*,#16126,.T.);
#22852=ORIENTED_EDGE('',*,*,#16124,.T.);
#22853=ORIENTED_EDGE('',*,*,#16126,.F.);
#22854=ORIENTED_EDGE('',*,*,#16081,.F.);
#22855=ORIENTED_EDGE('',*,*,#16075,.F.);
#22856=ORIENTED_EDGE('',*,*,#16115,.F.);
#22857=ORIENTED_EDGE('',*,*,#16116,.F.);
#22858=ORIENTED_EDGE('',*,*,#16107,.F.);
#22859=ORIENTED_EDGE('',*,*,#16119,.F.);
#22860=ORIENTED_EDGE('',*,*,#16080,.F.);
#22861=ORIENTED_EDGE('',*,*,#16106,.F.);
#22862=ORIENTED_EDGE('',*,*,#16117,.F.);
#22863=ORIENTED_EDGE('',*,*,#16113,.F.);
#22864=ORIENTED_EDGE('',*,*,#16077,.F.);
#22865=ORIENTED_EDGE('',*,*,#16125,.F.);
#22866=ORIENTED_EDGE('',*,*,#16120,.F.);
#22867=ORIENTED_EDGE('',*,*,#16112,.F.);
#22868=ORIENTED_EDGE('',*,*,#16127,.F.);
#22869=ORIENTED_EDGE('',*,*,#16128,.F.);
#22870=ORIENTED_EDGE('',*,*,#16129,.F.);
#22871=ORIENTED_EDGE('',*,*,#16130,.F.);
#22872=ORIENTED_EDGE('',*,*,#16131,.F.);
#22873=ORIENTED_EDGE('',*,*,#16132,.F.);
#22874=ORIENTED_EDGE('',*,*,#16133,.F.);
#22875=ORIENTED_EDGE('',*,*,#16134,.F.);
#22876=ORIENTED_EDGE('',*,*,#16135,.F.);
#22877=ORIENTED_EDGE('',*,*,#16136,.F.);
#22878=ORIENTED_EDGE('',*,*,#16137,.T.);
#22879=ORIENTED_EDGE('',*,*,#16134,.T.);
#22880=ORIENTED_EDGE('',*,*,#16137,.F.);
#22881=ORIENTED_EDGE('',*,*,#16138,.T.);
#22882=ORIENTED_EDGE('',*,*,#16139,.T.);
#22883=ORIENTED_EDGE('',*,*,#16140,.T.);
#22884=ORIENTED_EDGE('',*,*,#16139,.F.);
#22885=ORIENTED_EDGE('',*,*,#16141,.T.);
#22886=ORIENTED_EDGE('',*,*,#16140,.F.);
#22887=ORIENTED_EDGE('',*,*,#16141,.F.);
#22888=ORIENTED_EDGE('',*,*,#16142,.T.);
#22889=ORIENTED_EDGE('',*,*,#16143,.T.);
#22890=ORIENTED_EDGE('',*,*,#16142,.F.);
#22891=ORIENTED_EDGE('',*,*,#16144,.F.);
#22892=ORIENTED_EDGE('',*,*,#16127,.T.);
#22893=ORIENTED_EDGE('',*,*,#16143,.F.);
#22894=ORIENTED_EDGE('',*,*,#16145,.F.);
#22895=ORIENTED_EDGE('',*,*,#16146,.F.);
#22896=ORIENTED_EDGE('',*,*,#16147,.F.);
#22897=ORIENTED_EDGE('',*,*,#16148,.F.);
#22898=ORIENTED_EDGE('',*,*,#16149,.F.);
#22899=ORIENTED_EDGE('',*,*,#16138,.F.);
#22900=ORIENTED_EDGE('',*,*,#16149,.T.);
#22901=ORIENTED_EDGE('',*,*,#16150,.T.);
#22902=ORIENTED_EDGE('',*,*,#16151,.T.);
#22903=ORIENTED_EDGE('',*,*,#16152,.T.);
#22904=ORIENTED_EDGE('',*,*,#16153,.T.);
#22905=ORIENTED_EDGE('',*,*,#16154,.T.);
#22906=ORIENTED_EDGE('',*,*,#16130,.T.);
#22907=ORIENTED_EDGE('',*,*,#16155,.T.);
#22908=ORIENTED_EDGE('',*,*,#16155,.F.);
#22909=ORIENTED_EDGE('',*,*,#16129,.T.);
#22910=ORIENTED_EDGE('',*,*,#16156,.T.);
#22911=ORIENTED_EDGE('',*,*,#16145,.T.);
#22912=ORIENTED_EDGE('',*,*,#16147,.T.);
#22913=ORIENTED_EDGE('',*,*,#16157,.F.);
#22914=ORIENTED_EDGE('',*,*,#16158,.F.);
#22915=ORIENTED_EDGE('',*,*,#16159,.F.);
#22916=ORIENTED_EDGE('',*,*,#16160,.F.);
#22917=ORIENTED_EDGE('',*,*,#16161,.F.);
#22918=ORIENTED_EDGE('',*,*,#16162,.F.);
#22919=ORIENTED_EDGE('',*,*,#16163,.F.);
#22920=ORIENTED_EDGE('',*,*,#16164,.F.);
#22921=ORIENTED_EDGE('',*,*,#16165,.F.);
#22922=ORIENTED_EDGE('',*,*,#16132,.T.);
#22923=ORIENTED_EDGE('',*,*,#16166,.T.);
#22924=ORIENTED_EDGE('',*,*,#16167,.T.);
#22925=ORIENTED_EDGE('',*,*,#16168,.T.);
#22926=ORIENTED_EDGE('',*,*,#16169,.T.);
#22927=ORIENTED_EDGE('',*,*,#16170,.T.);
#22928=ORIENTED_EDGE('',*,*,#16166,.F.);
#22929=ORIENTED_EDGE('',*,*,#16131,.T.);
#22930=ORIENTED_EDGE('',*,*,#16154,.F.);
#22931=ORIENTED_EDGE('',*,*,#16171,.F.);
#22932=ORIENTED_EDGE('',*,*,#16148,.T.);
#22933=ORIENTED_EDGE('',*,*,#16170,.F.);
#22934=ORIENTED_EDGE('',*,*,#16172,.F.);
#22935=ORIENTED_EDGE('',*,*,#16150,.F.);
#22936=ORIENTED_EDGE('',*,*,#16173,.T.);
#22937=ORIENTED_EDGE('',*,*,#16174,.T.);
#22938=ORIENTED_EDGE('',*,*,#16175,.T.);
#22939=ORIENTED_EDGE('',*,*,#16176,.T.);
#22940=ORIENTED_EDGE('',*,*,#16177,.T.);
#22941=ORIENTED_EDGE('',*,*,#16178,.T.);
#22942=ORIENTED_EDGE('',*,*,#16179,.F.);
#22943=ORIENTED_EDGE('',*,*,#16180,.F.);
#22944=ORIENTED_EDGE('',*,*,#16181,.F.);
#22945=ORIENTED_EDGE('',*,*,#16178,.F.);
#22946=ORIENTED_EDGE('',*,*,#16172,.T.);
#22947=ORIENTED_EDGE('',*,*,#16169,.F.);
#22948=ORIENTED_EDGE('',*,*,#16182,.T.);
#22949=ORIENTED_EDGE('',*,*,#16151,.F.);
#22950=ORIENTED_EDGE('',*,*,#16171,.T.);
#22951=ORIENTED_EDGE('',*,*,#16153,.F.);
#22952=ORIENTED_EDGE('',*,*,#16183,.T.);
#22953=ORIENTED_EDGE('',*,*,#16167,.F.);
#22954=ORIENTED_EDGE('',*,*,#16168,.F.);
#22955=ORIENTED_EDGE('',*,*,#16183,.F.);
#22956=ORIENTED_EDGE('',*,*,#16152,.F.);
#22957=ORIENTED_EDGE('',*,*,#16182,.F.);
#22958=ORIENTED_EDGE('',*,*,#16177,.F.);
#22959=ORIENTED_EDGE('',*,*,#16184,.F.);
#22960=ORIENTED_EDGE('',*,*,#16185,.F.);
#22961=ORIENTED_EDGE('',*,*,#16164,.T.);
#22962=ORIENTED_EDGE('',*,*,#16186,.F.);
#22963=ORIENTED_EDGE('',*,*,#16187,.F.);
#22964=ORIENTED_EDGE('',*,*,#16188,.F.);
#22965=ORIENTED_EDGE('',*,*,#16160,.T.);
#22966=ORIENTED_EDGE('',*,*,#16189,.F.);
#22967=ORIENTED_EDGE('',*,*,#16158,.T.);
#22968=ORIENTED_EDGE('',*,*,#16190,.F.);
#22969=ORIENTED_EDGE('',*,*,#16191,.F.);
#22970=ORIENTED_EDGE('',*,*,#16192,.F.);
#22971=ORIENTED_EDGE('',*,*,#16193,.F.);
#22972=ORIENTED_EDGE('',*,*,#16186,.T.);
#22973=ORIENTED_EDGE('',*,*,#16163,.T.);
#22974=ORIENTED_EDGE('',*,*,#16194,.T.);
#22975=ORIENTED_EDGE('',*,*,#16192,.T.);
#22976=ORIENTED_EDGE('',*,*,#16195,.F.);
#22977=ORIENTED_EDGE('',*,*,#16189,.T.);
#22978=ORIENTED_EDGE('',*,*,#16159,.T.);
#22979=ORIENTED_EDGE('',*,*,#16162,.T.);
#22980=ORIENTED_EDGE('',*,*,#16196,.F.);
#22981=ORIENTED_EDGE('',*,*,#16197,.F.);
#22982=ORIENTED_EDGE('',*,*,#16194,.F.);
#22983=ORIENTED_EDGE('',*,*,#16187,.T.);
#22984=ORIENTED_EDGE('',*,*,#16195,.T.);
#22985=ORIENTED_EDGE('',*,*,#16191,.T.);
#22986=ORIENTED_EDGE('',*,*,#16198,.F.);
#22987=ORIENTED_EDGE('',*,*,#16184,.T.);
#22988=ORIENTED_EDGE('',*,*,#16193,.T.);
#22989=ORIENTED_EDGE('',*,*,#16197,.T.);
#22990=ORIENTED_EDGE('',*,*,#16199,.F.);
#22991=ORIENTED_EDGE('',*,*,#16156,.F.);
#22992=ORIENTED_EDGE('',*,*,#16133,.T.);
#22993=ORIENTED_EDGE('',*,*,#16165,.T.);
#22994=ORIENTED_EDGE('',*,*,#16185,.T.);
#22995=ORIENTED_EDGE('',*,*,#16199,.T.);
#22996=ORIENTED_EDGE('',*,*,#16196,.T.);
#22997=ORIENTED_EDGE('',*,*,#16161,.T.);
#22998=ORIENTED_EDGE('',*,*,#16188,.T.);
#22999=ORIENTED_EDGE('',*,*,#16198,.T.);
#23000=ORIENTED_EDGE('',*,*,#16190,.T.);
#23001=ORIENTED_EDGE('',*,*,#16157,.T.);
#23002=ORIENTED_EDGE('',*,*,#16146,.T.);
#23003=ORIENTED_EDGE('',*,*,#16135,.T.);
#23004=ORIENTED_EDGE('',*,*,#16136,.T.);
#23005=ORIENTED_EDGE('',*,*,#16200,.T.);
#23006=ORIENTED_EDGE('',*,*,#16201,.T.);
#23007=ORIENTED_EDGE('',*,*,#16202,.T.);
#23008=ORIENTED_EDGE('',*,*,#16203,.T.);
#23009=ORIENTED_EDGE('',*,*,#16204,.T.);
#23010=ORIENTED_EDGE('',*,*,#16205,.T.);
#23011=ORIENTED_EDGE('',*,*,#16206,.T.);
#23012=ORIENTED_EDGE('',*,*,#16207,.T.);
#23013=ORIENTED_EDGE('',*,*,#16208,.T.);
#23014=ORIENTED_EDGE('',*,*,#16209,.T.);
#23015=ORIENTED_EDGE('',*,*,#16210,.T.);
#23016=ORIENTED_EDGE('',*,*,#16211,.T.);
#23017=ORIENTED_EDGE('',*,*,#16212,.T.);
#23018=ORIENTED_EDGE('',*,*,#16213,.T.);
#23019=ORIENTED_EDGE('',*,*,#16214,.T.);
#23020=ORIENTED_EDGE('',*,*,#16215,.T.);
#23021=ORIENTED_EDGE('',*,*,#16216,.T.);
#23022=ORIENTED_EDGE('',*,*,#16179,.T.);
#23023=ORIENTED_EDGE('',*,*,#16181,.T.);
#23024=ORIENTED_EDGE('',*,*,#16180,.T.);
#23025=ORIENTED_EDGE('',*,*,#16144,.T.);
#23026=ORIENTED_EDGE('',*,*,#16128,.T.);
#23027=ORIENTED_EDGE('',*,*,#16217,.T.);
#23028=ORIENTED_EDGE('',*,*,#16218,.T.);
#23029=ORIENTED_EDGE('',*,*,#16219,.T.);
#23030=ORIENTED_EDGE('',*,*,#16220,.T.);
#23031=ORIENTED_EDGE('',*,*,#16221,.T.);
#23032=ORIENTED_EDGE('',*,*,#16222,.T.);
#23033=ORIENTED_EDGE('',*,*,#16223,.T.);
#23034=ORIENTED_EDGE('',*,*,#16224,.T.);
#23035=ORIENTED_EDGE('',*,*,#16225,.T.);
#23036=ORIENTED_EDGE('',*,*,#16226,.T.);
#23037=ORIENTED_EDGE('',*,*,#16227,.T.);
#23038=ORIENTED_EDGE('',*,*,#16228,.T.);
#23039=ORIENTED_EDGE('',*,*,#16229,.T.);
#23040=ORIENTED_EDGE('',*,*,#16230,.T.);
#23041=ORIENTED_EDGE('',*,*,#16231,.T.);
#23042=ORIENTED_EDGE('',*,*,#16232,.T.);
#23043=ORIENTED_EDGE('',*,*,#16233,.T.);
#23044=ORIENTED_EDGE('',*,*,#16234,.T.);
#23045=ORIENTED_EDGE('',*,*,#16235,.T.);
#23046=ORIENTED_EDGE('',*,*,#16236,.T.);
#23047=ORIENTED_EDGE('',*,*,#16237,.T.);
#23048=ORIENTED_EDGE('',*,*,#16238,.T.);
#23049=ORIENTED_EDGE('',*,*,#16239,.T.);
#23050=ORIENTED_EDGE('',*,*,#16240,.T.);
#23051=ORIENTED_EDGE('',*,*,#16241,.T.);
#23052=ORIENTED_EDGE('',*,*,#16242,.T.);
#23053=ORIENTED_EDGE('',*,*,#16243,.T.);
#23054=ORIENTED_EDGE('',*,*,#16244,.T.);
#23055=ORIENTED_EDGE('',*,*,#16245,.T.);
#23056=ORIENTED_EDGE('',*,*,#16246,.T.);
#23057=ORIENTED_EDGE('',*,*,#16247,.T.);
#23058=ORIENTED_EDGE('',*,*,#16211,.F.);
#23059=ORIENTED_EDGE('',*,*,#16248,.F.);
#23060=ORIENTED_EDGE('',*,*,#16246,.F.);
#23061=ORIENTED_EDGE('',*,*,#16249,.T.);
#23062=ORIENTED_EDGE('',*,*,#16210,.F.);
#23063=ORIENTED_EDGE('',*,*,#16250,.F.);
#23064=ORIENTED_EDGE('',*,*,#16247,.F.);
#23065=ORIENTED_EDGE('',*,*,#16248,.T.);
#23066=ORIENTED_EDGE('',*,*,#16212,.F.);
#23067=ORIENTED_EDGE('',*,*,#16249,.F.);
#23068=ORIENTED_EDGE('',*,*,#16245,.F.);
#23069=ORIENTED_EDGE('',*,*,#16251,.T.);
#23070=ORIENTED_EDGE('',*,*,#16213,.F.);
#23071=ORIENTED_EDGE('',*,*,#16251,.F.);
#23072=ORIENTED_EDGE('',*,*,#16244,.F.);
#23073=ORIENTED_EDGE('',*,*,#16252,.T.);
#23074=ORIENTED_EDGE('',*,*,#16214,.F.);
#23075=ORIENTED_EDGE('',*,*,#16252,.F.);
#23076=ORIENTED_EDGE('',*,*,#16243,.F.);
#23077=ORIENTED_EDGE('',*,*,#16253,.T.);
#23078=ORIENTED_EDGE('',*,*,#16215,.F.);
#23079=ORIENTED_EDGE('',*,*,#16253,.F.);
#23080=ORIENTED_EDGE('',*,*,#16242,.F.);
#23081=ORIENTED_EDGE('',*,*,#16254,.T.);
#23082=ORIENTED_EDGE('',*,*,#16216,.F.);
#23083=ORIENTED_EDGE('',*,*,#16254,.F.);
#23084=ORIENTED_EDGE('',*,*,#16241,.F.);
#23085=ORIENTED_EDGE('',*,*,#16255,.T.);
#23086=ORIENTED_EDGE('',*,*,#16209,.F.);
#23087=ORIENTED_EDGE('',*,*,#16255,.F.);
#23088=ORIENTED_EDGE('',*,*,#16240,.F.);
#23089=ORIENTED_EDGE('',*,*,#16250,.T.);
#23090=ORIENTED_EDGE('',*,*,#16225,.F.);
#23091=ORIENTED_EDGE('',*,*,#16256,.F.);
#23092=ORIENTED_EDGE('',*,*,#16257,.F.);
#23093=ORIENTED_EDGE('',*,*,#16258,.T.);
#23094=ORIENTED_EDGE('',*,*,#16224,.F.);
#23095=ORIENTED_EDGE('',*,*,#16259,.F.);
#23096=ORIENTED_EDGE('',*,*,#16260,.F.);
#23097=ORIENTED_EDGE('',*,*,#16256,.T.);
#23098=ORIENTED_EDGE('',*,*,#16223,.F.);
#23099=ORIENTED_EDGE('',*,*,#16261,.F.);
#23100=ORIENTED_EDGE('',*,*,#16262,.F.);
#23101=ORIENTED_EDGE('',*,*,#16259,.T.);
#23102=ORIENTED_EDGE('',*,*,#16232,.F.);
#23103=ORIENTED_EDGE('',*,*,#16263,.F.);
#23104=ORIENTED_EDGE('',*,*,#16264,.F.);
#23105=ORIENTED_EDGE('',*,*,#16265,.T.);
#23106=ORIENTED_EDGE('',*,*,#16231,.F.);
#23107=ORIENTED_EDGE('',*,*,#16266,.F.);
#23108=ORIENTED_EDGE('',*,*,#16267,.F.);
#23109=ORIENTED_EDGE('',*,*,#16263,.T.);
#23110=ORIENTED_EDGE('',*,*,#16230,.F.);
#23111=ORIENTED_EDGE('',*,*,#16268,.F.);
#23112=ORIENTED_EDGE('',*,*,#16269,.F.);
#23113=ORIENTED_EDGE('',*,*,#16266,.T.);
#23114=ORIENTED_EDGE('',*,*,#16229,.F.);
#23115=ORIENTED_EDGE('',*,*,#16270,.F.);
#23116=ORIENTED_EDGE('',*,*,#16271,.F.);
#23117=ORIENTED_EDGE('',*,*,#16268,.T.);
#23118=ORIENTED_EDGE('',*,*,#16228,.F.);
#23119=ORIENTED_EDGE('',*,*,#16272,.F.);
#23120=ORIENTED_EDGE('',*,*,#16273,.F.);
#23121=ORIENTED_EDGE('',*,*,#16270,.T.);
#23122=ORIENTED_EDGE('',*,*,#16227,.F.);
#23123=ORIENTED_EDGE('',*,*,#16274,.F.);
#23124=ORIENTED_EDGE('',*,*,#16275,.F.);
#23125=ORIENTED_EDGE('',*,*,#16272,.T.);
#23126=ORIENTED_EDGE('',*,*,#16226,.F.);
#23127=ORIENTED_EDGE('',*,*,#16258,.F.);
#23128=ORIENTED_EDGE('',*,*,#16276,.F.);
#23129=ORIENTED_EDGE('',*,*,#16274,.T.);
#23130=ORIENTED_EDGE('',*,*,#16233,.F.);
#23131=ORIENTED_EDGE('',*,*,#16265,.F.);
#23132=ORIENTED_EDGE('',*,*,#16277,.F.);
#23133=ORIENTED_EDGE('',*,*,#16261,.T.);
#23134=ORIENTED_EDGE('',*,*,#16262,.T.);
#23135=ORIENTED_EDGE('',*,*,#16277,.T.);
#23136=ORIENTED_EDGE('',*,*,#16264,.T.);
#23137=ORIENTED_EDGE('',*,*,#16267,.T.);
#23138=ORIENTED_EDGE('',*,*,#16269,.T.);
#23139=ORIENTED_EDGE('',*,*,#16271,.T.);
#23140=ORIENTED_EDGE('',*,*,#16273,.T.);
#23141=ORIENTED_EDGE('',*,*,#16275,.T.);
#23142=ORIENTED_EDGE('',*,*,#16276,.T.);
#23143=ORIENTED_EDGE('',*,*,#16257,.T.);
#23144=ORIENTED_EDGE('',*,*,#16260,.T.);
#23145=ORIENTED_EDGE('',*,*,#16278,.T.);
#23146=ORIENTED_EDGE('',*,*,#16279,.T.);
#23147=ORIENTED_EDGE('',*,*,#16280,.T.);
#23148=ORIENTED_EDGE('',*,*,#16281,.T.);
#23149=ORIENTED_EDGE('',*,*,#16282,.T.);
#23150=ORIENTED_EDGE('',*,*,#16283,.T.);
#23151=ORIENTED_EDGE('',*,*,#16219,.F.);
#23152=ORIENTED_EDGE('',*,*,#16284,.F.);
#23153=ORIENTED_EDGE('',*,*,#16280,.F.);
#23154=ORIENTED_EDGE('',*,*,#16285,.T.);
#23155=ORIENTED_EDGE('',*,*,#16218,.F.);
#23156=ORIENTED_EDGE('',*,*,#16286,.F.);
#23157=ORIENTED_EDGE('',*,*,#16281,.F.);
#23158=ORIENTED_EDGE('',*,*,#16284,.T.);
#23159=ORIENTED_EDGE('',*,*,#16220,.F.);
#23160=ORIENTED_EDGE('',*,*,#16285,.F.);
#23161=ORIENTED_EDGE('',*,*,#16279,.F.);
#23162=ORIENTED_EDGE('',*,*,#16287,.T.);
#23163=ORIENTED_EDGE('',*,*,#16221,.F.);
#23164=ORIENTED_EDGE('',*,*,#16287,.F.);
#23165=ORIENTED_EDGE('',*,*,#16278,.F.);
#23166=ORIENTED_EDGE('',*,*,#16288,.T.);
#23167=ORIENTED_EDGE('',*,*,#16222,.F.);
#23168=ORIENTED_EDGE('',*,*,#16288,.F.);
#23169=ORIENTED_EDGE('',*,*,#16283,.F.);
#23170=ORIENTED_EDGE('',*,*,#16289,.T.);
#23171=ORIENTED_EDGE('',*,*,#16217,.F.);
#23172=ORIENTED_EDGE('',*,*,#16289,.F.);
#23173=ORIENTED_EDGE('',*,*,#16282,.F.);
#23174=ORIENTED_EDGE('',*,*,#16286,.T.);
#23175=ORIENTED_EDGE('',*,*,#16238,.F.);
#23176=ORIENTED_EDGE('',*,*,#16290,.F.);
#23177=ORIENTED_EDGE('',*,*,#16291,.F.);
#23178=ORIENTED_EDGE('',*,*,#16292,.T.);
#23179=ORIENTED_EDGE('',*,*,#16237,.F.);
#23180=ORIENTED_EDGE('',*,*,#16293,.F.);
#23181=ORIENTED_EDGE('',*,*,#16294,.F.);
#23182=ORIENTED_EDGE('',*,*,#16290,.T.);
#23183=ORIENTED_EDGE('',*,*,#16236,.F.);
#23184=ORIENTED_EDGE('',*,*,#16295,.F.);
#23185=ORIENTED_EDGE('',*,*,#16296,.F.);
#23186=ORIENTED_EDGE('',*,*,#16293,.T.);
#23187=ORIENTED_EDGE('',*,*,#16235,.F.);
#23188=ORIENTED_EDGE('',*,*,#16297,.F.);
#23189=ORIENTED_EDGE('',*,*,#16298,.F.);
#23190=ORIENTED_EDGE('',*,*,#16295,.T.);
#23191=ORIENTED_EDGE('',*,*,#16239,.F.);
#23192=ORIENTED_EDGE('',*,*,#16292,.F.);
#23193=ORIENTED_EDGE('',*,*,#16299,.F.);
#23194=ORIENTED_EDGE('',*,*,#16300,.T.);
#23195=ORIENTED_EDGE('',*,*,#16234,.F.);
#23196=ORIENTED_EDGE('',*,*,#16300,.F.);
#23197=ORIENTED_EDGE('',*,*,#16301,.F.);
#23198=ORIENTED_EDGE('',*,*,#16297,.T.);
#23199=ORIENTED_EDGE('',*,*,#16296,.T.);
#23200=ORIENTED_EDGE('',*,*,#16298,.T.);
#23201=ORIENTED_EDGE('',*,*,#16301,.T.);
#23202=ORIENTED_EDGE('',*,*,#16299,.T.);
#23203=ORIENTED_EDGE('',*,*,#16291,.T.);
#23204=ORIENTED_EDGE('',*,*,#16294,.T.);
#23205=ORIENTED_EDGE('',*,*,#16203,.F.);
#23206=ORIENTED_EDGE('',*,*,#16302,.F.);
#23207=ORIENTED_EDGE('',*,*,#16303,.F.);
#23208=ORIENTED_EDGE('',*,*,#16304,.T.);
#23209=ORIENTED_EDGE('',*,*,#16202,.F.);
#23210=ORIENTED_EDGE('',*,*,#16305,.F.);
#23211=ORIENTED_EDGE('',*,*,#16306,.F.);
#23212=ORIENTED_EDGE('',*,*,#16302,.T.);
#23213=ORIENTED_EDGE('',*,*,#16201,.F.);
#23214=ORIENTED_EDGE('',*,*,#16307,.F.);
#23215=ORIENTED_EDGE('',*,*,#16308,.F.);
#23216=ORIENTED_EDGE('',*,*,#16305,.T.);
#23217=ORIENTED_EDGE('',*,*,#16200,.F.);
#23218=ORIENTED_EDGE('',*,*,#16309,.F.);
#23219=ORIENTED_EDGE('',*,*,#16310,.F.);
#23220=ORIENTED_EDGE('',*,*,#16307,.T.);
#23221=ORIENTED_EDGE('',*,*,#16208,.F.);
#23222=ORIENTED_EDGE('',*,*,#16311,.F.);
#23223=ORIENTED_EDGE('',*,*,#16312,.F.);
#23224=ORIENTED_EDGE('',*,*,#16309,.T.);
#23225=ORIENTED_EDGE('',*,*,#16176,.F.);
#23226=ORIENTED_EDGE('',*,*,#16313,.F.);
#23227=ORIENTED_EDGE('',*,*,#16314,.F.);
#23228=ORIENTED_EDGE('',*,*,#16315,.T.);
#23229=ORIENTED_EDGE('',*,*,#16175,.F.);
#23230=ORIENTED_EDGE('',*,*,#16316,.F.);
#23231=ORIENTED_EDGE('',*,*,#16317,.F.);
#23232=ORIENTED_EDGE('',*,*,#16313,.T.);
#23233=ORIENTED_EDGE('',*,*,#16207,.F.);
#23234=ORIENTED_EDGE('',*,*,#16318,.F.);
#23235=ORIENTED_EDGE('',*,*,#16319,.F.);
#23236=ORIENTED_EDGE('',*,*,#16311,.T.);
#23237=ORIENTED_EDGE('',*,*,#16206,.F.);
#23238=ORIENTED_EDGE('',*,*,#16320,.F.);
#23239=ORIENTED_EDGE('',*,*,#16321,.F.);
#23240=ORIENTED_EDGE('',*,*,#16318,.T.);
#23241=ORIENTED_EDGE('',*,*,#16205,.F.);
#23242=ORIENTED_EDGE('',*,*,#16322,.F.);
#23243=ORIENTED_EDGE('',*,*,#16323,.F.);
#23244=ORIENTED_EDGE('',*,*,#16320,.T.);
#23245=ORIENTED_EDGE('',*,*,#16204,.F.);
#23246=ORIENTED_EDGE('',*,*,#16304,.F.);
#23247=ORIENTED_EDGE('',*,*,#16324,.F.);
#23248=ORIENTED_EDGE('',*,*,#16322,.T.);
#23249=ORIENTED_EDGE('',*,*,#16174,.F.);
#23250=ORIENTED_EDGE('',*,*,#16325,.F.);
#23251=ORIENTED_EDGE('',*,*,#16326,.F.);
#23252=ORIENTED_EDGE('',*,*,#16316,.T.);
#23253=ORIENTED_EDGE('',*,*,#16173,.F.);
#23254=ORIENTED_EDGE('',*,*,#16315,.F.);
#23255=ORIENTED_EDGE('',*,*,#16327,.F.);
#23256=ORIENTED_EDGE('',*,*,#16325,.T.);
#23257=ORIENTED_EDGE('',*,*,#16310,.T.);
#23258=ORIENTED_EDGE('',*,*,#16312,.T.);
#23259=ORIENTED_EDGE('',*,*,#16319,.T.);
#23260=ORIENTED_EDGE('',*,*,#16321,.T.);
#23261=ORIENTED_EDGE('',*,*,#16323,.T.);
#23262=ORIENTED_EDGE('',*,*,#16324,.T.);
#23263=ORIENTED_EDGE('',*,*,#16303,.T.);
#23264=ORIENTED_EDGE('',*,*,#16306,.T.);
#23265=ORIENTED_EDGE('',*,*,#16308,.T.);
#23266=ORIENTED_EDGE('',*,*,#16317,.T.);
#23267=ORIENTED_EDGE('',*,*,#16326,.T.);
#23268=ORIENTED_EDGE('',*,*,#16327,.T.);
#23269=ORIENTED_EDGE('',*,*,#16314,.T.);
#23270=ORIENTED_EDGE('',*,*,#16328,.F.);
#23271=ORIENTED_EDGE('',*,*,#16329,.T.);
#23272=ORIENTED_EDGE('',*,*,#16330,.T.);
#23273=ORIENTED_EDGE('',*,*,#16329,.F.);
#23274=ORIENTED_EDGE('',*,*,#16331,.T.);
#23275=ORIENTED_EDGE('',*,*,#16328,.T.);
#23276=ORIENTED_EDGE('',*,*,#16331,.F.);
#23277=ORIENTED_EDGE('',*,*,#16332,.F.);
#23278=ORIENTED_EDGE('',*,*,#16333,.T.);
#23279=ORIENTED_EDGE('',*,*,#16334,.T.);
#23280=ORIENTED_EDGE('',*,*,#16333,.F.);
#23281=ORIENTED_EDGE('',*,*,#16335,.T.);
#23282=ORIENTED_EDGE('',*,*,#16332,.T.);
#23283=ORIENTED_EDGE('',*,*,#16335,.F.);
#23284=ORIENTED_EDGE('',*,*,#16336,.F.);
#23285=ORIENTED_EDGE('',*,*,#16337,.T.);
#23286=ORIENTED_EDGE('',*,*,#16338,.T.);
#23287=ORIENTED_EDGE('',*,*,#16337,.F.);
#23288=ORIENTED_EDGE('',*,*,#16339,.T.);
#23289=ORIENTED_EDGE('',*,*,#16336,.T.);
#23290=ORIENTED_EDGE('',*,*,#16339,.F.);
#23291=ORIENTED_EDGE('',*,*,#16340,.F.);
#23292=ORIENTED_EDGE('',*,*,#16341,.T.);
#23293=ORIENTED_EDGE('',*,*,#16342,.T.);
#23294=ORIENTED_EDGE('',*,*,#16341,.F.);
#23295=ORIENTED_EDGE('',*,*,#16343,.T.);
#23296=ORIENTED_EDGE('',*,*,#16340,.T.);
#23297=ORIENTED_EDGE('',*,*,#16343,.F.);
#23298=ORIENTED_EDGE('',*,*,#16344,.F.);
#23299=ORIENTED_EDGE('',*,*,#16345,.T.);
#23300=ORIENTED_EDGE('',*,*,#16346,.T.);
#23301=ORIENTED_EDGE('',*,*,#16345,.F.);
#23302=ORIENTED_EDGE('',*,*,#16347,.T.);
#23303=ORIENTED_EDGE('',*,*,#16344,.T.);
#23304=ORIENTED_EDGE('',*,*,#16347,.F.);
#23305=ORIENTED_EDGE('',*,*,#16348,.F.);
#23306=ORIENTED_EDGE('',*,*,#16349,.T.);
#23307=ORIENTED_EDGE('',*,*,#16350,.T.);
#23308=ORIENTED_EDGE('',*,*,#16349,.F.);
#23309=ORIENTED_EDGE('',*,*,#16351,.T.);
#23310=ORIENTED_EDGE('',*,*,#16348,.T.);
#23311=ORIENTED_EDGE('',*,*,#16351,.F.);
#23312=ORIENTED_EDGE('',*,*,#16352,.F.);
#23313=ORIENTED_EDGE('',*,*,#16353,.T.);
#23314=ORIENTED_EDGE('',*,*,#16354,.T.);
#23315=ORIENTED_EDGE('',*,*,#16353,.F.);
#23316=ORIENTED_EDGE('',*,*,#16355,.T.);
#23317=ORIENTED_EDGE('',*,*,#16352,.T.);
#23318=ORIENTED_EDGE('',*,*,#16355,.F.);
#23319=ORIENTED_EDGE('',*,*,#16356,.F.);
#23320=ORIENTED_EDGE('',*,*,#16357,.T.);
#23321=ORIENTED_EDGE('',*,*,#16358,.T.);
#23322=ORIENTED_EDGE('',*,*,#16357,.F.);
#23323=ORIENTED_EDGE('',*,*,#16359,.T.);
#23324=ORIENTED_EDGE('',*,*,#16356,.T.);
#23325=ORIENTED_EDGE('',*,*,#16359,.F.);
#23326=ORIENTED_EDGE('',*,*,#16360,.F.);
#23327=ORIENTED_EDGE('',*,*,#16361,.T.);
#23328=ORIENTED_EDGE('',*,*,#16362,.T.);
#23329=ORIENTED_EDGE('',*,*,#16361,.F.);
#23330=ORIENTED_EDGE('',*,*,#16363,.T.);
#23331=ORIENTED_EDGE('',*,*,#16360,.T.);
#23332=ORIENTED_EDGE('',*,*,#16363,.F.);
#23333=ORIENTED_EDGE('',*,*,#16364,.F.);
#23334=ORIENTED_EDGE('',*,*,#16365,.T.);
#23335=ORIENTED_EDGE('',*,*,#16366,.T.);
#23336=ORIENTED_EDGE('',*,*,#16365,.F.);
#23337=ORIENTED_EDGE('',*,*,#16367,.T.);
#23338=ORIENTED_EDGE('',*,*,#16364,.T.);
#23339=ORIENTED_EDGE('',*,*,#16367,.F.);
#23340=ORIENTED_EDGE('',*,*,#16368,.F.);
#23341=ORIENTED_EDGE('',*,*,#16369,.T.);
#23342=ORIENTED_EDGE('',*,*,#16370,.T.);
#23343=ORIENTED_EDGE('',*,*,#16369,.F.);
#23344=ORIENTED_EDGE('',*,*,#16371,.T.);
#23345=ORIENTED_EDGE('',*,*,#16368,.T.);
#23346=ORIENTED_EDGE('',*,*,#16371,.F.);
#23347=ORIENTED_EDGE('',*,*,#16372,.F.);
#23348=ORIENTED_EDGE('',*,*,#16373,.T.);
#23349=ORIENTED_EDGE('',*,*,#16374,.T.);
#23350=ORIENTED_EDGE('',*,*,#16373,.F.);
#23351=ORIENTED_EDGE('',*,*,#16375,.T.);
#23352=ORIENTED_EDGE('',*,*,#16372,.T.);
#23353=ORIENTED_EDGE('',*,*,#16375,.F.);
#23354=ORIENTED_EDGE('',*,*,#16376,.F.);
#23355=ORIENTED_EDGE('',*,*,#16377,.T.);
#23356=ORIENTED_EDGE('',*,*,#16378,.T.);
#23357=ORIENTED_EDGE('',*,*,#16377,.F.);
#23358=ORIENTED_EDGE('',*,*,#16379,.T.);
#23359=ORIENTED_EDGE('',*,*,#16376,.T.);
#23360=ORIENTED_EDGE('',*,*,#16379,.F.);
#23361=ORIENTED_EDGE('',*,*,#16380,.F.);
#23362=ORIENTED_EDGE('',*,*,#16381,.T.);
#23363=ORIENTED_EDGE('',*,*,#16382,.T.);
#23364=ORIENTED_EDGE('',*,*,#16381,.F.);
#23365=ORIENTED_EDGE('',*,*,#16383,.T.);
#23366=ORIENTED_EDGE('',*,*,#16380,.T.);
#23367=ORIENTED_EDGE('',*,*,#16383,.F.);
#23368=ORIENTED_EDGE('',*,*,#16384,.F.);
#23369=ORIENTED_EDGE('',*,*,#16385,.T.);
#23370=ORIENTED_EDGE('',*,*,#16386,.T.);
#23371=ORIENTED_EDGE('',*,*,#16385,.F.);
#23372=ORIENTED_EDGE('',*,*,#16387,.T.);
#23373=ORIENTED_EDGE('',*,*,#16384,.T.);
#23374=ORIENTED_EDGE('',*,*,#16387,.F.);
#23375=ORIENTED_EDGE('',*,*,#16388,.F.);
#23376=ORIENTED_EDGE('',*,*,#16389,.T.);
#23377=ORIENTED_EDGE('',*,*,#16390,.T.);
#23378=ORIENTED_EDGE('',*,*,#16389,.F.);
#23379=ORIENTED_EDGE('',*,*,#16391,.T.);
#23380=ORIENTED_EDGE('',*,*,#16388,.T.);
#23381=ORIENTED_EDGE('',*,*,#16391,.F.);
#23382=ORIENTED_EDGE('',*,*,#16392,.F.);
#23383=ORIENTED_EDGE('',*,*,#16393,.T.);
#23384=ORIENTED_EDGE('',*,*,#16394,.T.);
#23385=ORIENTED_EDGE('',*,*,#16393,.F.);
#23386=ORIENTED_EDGE('',*,*,#16395,.T.);
#23387=ORIENTED_EDGE('',*,*,#16392,.T.);
#23388=ORIENTED_EDGE('',*,*,#16395,.F.);
#23389=ORIENTED_EDGE('',*,*,#16396,.T.);
#23390=ORIENTED_EDGE('',*,*,#16397,.T.);
#23391=ORIENTED_EDGE('',*,*,#16398,.F.);
#23392=ORIENTED_EDGE('',*,*,#16399,.F.);
#23393=ORIENTED_EDGE('',*,*,#16398,.T.);
#23394=ORIENTED_EDGE('',*,*,#16400,.F.);
#23395=ORIENTED_EDGE('',*,*,#16401,.T.);
#23396=ORIENTED_EDGE('',*,*,#16402,.F.);
#23397=ORIENTED_EDGE('',*,*,#16403,.T.);
#23398=ORIENTED_EDGE('',*,*,#16404,.F.);
#23399=ORIENTED_EDGE('',*,*,#16405,.T.);
#23400=ORIENTED_EDGE('',*,*,#16406,.T.);
#23401=ORIENTED_EDGE('',*,*,#16407,.F.);
#23402=ORIENTED_EDGE('',*,*,#16408,.F.);
#23403=ORIENTED_EDGE('',*,*,#16409,.T.);
#23404=ORIENTED_EDGE('',*,*,#16410,.F.);
#23405=ORIENTED_EDGE('',*,*,#16411,.F.);
#23406=ORIENTED_EDGE('',*,*,#16407,.T.);
#23407=ORIENTED_EDGE('',*,*,#16412,.T.);
#23408=ORIENTED_EDGE('',*,*,#16413,.T.);
#23409=ORIENTED_EDGE('',*,*,#16414,.T.);
#23410=ORIENTED_EDGE('',*,*,#16415,.T.);
#23411=ORIENTED_EDGE('',*,*,#16416,.T.);
#23412=ORIENTED_EDGE('',*,*,#16396,.F.);
#23413=ORIENTED_EDGE('',*,*,#16417,.F.);
#23414=ORIENTED_EDGE('',*,*,#16410,.T.);
#23415=ORIENTED_EDGE('',*,*,#16418,.T.);
#23416=ORIENTED_EDGE('',*,*,#16419,.F.);
#23417=ORIENTED_EDGE('',*,*,#16405,.F.);
#23418=ORIENTED_EDGE('',*,*,#16420,.F.);
#23419=ORIENTED_EDGE('',*,*,#16419,.T.);
#23420=ORIENTED_EDGE('',*,*,#16421,.T.);
#23421=ORIENTED_EDGE('',*,*,#16408,.T.);
#23422=ORIENTED_EDGE('',*,*,#16411,.T.);
#23423=ORIENTED_EDGE('',*,*,#16417,.T.);
#23424=ORIENTED_EDGE('',*,*,#16399,.T.);
#23425=ORIENTED_EDGE('',*,*,#16406,.F.);
#23426=ORIENTED_EDGE('',*,*,#16421,.F.);
#23427=ORIENTED_EDGE('',*,*,#16418,.F.);
#23428=ORIENTED_EDGE('',*,*,#16409,.F.);
#23429=ORIENTED_EDGE('',*,*,#16416,.F.);
#23430=ORIENTED_EDGE('',*,*,#16422,.T.);
#23431=ORIENTED_EDGE('',*,*,#16400,.T.);
#23432=ORIENTED_EDGE('',*,*,#16397,.F.);
#23433=ORIENTED_EDGE('',*,*,#16414,.F.);
#23434=ORIENTED_EDGE('',*,*,#16423,.T.);
#23435=ORIENTED_EDGE('',*,*,#16402,.T.);
#23436=ORIENTED_EDGE('',*,*,#16424,.T.);
#23437=ORIENTED_EDGE('',*,*,#16330,.F.);
#23438=ORIENTED_EDGE('',*,*,#16334,.F.);
#23439=ORIENTED_EDGE('',*,*,#16338,.F.);
#23440=ORIENTED_EDGE('',*,*,#16342,.F.);
#23441=ORIENTED_EDGE('',*,*,#16346,.F.);
#23442=ORIENTED_EDGE('',*,*,#16350,.F.);
#23443=ORIENTED_EDGE('',*,*,#16354,.F.);
#23444=ORIENTED_EDGE('',*,*,#16358,.F.);
#23445=ORIENTED_EDGE('',*,*,#16362,.F.);
#23446=ORIENTED_EDGE('',*,*,#16366,.F.);
#23447=ORIENTED_EDGE('',*,*,#16370,.F.);
#23448=ORIENTED_EDGE('',*,*,#16374,.F.);
#23449=ORIENTED_EDGE('',*,*,#16378,.F.);
#23450=ORIENTED_EDGE('',*,*,#16382,.F.);
#23451=ORIENTED_EDGE('',*,*,#16386,.F.);
#23452=ORIENTED_EDGE('',*,*,#16390,.F.);
#23453=ORIENTED_EDGE('',*,*,#16394,.F.);
#23454=ORIENTED_EDGE('',*,*,#16404,.T.);
#23455=ORIENTED_EDGE('',*,*,#16425,.T.);
#23456=ORIENTED_EDGE('',*,*,#16412,.F.);
#23457=ORIENTED_EDGE('',*,*,#16420,.T.);
#23458=ORIENTED_EDGE('',*,*,#16413,.F.);
#23459=ORIENTED_EDGE('',*,*,#16425,.F.);
#23460=ORIENTED_EDGE('',*,*,#16403,.F.);
#23461=ORIENTED_EDGE('',*,*,#16423,.F.);
#23462=ORIENTED_EDGE('',*,*,#16415,.F.);
#23463=ORIENTED_EDGE('',*,*,#16424,.F.);
#23464=ORIENTED_EDGE('',*,*,#16401,.F.);
#23465=ORIENTED_EDGE('',*,*,#16422,.F.);
#23466=ORIENTED_EDGE('',*,*,#16426,.F.);
#23467=ORIENTED_EDGE('',*,*,#16427,.T.);
#23468=ORIENTED_EDGE('',*,*,#16428,.T.);
#23469=ORIENTED_EDGE('',*,*,#16427,.F.);
#23470=ORIENTED_EDGE('',*,*,#16428,.F.);
#23471=ORIENTED_EDGE('',*,*,#16429,.T.);
#23472=ORIENTED_EDGE('',*,*,#16430,.T.);
#23473=ORIENTED_EDGE('',*,*,#16429,.F.);
#23474=ORIENTED_EDGE('',*,*,#16431,.T.);
#23475=ORIENTED_EDGE('',*,*,#16432,.T.);
#23476=ORIENTED_EDGE('',*,*,#16433,.F.);
#23477=ORIENTED_EDGE('',*,*,#16432,.F.);
#23478=ORIENTED_EDGE('',*,*,#16434,.T.);
#23479=ORIENTED_EDGE('',*,*,#16431,.F.);
#23480=ORIENTED_EDGE('',*,*,#16435,.T.);
#23481=ORIENTED_EDGE('',*,*,#16436,.T.);
#23482=ORIENTED_EDGE('',*,*,#16435,.F.);
#23483=ORIENTED_EDGE('',*,*,#16434,.F.);
#23484=ORIENTED_EDGE('',*,*,#16433,.T.);
#23485=ORIENTED_EDGE('',*,*,#16430,.F.);
#23486=ORIENTED_EDGE('',*,*,#16437,.F.);
#23487=ORIENTED_EDGE('',*,*,#16438,.F.);
#23488=ORIENTED_EDGE('',*,*,#16439,.F.);
#23489=ORIENTED_EDGE('',*,*,#16440,.F.);
#23490=ORIENTED_EDGE('',*,*,#16441,.F.);
#23491=ORIENTED_EDGE('',*,*,#16442,.F.);
#23492=ORIENTED_EDGE('',*,*,#16426,.T.);
#23493=ORIENTED_EDGE('',*,*,#16436,.F.);
#23494=ORIENTED_EDGE('',*,*,#16437,.T.);
#23495=ORIENTED_EDGE('',*,*,#16443,.F.);
#23496=ORIENTED_EDGE('',*,*,#16444,.F.);
#23497=ORIENTED_EDGE('',*,*,#16445,.T.);
#23498=ORIENTED_EDGE('',*,*,#16438,.T.);
#23499=ORIENTED_EDGE('',*,*,#16445,.F.);
#23500=ORIENTED_EDGE('',*,*,#16446,.F.);
#23501=ORIENTED_EDGE('',*,*,#16447,.T.);
#23502=ORIENTED_EDGE('',*,*,#16439,.T.);
#23503=ORIENTED_EDGE('',*,*,#16447,.F.);
#23504=ORIENTED_EDGE('',*,*,#16448,.F.);
#23505=ORIENTED_EDGE('',*,*,#16449,.T.);
#23506=ORIENTED_EDGE('',*,*,#16440,.T.);
#23507=ORIENTED_EDGE('',*,*,#16449,.F.);
#23508=ORIENTED_EDGE('',*,*,#16450,.F.);
#23509=ORIENTED_EDGE('',*,*,#16451,.T.);
#23510=ORIENTED_EDGE('',*,*,#16441,.T.);
#23511=ORIENTED_EDGE('',*,*,#16451,.F.);
#23512=ORIENTED_EDGE('',*,*,#16452,.F.);
#23513=ORIENTED_EDGE('',*,*,#16453,.T.);
#23514=ORIENTED_EDGE('',*,*,#16442,.T.);
#23515=ORIENTED_EDGE('',*,*,#16453,.F.);
#23516=ORIENTED_EDGE('',*,*,#16454,.F.);
#23517=ORIENTED_EDGE('',*,*,#16443,.T.);
#23518=ORIENTED_EDGE('',*,*,#16444,.T.);
#23519=ORIENTED_EDGE('',*,*,#16454,.T.);
#23520=ORIENTED_EDGE('',*,*,#16452,.T.);
#23521=ORIENTED_EDGE('',*,*,#16450,.T.);
#23522=ORIENTED_EDGE('',*,*,#16448,.T.);
#23523=ORIENTED_EDGE('',*,*,#16446,.T.);
#23524=ORIENTED_EDGE('',*,*,#16455,.F.);
#23525=ORIENTED_EDGE('',*,*,#16456,.F.);
#23526=ORIENTED_EDGE('',*,*,#16457,.T.);
#23527=ORIENTED_EDGE('',*,*,#16458,.F.);
#23528=ORIENTED_EDGE('',*,*,#16457,.F.);
#23529=ORIENTED_EDGE('',*,*,#16459,.T.);
#23530=ORIENTED_EDGE('',*,*,#16460,.T.);
#23531=ORIENTED_EDGE('',*,*,#16461,.T.);
#23532=ORIENTED_EDGE('',*,*,#16462,.T.);
#23533=ORIENTED_EDGE('',*,*,#16463,.T.);
#23534=ORIENTED_EDGE('',*,*,#16464,.T.);
#23535=ORIENTED_EDGE('',*,*,#16465,.T.);
#23536=ORIENTED_EDGE('',*,*,#16466,.T.);
#23537=ORIENTED_EDGE('',*,*,#16459,.F.);
#23538=ORIENTED_EDGE('',*,*,#16455,.T.);
#23539=ORIENTED_EDGE('',*,*,#16456,.T.);
#23540=ORIENTED_EDGE('',*,*,#16467,.T.);
#23541=ORIENTED_EDGE('',*,*,#16468,.T.);
#23542=ORIENTED_EDGE('',*,*,#16467,.F.);
#23543=ORIENTED_EDGE('',*,*,#16469,.F.);
#23544=ORIENTED_EDGE('',*,*,#16470,.T.);
#23545=ORIENTED_EDGE('',*,*,#16471,.T.);
#23546=ORIENTED_EDGE('',*,*,#16470,.F.);
#23547=ORIENTED_EDGE('',*,*,#16472,.F.);
#23548=ORIENTED_EDGE('',*,*,#16473,.T.);
#23549=ORIENTED_EDGE('',*,*,#16474,.T.);
#23550=ORIENTED_EDGE('',*,*,#16473,.F.);
#23551=ORIENTED_EDGE('',*,*,#16458,.T.);
#23552=ORIENTED_EDGE('',*,*,#16475,.F.);
#23553=ORIENTED_EDGE('',*,*,#16476,.F.);
#23554=ORIENTED_EDGE('',*,*,#16477,.F.);
#23555=ORIENTED_EDGE('',*,*,#16478,.F.);
#23556=ORIENTED_EDGE('',*,*,#16479,.F.);
#23557=ORIENTED_EDGE('',*,*,#16480,.F.);
#23558=ORIENTED_EDGE('',*,*,#16474,.F.);
#23559=ORIENTED_EDGE('',*,*,#16472,.T.);
#23560=ORIENTED_EDGE('',*,*,#16471,.F.);
#23561=ORIENTED_EDGE('',*,*,#16468,.F.);
#23562=ORIENTED_EDGE('',*,*,#16469,.T.);
#23563=ORIENTED_EDGE('',*,*,#16481,.F.);
#23564=ORIENTED_EDGE('',*,*,#16482,.T.);
#23565=ORIENTED_EDGE('',*,*,#16476,.T.);
#23566=ORIENTED_EDGE('',*,*,#16483,.F.);
#23567=ORIENTED_EDGE('',*,*,#16484,.F.);
#23568=ORIENTED_EDGE('',*,*,#16485,.F.);
#23569=ORIENTED_EDGE('',*,*,#16486,.T.);
#23570=ORIENTED_EDGE('',*,*,#16477,.T.);
#23571=ORIENTED_EDGE('',*,*,#16482,.F.);
#23572=ORIENTED_EDGE('',*,*,#16487,.F.);
#23573=ORIENTED_EDGE('',*,*,#16488,.F.);
#23574=ORIENTED_EDGE('',*,*,#16489,.T.);
#23575=ORIENTED_EDGE('',*,*,#16478,.T.);
#23576=ORIENTED_EDGE('',*,*,#16486,.F.);
#23577=ORIENTED_EDGE('',*,*,#16490,.F.);
#23578=ORIENTED_EDGE('',*,*,#16491,.F.);
#23579=ORIENTED_EDGE('',*,*,#16492,.T.);
#23580=ORIENTED_EDGE('',*,*,#16479,.T.);
#23581=ORIENTED_EDGE('',*,*,#16489,.F.);
#23582=ORIENTED_EDGE('',*,*,#16493,.F.);
#23583=ORIENTED_EDGE('',*,*,#16494,.F.);
#23584=ORIENTED_EDGE('',*,*,#16495,.T.);
#23585=ORIENTED_EDGE('',*,*,#16480,.T.);
#23586=ORIENTED_EDGE('',*,*,#16492,.F.);
#23587=ORIENTED_EDGE('',*,*,#16496,.F.);
#23588=ORIENTED_EDGE('',*,*,#16497,.F.);
#23589=ORIENTED_EDGE('',*,*,#16483,.T.);
#23590=ORIENTED_EDGE('',*,*,#16475,.T.);
#23591=ORIENTED_EDGE('',*,*,#16495,.F.);
#23592=ORIENTED_EDGE('',*,*,#16498,.F.);
#23593=ORIENTED_EDGE('',*,*,#16484,.T.);
#23594=ORIENTED_EDGE('',*,*,#16497,.T.);
#23595=ORIENTED_EDGE('',*,*,#16465,.F.);
#23596=ORIENTED_EDGE('',*,*,#16498,.T.);
#23597=ORIENTED_EDGE('',*,*,#16494,.T.);
#23598=ORIENTED_EDGE('',*,*,#16460,.F.);
#23599=ORIENTED_EDGE('',*,*,#16466,.F.);
#23600=ORIENTED_EDGE('',*,*,#16496,.T.);
#23601=ORIENTED_EDGE('',*,*,#16491,.T.);
#23602=ORIENTED_EDGE('',*,*,#16461,.F.);
#23603=ORIENTED_EDGE('',*,*,#16493,.T.);
#23604=ORIENTED_EDGE('',*,*,#16488,.T.);
#23605=ORIENTED_EDGE('',*,*,#16462,.F.);
#23606=ORIENTED_EDGE('',*,*,#16490,.T.);
#23607=ORIENTED_EDGE('',*,*,#16485,.T.);
#23608=ORIENTED_EDGE('',*,*,#16463,.F.);
#23609=ORIENTED_EDGE('',*,*,#16487,.T.);
#23610=ORIENTED_EDGE('',*,*,#16481,.T.);
#23611=ORIENTED_EDGE('',*,*,#16464,.F.);
#23612=ORIENTED_EDGE('',*,*,#16499,.F.);
#23613=ORIENTED_EDGE('',*,*,#16500,.T.);
#23614=ORIENTED_EDGE('',*,*,#16501,.T.);
#23615=ORIENTED_EDGE('',*,*,#16500,.F.);
#23616=ORIENTED_EDGE('',*,*,#16502,.F.);
#23617=ORIENTED_EDGE('',*,*,#16503,.T.);
#23618=ORIENTED_EDGE('',*,*,#16504,.T.);
#23619=ORIENTED_EDGE('',*,*,#16503,.F.);
#23620=ORIENTED_EDGE('',*,*,#16499,.T.);
#23621=ORIENTED_EDGE('',*,*,#16504,.F.);
#23622=ORIENTED_EDGE('',*,*,#16501,.F.);
#23623=ORIENTED_EDGE('',*,*,#16502,.T.);
#23624=ORIENTED_EDGE('',*,*,#16505,.T.);
#23625=ORIENTED_EDGE('',*,*,#16506,.F.);
#23626=ORIENTED_EDGE('',*,*,#16507,.F.);
#23627=ORIENTED_EDGE('',*,*,#16508,.T.);
#23628=ORIENTED_EDGE('',*,*,#16509,.F.);
#23629=ORIENTED_EDGE('',*,*,#16510,.F.);
#23630=ORIENTED_EDGE('',*,*,#16511,.T.);
#23631=ORIENTED_EDGE('',*,*,#16512,.T.);
#23632=ORIENTED_EDGE('',*,*,#16507,.T.);
#23633=ORIENTED_EDGE('',*,*,#16513,.T.);
#23634=ORIENTED_EDGE('',*,*,#16511,.F.);
#23635=ORIENTED_EDGE('',*,*,#16514,.T.);
#23636=ORIENTED_EDGE('',*,*,#16509,.T.);
#23637=ORIENTED_EDGE('',*,*,#16515,.F.);
#23638=ORIENTED_EDGE('',*,*,#16505,.F.);
#23639=ORIENTED_EDGE('',*,*,#16516,.F.);
#23640=ORIENTED_EDGE('',*,*,#16516,.T.);
#23641=ORIENTED_EDGE('',*,*,#16508,.F.);
#23642=ORIENTED_EDGE('',*,*,#16514,.F.);
#23643=ORIENTED_EDGE('',*,*,#16510,.T.);
#23644=ORIENTED_EDGE('',*,*,#16515,.T.);
#23645=ORIENTED_EDGE('',*,*,#16512,.F.);
#23646=ORIENTED_EDGE('',*,*,#16513,.F.);
#23647=ORIENTED_EDGE('',*,*,#16506,.T.);
#23648=ORIENTED_EDGE('',*,*,#16517,.F.);
#23649=ORIENTED_EDGE('',*,*,#16518,.T.);
#23650=ORIENTED_EDGE('',*,*,#16519,.T.);
#23651=ORIENTED_EDGE('',*,*,#16518,.F.);
#23652=ORIENTED_EDGE('',*,*,#16520,.F.);
#23653=ORIENTED_EDGE('',*,*,#16521,.T.);
#23654=ORIENTED_EDGE('',*,*,#16522,.T.);
#23655=ORIENTED_EDGE('',*,*,#16521,.F.);
#23656=ORIENTED_EDGE('',*,*,#16523,.F.);
#23657=ORIENTED_EDGE('',*,*,#16524,.T.);
#23658=ORIENTED_EDGE('',*,*,#16525,.T.);
#23659=ORIENTED_EDGE('',*,*,#16524,.F.);
#23660=ORIENTED_EDGE('',*,*,#16526,.F.);
#23661=ORIENTED_EDGE('',*,*,#16527,.T.);
#23662=ORIENTED_EDGE('',*,*,#16528,.T.);
#23663=ORIENTED_EDGE('',*,*,#16527,.F.);
#23664=ORIENTED_EDGE('',*,*,#16529,.F.);
#23665=ORIENTED_EDGE('',*,*,#16530,.T.);
#23666=ORIENTED_EDGE('',*,*,#16531,.T.);
#23667=ORIENTED_EDGE('',*,*,#16530,.F.);
#23668=ORIENTED_EDGE('',*,*,#16532,.F.);
#23669=ORIENTED_EDGE('',*,*,#16533,.T.);
#23670=ORIENTED_EDGE('',*,*,#16534,.T.);
#23671=ORIENTED_EDGE('',*,*,#16533,.F.);
#23672=ORIENTED_EDGE('',*,*,#16535,.F.);
#23673=ORIENTED_EDGE('',*,*,#16536,.T.);
#23674=ORIENTED_EDGE('',*,*,#16537,.T.);
#23675=ORIENTED_EDGE('',*,*,#16536,.F.);
#23676=ORIENTED_EDGE('',*,*,#16538,.F.);
#23677=ORIENTED_EDGE('',*,*,#16539,.T.);
#23678=ORIENTED_EDGE('',*,*,#16540,.T.);
#23679=ORIENTED_EDGE('',*,*,#16539,.F.);
#23680=ORIENTED_EDGE('',*,*,#16541,.F.);
#23681=ORIENTED_EDGE('',*,*,#16542,.T.);
#23682=ORIENTED_EDGE('',*,*,#16543,.T.);
#23683=ORIENTED_EDGE('',*,*,#16542,.F.);
#23684=ORIENTED_EDGE('',*,*,#16544,.F.);
#23685=ORIENTED_EDGE('',*,*,#16545,.T.);
#23686=ORIENTED_EDGE('',*,*,#16546,.T.);
#23687=ORIENTED_EDGE('',*,*,#16545,.F.);
#23688=ORIENTED_EDGE('',*,*,#16547,.F.);
#23689=ORIENTED_EDGE('',*,*,#16548,.F.);
#23690=ORIENTED_EDGE('',*,*,#16549,.F.);
#23691=ORIENTED_EDGE('',*,*,#16550,.F.);
#23692=ORIENTED_EDGE('',*,*,#16517,.T.);
#23693=ORIENTED_EDGE('',*,*,#16520,.T.);
#23694=ORIENTED_EDGE('',*,*,#16523,.T.);
#23695=ORIENTED_EDGE('',*,*,#16526,.T.);
#23696=ORIENTED_EDGE('',*,*,#16529,.T.);
#23697=ORIENTED_EDGE('',*,*,#16532,.T.);
#23698=ORIENTED_EDGE('',*,*,#16535,.T.);
#23699=ORIENTED_EDGE('',*,*,#16538,.T.);
#23700=ORIENTED_EDGE('',*,*,#16541,.T.);
#23701=ORIENTED_EDGE('',*,*,#16544,.T.);
#23702=ORIENTED_EDGE('',*,*,#16549,.T.);
#23703=ORIENTED_EDGE('',*,*,#16551,.F.);
#23704=ORIENTED_EDGE('',*,*,#16552,.F.);
#23705=ORIENTED_EDGE('',*,*,#16553,.T.);
#23706=ORIENTED_EDGE('',*,*,#16548,.T.);
#23707=ORIENTED_EDGE('',*,*,#16554,.T.);
#23708=ORIENTED_EDGE('',*,*,#16555,.T.);
#23709=ORIENTED_EDGE('',*,*,#16556,.F.);
#23710=ORIENTED_EDGE('',*,*,#16557,.F.);
#23711=ORIENTED_EDGE('',*,*,#16551,.T.);
#23712=ORIENTED_EDGE('',*,*,#16556,.T.);
#23713=ORIENTED_EDGE('',*,*,#16558,.T.);
#23714=ORIENTED_EDGE('',*,*,#16559,.F.);
#23715=ORIENTED_EDGE('',*,*,#16560,.F.);
#23716=ORIENTED_EDGE('',*,*,#16559,.T.);
#23717=ORIENTED_EDGE('',*,*,#16561,.T.);
#23718=ORIENTED_EDGE('',*,*,#16562,.T.);
#23719=ORIENTED_EDGE('',*,*,#16550,.T.);
#23720=ORIENTED_EDGE('',*,*,#16553,.F.);
#23721=ORIENTED_EDGE('',*,*,#16563,.F.);
#23722=ORIENTED_EDGE('',*,*,#16552,.T.);
#23723=ORIENTED_EDGE('',*,*,#16557,.T.);
#23724=ORIENTED_EDGE('',*,*,#16560,.T.);
#23725=ORIENTED_EDGE('',*,*,#16563,.T.);
#23726=ORIENTED_EDGE('',*,*,#16519,.F.);
#23727=ORIENTED_EDGE('',*,*,#16522,.F.);
#23728=ORIENTED_EDGE('',*,*,#16525,.F.);
#23729=ORIENTED_EDGE('',*,*,#16528,.F.);
#23730=ORIENTED_EDGE('',*,*,#16531,.F.);
#23731=ORIENTED_EDGE('',*,*,#16534,.F.);
#23732=ORIENTED_EDGE('',*,*,#16537,.F.);
#23733=ORIENTED_EDGE('',*,*,#16540,.F.);
#23734=ORIENTED_EDGE('',*,*,#16543,.F.);
#23735=ORIENTED_EDGE('',*,*,#16546,.F.);
#23736=ORIENTED_EDGE('',*,*,#16554,.F.);
#23737=ORIENTED_EDGE('',*,*,#16547,.T.);
#23738=ORIENTED_EDGE('',*,*,#16562,.F.);
#23739=ORIENTED_EDGE('',*,*,#16564,.F.);
#23740=ORIENTED_EDGE('',*,*,#16555,.F.);
#23741=ORIENTED_EDGE('',*,*,#16564,.T.);
#23742=ORIENTED_EDGE('',*,*,#16561,.F.);
#23743=ORIENTED_EDGE('',*,*,#16558,.F.);
#23744=ORIENTED_EDGE('',*,*,#16565,.F.);
#23745=ORIENTED_EDGE('',*,*,#16566,.T.);
#23746=ORIENTED_EDGE('',*,*,#16567,.T.);
#23747=ORIENTED_EDGE('',*,*,#16566,.F.);
#23748=ORIENTED_EDGE('',*,*,#16567,.F.);
#23749=ORIENTED_EDGE('',*,*,#16568,.T.);
#23750=ORIENTED_EDGE('',*,*,#16569,.T.);
#23751=ORIENTED_EDGE('',*,*,#16568,.F.);
#23752=ORIENTED_EDGE('',*,*,#16570,.T.);
#23753=ORIENTED_EDGE('',*,*,#16571,.T.);
#23754=ORIENTED_EDGE('',*,*,#16572,.F.);
#23755=ORIENTED_EDGE('',*,*,#16571,.F.);
#23756=ORIENTED_EDGE('',*,*,#16573,.T.);
#23757=ORIENTED_EDGE('',*,*,#16570,.F.);
#23758=ORIENTED_EDGE('',*,*,#16574,.T.);
#23759=ORIENTED_EDGE('',*,*,#16575,.T.);
#23760=ORIENTED_EDGE('',*,*,#16574,.F.);
#23761=ORIENTED_EDGE('',*,*,#16573,.F.);
#23762=ORIENTED_EDGE('',*,*,#16572,.T.);
#23763=ORIENTED_EDGE('',*,*,#16569,.F.);
#23764=ORIENTED_EDGE('',*,*,#16576,.F.);
#23765=ORIENTED_EDGE('',*,*,#16577,.F.);
#23766=ORIENTED_EDGE('',*,*,#16578,.F.);
#23767=ORIENTED_EDGE('',*,*,#16579,.F.);
#23768=ORIENTED_EDGE('',*,*,#16580,.F.);
#23769=ORIENTED_EDGE('',*,*,#16581,.F.);
#23770=ORIENTED_EDGE('',*,*,#16565,.T.);
#23771=ORIENTED_EDGE('',*,*,#16575,.F.);
#23772=ORIENTED_EDGE('',*,*,#16576,.T.);
#23773=ORIENTED_EDGE('',*,*,#16582,.F.);
#23774=ORIENTED_EDGE('',*,*,#16583,.F.);
#23775=ORIENTED_EDGE('',*,*,#16584,.T.);
#23776=ORIENTED_EDGE('',*,*,#16577,.T.);
#23777=ORIENTED_EDGE('',*,*,#16584,.F.);
#23778=ORIENTED_EDGE('',*,*,#16585,.F.);
#23779=ORIENTED_EDGE('',*,*,#16586,.T.);
#23780=ORIENTED_EDGE('',*,*,#16578,.T.);
#23781=ORIENTED_EDGE('',*,*,#16586,.F.);
#23782=ORIENTED_EDGE('',*,*,#16587,.F.);
#23783=ORIENTED_EDGE('',*,*,#16588,.T.);
#23784=ORIENTED_EDGE('',*,*,#16579,.T.);
#23785=ORIENTED_EDGE('',*,*,#16588,.F.);
#23786=ORIENTED_EDGE('',*,*,#16589,.F.);
#23787=ORIENTED_EDGE('',*,*,#16590,.T.);
#23788=ORIENTED_EDGE('',*,*,#16580,.T.);
#23789=ORIENTED_EDGE('',*,*,#16590,.F.);
#23790=ORIENTED_EDGE('',*,*,#16591,.F.);
#23791=ORIENTED_EDGE('',*,*,#16592,.T.);
#23792=ORIENTED_EDGE('',*,*,#16581,.T.);
#23793=ORIENTED_EDGE('',*,*,#16592,.F.);
#23794=ORIENTED_EDGE('',*,*,#16593,.F.);
#23795=ORIENTED_EDGE('',*,*,#16582,.T.);
#23796=ORIENTED_EDGE('',*,*,#16583,.T.);
#23797=ORIENTED_EDGE('',*,*,#16593,.T.);
#23798=ORIENTED_EDGE('',*,*,#16591,.T.);
#23799=ORIENTED_EDGE('',*,*,#16589,.T.);
#23800=ORIENTED_EDGE('',*,*,#16587,.T.);
#23801=ORIENTED_EDGE('',*,*,#16585,.T.);
#23802=CYLINDRICAL_SURFACE('',#26043,3.4);
#23803=CYLINDRICAL_SURFACE('',#26046,3.4);
#23804=CYLINDRICAL_SURFACE('',#26049,2.99999999999999);
#23805=CYLINDRICAL_SURFACE('',#26052,2.99999999999999);
#23806=CYLINDRICAL_SURFACE('',#26071,3.);
#23807=CYLINDRICAL_SURFACE('',#26074,3.);
#23808=CYLINDRICAL_SURFACE('',#26077,4.25000000000001);
#23809=CYLINDRICAL_SURFACE('',#26080,4.25000000000001);
#23810=CYLINDRICAL_SURFACE('',#26096,2.1);
#23811=CYLINDRICAL_SURFACE('',#26099,2.1);
#23812=CYLINDRICAL_SURFACE('',#26102,2.1);
#23813=CYLINDRICAL_SURFACE('',#26105,2.1);
#23814=CYLINDRICAL_SURFACE('',#26108,3.);
#23815=CYLINDRICAL_SURFACE('',#26111,3.);
#23816=CYLINDRICAL_SURFACE('',#26114,5.5);
#23817=CYLINDRICAL_SURFACE('',#26117,3.3);
#23818=CYLINDRICAL_SURFACE('',#26120,5.5);
#23819=CYLINDRICAL_SURFACE('',#26123,3.3);
#23820=CYLINDRICAL_SURFACE('',#26126,17.5);
#23821=CYLINDRICAL_SURFACE('',#26129,35.);
#23822=CYLINDRICAL_SURFACE('',#26143,2.1);
#23823=CYLINDRICAL_SURFACE('',#26146,2.1);
#23824=CYLINDRICAL_SURFACE('',#26149,2.1);
#23825=CYLINDRICAL_SURFACE('',#26152,2.1);
#23826=CYLINDRICAL_SURFACE('',#26155,2.1);
#23827=CYLINDRICAL_SURFACE('',#26158,2.1);
#23828=CYLINDRICAL_SURFACE('',#26161,18.);
#23829=CYLINDRICAL_SURFACE('',#26174,10.);
#23830=CYLINDRICAL_SURFACE('',#26175,10.);
#23831=CYLINDRICAL_SURFACE('',#26177,2.99999999999999);
#23832=CYLINDRICAL_SURFACE('',#26180,2.99999999999999);
#23833=CYLINDRICAL_SURFACE('',#26183,3.3);
#23834=CYLINDRICAL_SURFACE('',#26186,3.3);
#23835=CYLINDRICAL_SURFACE('',#26189,3.3);
#23836=CYLINDRICAL_SURFACE('',#26192,3.3);
#23837=CYLINDRICAL_SURFACE('',#26204,3.3);
#23838=CYLINDRICAL_SURFACE('',#26207,3.3);
#23839=CYLINDRICAL_SURFACE('',#26210,3.3);
#23840=CYLINDRICAL_SURFACE('',#26213,3.3);
#23841=CYLINDRICAL_SURFACE('',#26216,3.3);
#23842=CYLINDRICAL_SURFACE('',#26219,3.3);
#23843=CYLINDRICAL_SURFACE('',#26230,5.49999999999995);
#23844=CYLINDRICAL_SURFACE('',#26233,3.49999999999995);
#23845=CYLINDRICAL_SURFACE('',#26244,5.49999999999995);
#23846=CYLINDRICAL_SURFACE('',#26247,3.49999999999995);
#23847=CYLINDRICAL_SURFACE('',#26258,5.49999999999995);
#23848=CYLINDRICAL_SURFACE('',#26261,3.49999999999995);
#23849=CYLINDRICAL_SURFACE('',#26272,5.49999999999995);
#23850=CYLINDRICAL_SURFACE('',#26275,3.49999999999995);
#23851=CYLINDRICAL_SURFACE('',#26286,5.49999999999995);
#23852=CYLINDRICAL_SURFACE('',#26289,3.49999999999995);
#23853=CYLINDRICAL_SURFACE('',#26300,5.49999999999995);
#23854=CYLINDRICAL_SURFACE('',#26303,3.49999999999995);
#23855=CYLINDRICAL_SURFACE('',#26314,5.50000000000001);
#23856=CYLINDRICAL_SURFACE('',#26317,3.5);
#23857=CYLINDRICAL_SURFACE('',#26328,5.50000000000001);
#23858=CYLINDRICAL_SURFACE('',#26331,3.5);
#23859=CYLINDRICAL_SURFACE('',#26342,5.50000000000001);
#23860=CYLINDRICAL_SURFACE('',#26345,3.5);
#23861=CYLINDRICAL_SURFACE('',#26356,5.50000000000001);
#23862=CYLINDRICAL_SURFACE('',#26359,3.5);
#23863=CYLINDRICAL_SURFACE('',#26370,5.50000000000001);
#23864=CYLINDRICAL_SURFACE('',#26373,3.5);
#23865=CYLINDRICAL_SURFACE('',#26384,5.50000000000001);
#23866=CYLINDRICAL_SURFACE('',#26387,3.5);
#23867=CYLINDRICAL_SURFACE('',#26398,5.50000000000001);
#23868=CYLINDRICAL_SURFACE('',#26401,3.5);
#23869=CYLINDRICAL_SURFACE('',#26412,5.5);
#23870=CYLINDRICAL_SURFACE('',#26415,3.5);
#23871=CYLINDRICAL_SURFACE('',#26426,5.5);
#23872=CYLINDRICAL_SURFACE('',#26429,3.5);
#23873=CYLINDRICAL_SURFACE('',#26547,2.3);
#23874=CYLINDRICAL_SURFACE('',#26548,2.3);
#23875=CYLINDRICAL_SURFACE('',#26549,0.5);
#23876=CYLINDRICAL_SURFACE('',#26550,0.5);
#23877=CYLINDRICAL_SURFACE('',#26551,0.5);
#23878=CYLINDRICAL_SURFACE('',#26552,0.5);
#23879=CYLINDRICAL_SURFACE('',#26553,0.5);
#23880=CYLINDRICAL_SURFACE('',#26554,0.5);
#23881=CYLINDRICAL_SURFACE('',#26555,0.5);
#23882=CYLINDRICAL_SURFACE('',#26556,0.5);
#23883=CYLINDRICAL_SURFACE('',#26557,1.);
#23884=CYLINDRICAL_SURFACE('',#26563,2.3);
#23885=CYLINDRICAL_SURFACE('',#26564,2.3);
#23886=CYLINDRICAL_SURFACE('',#26565,0.5);
#23887=CYLINDRICAL_SURFACE('',#26566,0.5);
#23888=CYLINDRICAL_SURFACE('',#26567,0.5);
#23889=CYLINDRICAL_SURFACE('',#26568,0.5);
#23890=CYLINDRICAL_SURFACE('',#26569,0.5);
#23891=CYLINDRICAL_SURFACE('',#26570,0.5);
#23892=CYLINDRICAL_SURFACE('',#26571,0.5);
#23893=CYLINDRICAL_SURFACE('',#26572,0.5);
#23894=CYLINDRICAL_SURFACE('',#26573,1.);
#23895=CYLINDRICAL_SURFACE('',#26593,2.5);
#23896=CYLINDRICAL_SURFACE('',#26596,2.5);
#23897=CYLINDRICAL_SURFACE('',#26599,3.65);
#23898=CYLINDRICAL_SURFACE('',#26604,3.32349999999999);
#23899=CYLINDRICAL_SURFACE('',#26607,3.3235);
#23900=CYLINDRICAL_SURFACE('',#26610,3.32349999999999);
#23901=CYLINDRICAL_SURFACE('',#26613,3.3235);
#23902=CYLINDRICAL_SURFACE('',#26616,2.5);
#23903=CYLINDRICAL_SURFACE('',#26619,2.5);
#23904=CYLINDRICAL_SURFACE('',#26622,3.65);
#23905=CYLINDRICAL_SURFACE('',#26625,0.500000000000006);
#23906=CYLINDRICAL_SURFACE('',#26631,0.5);
#23907=CYLINDRICAL_SURFACE('',#26637,4.);
#23908=CYLINDRICAL_SURFACE('',#26639,4.99995);
#23909=CYLINDRICAL_SURFACE('',#26669,2.3);
#23910=CYLINDRICAL_SURFACE('',#26672,2.3);
#23911=CYLINDRICAL_SURFACE('',#26675,2.3);
#23912=CYLINDRICAL_SURFACE('',#26678,2.3);
#23913=CYLINDRICAL_SURFACE('',#26681,0.5);
#23914=CYLINDRICAL_SURFACE('',#26684,0.5);
#23915=CYLINDRICAL_SURFACE('',#26687,0.5);
#23916=CYLINDRICAL_SURFACE('',#26690,0.5);
#23917=CYLINDRICAL_SURFACE('',#26693,0.5);
#23918=CYLINDRICAL_SURFACE('',#26696,0.5);
#23919=CYLINDRICAL_SURFACE('',#26699,0.5);
#23920=CYLINDRICAL_SURFACE('',#26702,0.5);
#23921=CYLINDRICAL_SURFACE('',#26705,0.5);
#23922=CYLINDRICAL_SURFACE('',#26708,0.5);
#23923=CYLINDRICAL_SURFACE('',#26711,0.5);
#23924=CYLINDRICAL_SURFACE('',#26714,0.5);
#23925=CYLINDRICAL_SURFACE('',#26717,0.5);
#23926=CYLINDRICAL_SURFACE('',#26720,0.5);
#23927=CYLINDRICAL_SURFACE('',#26723,0.5);
#23928=CYLINDRICAL_SURFACE('',#26726,0.5);
#23929=CYLINDRICAL_SURFACE('',#26767,0.450000000000001);
#23930=CYLINDRICAL_SURFACE('',#26770,0.450000000000001);
#23931=CYLINDRICAL_SURFACE('',#26773,0.55);
#23932=CYLINDRICAL_SURFACE('',#26775,2.25);
#23933=CYLINDRICAL_SURFACE('',#26777,0.549999999999998);
#23934=CYLINDRICAL_SURFACE('',#26780,0.55);
#23935=CYLINDRICAL_SURFACE('',#26783,0.55);
#23936=CYLINDRICAL_SURFACE('',#26786,0.55);
#23937=CYLINDRICAL_SURFACE('',#26788,2.25);
#23938=CYLINDRICAL_SURFACE('',#26790,0.55);
#23939=CYLINDRICAL_SURFACE('',#26795,0.550000000000001);
#23940=CYLINDRICAL_SURFACE('',#26797,2.25);
#23941=CYLINDRICAL_SURFACE('',#26799,0.550000000000002);
#23942=CYLINDRICAL_SURFACE('',#26802,0.55);
#23943=CYLINDRICAL_SURFACE('',#26805,0.55);
#23944=CYLINDRICAL_SURFACE('',#26808,0.55);
#23945=CYLINDRICAL_SURFACE('',#26810,2.25);
#23946=CYLINDRICAL_SURFACE('',#26812,0.55);
#23947=CYLINDRICAL_SURFACE('',#26815,0.450000000000001);
#23948=CYLINDRICAL_SURFACE('',#26818,0.450000000000001);
#23949=CYLINDRICAL_SURFACE('',#26857,0.5);
#23950=CYLINDRICAL_SURFACE('',#26872,0.5);
#23951=CYLINDRICAL_SURFACE('',#26875,0.5);
#23952=CYLINDRICAL_SURFACE('',#26878,0.5);
#23953=CYLINDRICAL_SURFACE('',#26880,2.3);
#23954=CYLINDRICAL_SURFACE('',#26882,0.5);
#23955=CYLINDRICAL_SURFACE('',#26885,0.5);
#23956=CYLINDRICAL_SURFACE('',#26888,0.5);
#23957=CYLINDRICAL_SURFACE('',#26891,0.5);
#23958=CYLINDRICAL_SURFACE('',#26893,2.3);
#23959=CYLINDRICAL_SURFACE('',#26895,0.5);
#23960=CYLINDRICAL_SURFACE('',#26900,0.5);
#23961=CYLINDRICAL_SURFACE('',#26902,2.3);
#23962=CYLINDRICAL_SURFACE('',#26904,0.5);
#23963=CYLINDRICAL_SURFACE('',#26907,0.5);
#23964=CYLINDRICAL_SURFACE('',#26910,0.5);
#23965=CYLINDRICAL_SURFACE('',#26913,0.5);
#23966=CYLINDRICAL_SURFACE('',#26915,2.3);
#23967=CYLINDRICAL_SURFACE('',#26917,0.5);
#23968=CYLINDRICAL_SURFACE('',#26920,0.5);
#23969=CYLINDRICAL_SURFACE('',#26923,0.5);
#23970=CYLINDRICAL_SURFACE('',#26931,0.500000000000006);
#23971=CYLINDRICAL_SURFACE('',#26933,2.);
#23972=CYLINDRICAL_SURFACE('',#26941,2.);
#23973=CYLINDRICAL_SURFACE('',#26997,0.450000000000001);
#23974=CYLINDRICAL_SURFACE('',#27000,0.450000000000001);
#23975=CYLINDRICAL_SURFACE('',#27003,0.55);
#23976=CYLINDRICAL_SURFACE('',#27005,2.25);
#23977=CYLINDRICAL_SURFACE('',#27007,0.55);
#23978=CYLINDRICAL_SURFACE('',#27010,0.55);
#23979=CYLINDRICAL_SURFACE('',#27013,0.55);
#23980=CYLINDRICAL_SURFACE('',#27016,0.550000000000002);
#23981=CYLINDRICAL_SURFACE('',#27018,2.25);
#23982=CYLINDRICAL_SURFACE('',#27020,0.55);
#23983=CYLINDRICAL_SURFACE('',#27025,0.55);
#23984=CYLINDRICAL_SURFACE('',#27027,2.25);
#23985=CYLINDRICAL_SURFACE('',#27029,0.55);
#23986=CYLINDRICAL_SURFACE('',#27032,0.55);
#23987=CYLINDRICAL_SURFACE('',#27035,0.55);
#23988=CYLINDRICAL_SURFACE('',#27038,0.549999999999998);
#23989=CYLINDRICAL_SURFACE('',#27040,2.25);
#23990=CYLINDRICAL_SURFACE('',#27042,0.550000000000001);
#23991=CYLINDRICAL_SURFACE('',#27045,0.450000000000001);
#23992=CYLINDRICAL_SURFACE('',#27048,0.450000000000001);
#23993=CYLINDRICAL_SURFACE('',#27119,0.5);
#23994=CYLINDRICAL_SURFACE('',#27121,0.5);
#23995=CYLINDRICAL_SURFACE('',#27126,0.5);
#23996=CYLINDRICAL_SURFACE('',#27128,0.5);
#23997=CYLINDRICAL_SURFACE('',#27130,2.3);
#23998=CYLINDRICAL_SURFACE('',#27132,0.5);
#23999=CYLINDRICAL_SURFACE('',#27134,0.5);
#24000=CYLINDRICAL_SURFACE('',#27138,0.5);
#24001=CYLINDRICAL_SURFACE('',#27140,0.5);
#24002=CYLINDRICAL_SURFACE('',#27142,2.3);
#24003=CYLINDRICAL_SURFACE('',#27146,0.5);
#24004=CYLINDRICAL_SURFACE('',#27148,0.5);
#24005=CYLINDRICAL_SURFACE('',#27150,2.3);
#24006=CYLINDRICAL_SURFACE('',#27152,0.5);
#24007=CYLINDRICAL_SURFACE('',#27154,0.5);
#24008=CYLINDRICAL_SURFACE('',#27159,0.5);
#24009=CYLINDRICAL_SURFACE('',#27161,0.5);
#24010=CYLINDRICAL_SURFACE('',#27163,2.3);
#24011=CYLINDRICAL_SURFACE('',#27165,0.5);
#24012=CYLINDRICAL_SURFACE('',#27167,0.5);
#24013=CYLINDRICAL_SURFACE('',#27184,4.99995);
#24014=CYLINDRICAL_SURFACE('',#27188,5.5);
#24015=CYLINDRICAL_SURFACE('',#27189,5.50000000000001);
#24016=CYLINDRICAL_SURFACE('',#27190,5.5);
#24017=CYLINDRICAL_SURFACE('',#27191,5.49999999999999);
#24018=CYLINDRICAL_SURFACE('',#27207,3.);
#24019=CYLINDRICAL_SURFACE('',#27210,4.);
#24020=CYLINDRICAL_SURFACE('',#27276,6.00000000000003);
#24021=CYLINDRICAL_SURFACE('',#27286,7.5000000000001);
#24022=CYLINDRICAL_SURFACE('',#27294,9.99999999999998);
#24023=CYLINDRICAL_SURFACE('',#27303,7.5);
#24024=CYLINDRICAL_SURFACE('',#27305,7.15);
#24025=CYLINDRICAL_SURFACE('',#27308,7.5);
#24026=CYLINDRICAL_SURFACE('',#27327,2.);
#24027=CYLINDRICAL_SURFACE('',#27329,2.45849999999999);
#24028=CYLINDRICAL_SURFACE('',#27330,3.3);
#24029=CYLINDRICAL_SURFACE('',#27333,3.3);
#24030=CYLINDRICAL_SURFACE('',#27336,3.3);
#24031=CYLINDRICAL_SURFACE('',#27339,3.3);
#24032=CYLINDRICAL_SURFACE('',#27342,3.3);
#24033=CYLINDRICAL_SURFACE('',#27345,3.3);
#24034=CYLINDRICAL_SURFACE('',#27348,18.);
#24035=CYLINDRICAL_SURFACE('',#27351,13.);
#24036=CYLINDRICAL_SURFACE('',#27354,12.75);
#24037=CYLINDRICAL_SURFACE('',#27357,10.);
#24038=CYLINDRICAL_SURFACE('',#27360,12.75);
#24039=CYLINDRICAL_SURFACE('',#27363,13.);
#24040=CYLINDRICAL_SURFACE('',#27376,29.);
#24041=CYLINDRICAL_SURFACE('',#27378,29.);
#24042=CYLINDRICAL_SURFACE('',#27396,16.);
#24043=CYLINDRICAL_SURFACE('',#27399,7.5);
#24044=CYLINDRICAL_SURFACE('',#27402,16.);
#24045=CYLINDRICAL_SURFACE('',#27405,5.5);
#24046=CYLINDRICAL_SURFACE('',#27408,3.3);
#24047=CYLINDRICAL_SURFACE('',#27411,5.5);
#24048=CYLINDRICAL_SURFACE('',#27414,3.3);
#24049=CYLINDRICAL_SURFACE('',#27436,0.85);
#24050=CYLINDRICAL_SURFACE('',#27439,0.85);
#24051=CYLINDRICAL_SURFACE('',#27442,7.15);
#24052=CYLINDRICAL_SURFACE('',#27445,8.8);
#24053=CYLINDRICAL_SURFACE('',#27459,1.9);
#24054=CYLINDRICAL_SURFACE('',#27461,1.9);
#24055=CYLINDRICAL_SURFACE('',#27462,1.9);
#24056=CYLINDRICAL_SURFACE('',#27464,1.9);
#24057=CYLINDRICAL_SURFACE('',#27472,14.);
#24058=CYLINDRICAL_SURFACE('',#27475,9.75);
#24059=CYLINDRICAL_SURFACE('',#27478,7.5);
#24060=CYLINDRICAL_SURFACE('',#27481,9.75);
#24061=CYLINDRICAL_SURFACE('',#27484,14.);
#24062=CYLINDRICAL_SURFACE('',#27487,3.1);
#24063=CYLINDRICAL_SURFACE('',#27490,3.1);
#24064=CYLINDRICAL_SURFACE('',#27493,3.1);
#24065=CYLINDRICAL_SURFACE('',#27496,3.1);
#24066=CYLINDRICAL_SURFACE('',#27499,3.50000000000001);
#24067=CYLINDRICAL_SURFACE('',#27502,3.5);
#24068=CYLINDRICAL_SURFACE('',#27505,3.50000000000001);
#24069=CYLINDRICAL_SURFACE('',#27508,3.50000000000001);
#24070=CYLINDRICAL_SURFACE('',#27511,5.5);
#24071=CYLINDRICAL_SURFACE('',#27514,3.3);
#24072=CYLINDRICAL_SURFACE('',#27517,5.5);
#24073=CYLINDRICAL_SURFACE('',#27520,3.3);
#24074=CYLINDRICAL_SURFACE('',#27523,5.5);
#24075=CYLINDRICAL_SURFACE('',#27526,3.3);
#24076=CYLINDRICAL_SURFACE('',#27529,5.5);
#24077=CYLINDRICAL_SURFACE('',#27532,3.3);
#24078=CYLINDRICAL_SURFACE('',#27610,2.);
#24079=CYLINDRICAL_SURFACE('',#27617,2.);
#24080=CYLINDRICAL_SURFACE('',#27625,12.5);
#24081=CYLINDRICAL_SURFACE('',#27628,10.5);
#24082=CYLINDRICAL_SURFACE('',#27631,6.9585);
#24083=CYLINDRICAL_SURFACE('',#27632,12.5);
#24084=CYLINDRICAL_SURFACE('',#27639,12.5);
#24085=CYLINDRICAL_SURFACE('',#27642,12.5);
#24086=CYLINDRICAL_SURFACE('',#27645,12.5);
#24087=CYLINDRICAL_SURFACE('',#27669,9.75);
#24088=CYLINDRICAL_SURFACE('',#27672,7.5);
#24089=CYLINDRICAL_SURFACE('',#27682,3.);
#24090=CYLINDRICAL_SURFACE('',#27685,3.);
#24091=CYLINDRICAL_SURFACE('',#27688,3.25);
#24092=CYLINDRICAL_SURFACE('',#27691,3.25);
#24093=CYLINDRICAL_SURFACE('',#27694,3.25);
#24094=CYLINDRICAL_SURFACE('',#27697,3.25);
#24095=CYLINDRICAL_SURFACE('',#27717,2.);
#24096=CYLINDRICAL_SURFACE('',#27721,2.);
#24097=CYLINDRICAL_SURFACE('',#27917,2.);
#24098=CYLINDRICAL_SURFACE('',#27921,2.);
#24099=CYLINDRICAL_SURFACE('',#27925,2.);
#24100=CYLINDRICAL_SURFACE('',#27929,13.5);
#24101=CYLINDRICAL_SURFACE('',#27933,2.);
#24102=CYLINDRICAL_SURFACE('',#27937,2.);
#24103=CYLINDRICAL_SURFACE('',#27941,2.);
#24104=CYLINDRICAL_SURFACE('',#27949,2.5);
#24105=CYLINDRICAL_SURFACE('',#27961,5.);
#24106=CYLINDRICAL_SURFACE('',#27978,3.);
#24107=CYLINDRICAL_SURFACE('',#27983,5.);
#24108=CYLINDRICAL_SURFACE('',#28000,3.);
#24109=CYLINDRICAL_SURFACE('',#28017,17.5);
#24110=CYLINDRICAL_SURFACE('',#28019,17.5);
#24111=CYLINDRICAL_SURFACE('',#28021,13.);
#24112=CYLINDRICAL_SURFACE('',#28023,13.);
#24113=CYLINDRICAL_SURFACE('',#28025,13.);
#24114=CYLINDRICAL_SURFACE('',#28027,13.);
#24115=CYLINDRICAL_SURFACE('',#28029,27.5);
#24116=CYLINDRICAL_SURFACE('',#28033,6.00000000000001);
#24117=CYLINDRICAL_SURFACE('',#28036,2.5);
#24118=CYLINDRICAL_SURFACE('',#28041,3.3);
#24119=CYLINDRICAL_SURFACE('',#28045,2.5);
#24120=CYLINDRICAL_SURFACE('',#28049,5.5);
#24121=CYLINDRICAL_SURFACE('',#28050,5.5);
#24122=CYLINDRICAL_SURFACE('',#28054,2.5);
#24123=CYLINDRICAL_SURFACE('',#28055,2.5);
#24124=CYLINDRICAL_SURFACE('',#28060,3.3);
#24125=CYLINDRICAL_SURFACE('',#28082,6.);
#24126=CYLINDRICAL_SURFACE('',#28083,6.);
#24127=CYLINDRICAL_SURFACE('',#28084,27.5);
#24128=CYLINDRICAL_SURFACE('',#28086,2.1);
#24129=CYLINDRICAL_SURFACE('',#28096,13.);
#24130=CYLINDRICAL_SURFACE('',#28098,13.);
#24131=CYLINDRICAL_SURFACE('',#28100,13.);
#24132=CYLINDRICAL_SURFACE('',#28102,17.5);
#24133=CYLINDRICAL_SURFACE('',#28104,17.5);
#24134=CYLINDRICAL_SURFACE('',#28106,13.);
#24135=CYLINDRICAL_SURFACE('',#28112,27.5);
#24136=CYLINDRICAL_SURFACE('',#28136,27.);
#24137=CYLINDRICAL_SURFACE('',#28167,27.);
#24138=CYLINDRICAL_SURFACE('',#28168,27.);
#24139=CYLINDRICAL_SURFACE('',#28189,27.);
#24140=CYLINDRICAL_SURFACE('',#28195,1.4361111111);
#24141=CYLINDRICAL_SURFACE('',#28206,0.4033333333);
#24142=CYLINDRICAL_SURFACE('',#28208,27.);
#24143=CYLINDRICAL_SURFACE('',#28214,2.5);
#24144=CYLINDRICAL_SURFACE('',#28226,5.);
#24145=CYLINDRICAL_SURFACE('',#28243,3.);
#24146=CYLINDRICAL_SURFACE('',#28248,5.);
#24147=CYLINDRICAL_SURFACE('',#28265,3.);
#24148=CYLINDRICAL_SURFACE('',#28282,17.5);
#24149=CYLINDRICAL_SURFACE('',#28284,17.5);
#24150=CYLINDRICAL_SURFACE('',#28286,13.);
#24151=CYLINDRICAL_SURFACE('',#28288,13.);
#24152=CYLINDRICAL_SURFACE('',#28290,13.);
#24153=CYLINDRICAL_SURFACE('',#28292,13.);
#24154=CYLINDRICAL_SURFACE('',#28294,27.5);
#24155=CYLINDRICAL_SURFACE('',#28298,9.5);
#24156=CYLINDRICAL_SURFACE('',#28301,2.5);
#24157=CYLINDRICAL_SURFACE('',#28306,3.3);
#24158=CYLINDRICAL_SURFACE('',#28310,2.5);
#24159=CYLINDRICAL_SURFACE('',#28314,5.5);
#24160=CYLINDRICAL_SURFACE('',#28315,5.5);
#24161=CYLINDRICAL_SURFACE('',#28319,2.5);
#24162=CYLINDRICAL_SURFACE('',#28320,2.5);
#24163=CYLINDRICAL_SURFACE('',#28325,3.3);
#24164=CYLINDRICAL_SURFACE('',#28347,9.5);
#24165=CYLINDRICAL_SURFACE('',#28348,9.5);
#24166=CYLINDRICAL_SURFACE('',#28349,27.5);
#24167=CYLINDRICAL_SURFACE('',#28351,2.1);
#24168=CYLINDRICAL_SURFACE('',#28356,13.);
#24169=CYLINDRICAL_SURFACE('',#28358,13.);
#24170=CYLINDRICAL_SURFACE('',#28360,13.);
#24171=CYLINDRICAL_SURFACE('',#28362,17.5);
#24172=CYLINDRICAL_SURFACE('',#28364,17.5);
#24173=CYLINDRICAL_SURFACE('',#28366,13.);
#24174=CYLINDRICAL_SURFACE('',#28372,27.5);
#24175=CYLINDRICAL_SURFACE('',#28396,27.);
#24176=CYLINDRICAL_SURFACE('',#28427,27.);
#24177=CYLINDRICAL_SURFACE('',#28428,27.);
#24178=CYLINDRICAL_SURFACE('',#28449,27.);
#24179=CYLINDRICAL_SURFACE('',#28455,1.4361111111);
#24180=CYLINDRICAL_SURFACE('',#28466,0.4033333333);
#24181=CYLINDRICAL_SURFACE('',#28468,27.);
#24182=CYLINDRICAL_SURFACE('',#28480,2.5);
#24183=CYLINDRICAL_SURFACE('',#28484,2.5);
#24184=CYLINDRICAL_SURFACE('',#28488,2.5);
#24185=CYLINDRICAL_SURFACE('',#28492,2.5);
#24186=CYLINDRICAL_SURFACE('',#28496,2.5);
#24187=CYLINDRICAL_SURFACE('',#28500,2.5);
#24188=CYLINDRICAL_SURFACE('',#28504,2.5);
#24189=CYLINDRICAL_SURFACE('',#28508,2.5);
#24190=CYLINDRICAL_SURFACE('',#28512,2.5);
#24191=CYLINDRICAL_SURFACE('',#28516,2.5);
#24192=CYLINDRICAL_SURFACE('',#28520,2.5);
#24193=CYLINDRICAL_SURFACE('',#28524,2.5);
#24194=CYLINDRICAL_SURFACE('',#28528,2.5);
#24195=CYLINDRICAL_SURFACE('',#28532,2.5);
#24196=CYLINDRICAL_SURFACE('',#28536,2.5);
#24197=CYLINDRICAL_SURFACE('',#28540,2.5);
#24198=CYLINDRICAL_SURFACE('',#28544,2.5);
#24199=CYLINDRICAL_SURFACE('',#28562,0.200000000000001);
#24200=CYLINDRICAL_SURFACE('',#28563,0.200000000000001);
#24201=CYLINDRICAL_SURFACE('',#28565,5.);
#24202=CYLINDRICAL_SURFACE('',#28574,3.);
#24203=CYLINDRICAL_SURFACE('',#28599,4.25);
#24204=CYLINDRICAL_SURFACE('',#28601,2.065);
#24205=CYLINDRICAL_SURFACE('',#28604,3.);
#24206=CYLINDRICAL_SURFACE('',#28623,5.);
#24207=CYLINDRICAL_SURFACE('',#28626,2.5);
#24208=CYLINDRICAL_SURFACE('',#28631,4.25);
#24209=CYLINDRICAL_SURFACE('',#28634,2.5);
#24210=CYLINDRICAL_SURFACE('',#28642,4.);
#24211=CYLINDRICAL_SURFACE('',#28645,4.);
#24212=CYLINDRICAL_SURFACE('',#28648,3.25);
#24213=CYLINDRICAL_SURFACE('',#28651,3.25);
#24214=CYLINDRICAL_SURFACE('',#28654,3.25);
#24215=CYLINDRICAL_SURFACE('',#28657,3.25);
#24216=CYLINDRICAL_SURFACE('',#28660,3.25);
#24217=CYLINDRICAL_SURFACE('',#28663,3.25);
#24218=CYLINDRICAL_SURFACE('',#28666,3.25);
#24219=CYLINDRICAL_SURFACE('',#28669,3.25);
#24220=CYLINDRICAL_SURFACE('',#28681,5.);
#24221=CYLINDRICAL_SURFACE('',#28690,3.);
#24222=ADVANCED_FACE('',(#2269),#23802,.F.);
#24223=ADVANCED_FACE('',(#2270),#23803,.F.);
#24224=ADVANCED_FACE('',(#2271),#23804,.F.);
#24225=ADVANCED_FACE('',(#2272),#23805,.F.);
#24226=ADVANCED_FACE('',(#2273),#1498,.F.);
#24227=ADVANCED_FACE('',(#2274),#1499,.F.);
#24228=ADVANCED_FACE('',(#2275),#1500,.F.);
#24229=ADVANCED_FACE('',(#2276),#1501,.F.);
#24230=ADVANCED_FACE('',(#2277,#1168,#1169,#1170,#1171,#1172,#1173),#1502,
 .F.);
#24231=ADVANCED_FACE('',(#2278,#1174,#1175,#1176,#1177,#1178,#1179),#1503,
 .T.);
#24232=ADVANCED_FACE('',(#2279),#1504,.F.);
#24233=ADVANCED_FACE('',(#2280),#1505,.F.);
#24234=ADVANCED_FACE('',(#2281),#1506,.F.);
#24235=ADVANCED_FACE('',(#2282),#1507,.F.);
#24236=ADVANCED_FACE('',(#2283),#1508,.F.);
#24237=ADVANCED_FACE('',(#2284),#1509,.F.);
#24238=ADVANCED_FACE('',(#2285),#1510,.F.);
#24239=ADVANCED_FACE('',(#2286),#1511,.F.);
#24240=ADVANCED_FACE('',(#2287),#23806,.F.);
#24241=ADVANCED_FACE('',(#2288),#23807,.F.);
#24242=ADVANCED_FACE('',(#2289),#23808,.F.);
#24243=ADVANCED_FACE('',(#2290),#23809,.F.);
#24244=ADVANCED_FACE('',(#2291),#1512,.T.);
#24245=ADVANCED_FACE('',(#2292),#1513,.F.);
#24246=ADVANCED_FACE('',(#2293),#1514,.F.);
#24247=ADVANCED_FACE('',(#2294),#1515,.F.);
#24248=ADVANCED_FACE('',(#2295),#1516,.F.);
#24249=ADVANCED_FACE('',(#2296),#1517,.T.);
#24250=ADVANCED_FACE('',(#2297,#1180,#1181,#1182,#1183),#1518,.F.);
#24251=ADVANCED_FACE('',(#2298),#1519,.F.);
#24252=ADVANCED_FACE('',(#2299),#1520,.F.);
#24253=ADVANCED_FACE('',(#2300),#1521,.F.);
#24254=ADVANCED_FACE('',(#2301),#1522,.F.);
#24255=ADVANCED_FACE('',(#2302,#1184,#1185,#1186,#1187),#1523,.T.);
#24256=ADVANCED_FACE('',(#2303),#23810,.F.);
#24257=ADVANCED_FACE('',(#2304),#23811,.F.);
#24258=ADVANCED_FACE('',(#2305),#23812,.F.);
#24259=ADVANCED_FACE('',(#2306),#23813,.F.);
#24260=ADVANCED_FACE('',(#2307),#23814,.F.);
#24261=ADVANCED_FACE('',(#2308),#23815,.F.);
#24262=ADVANCED_FACE('',(#2309),#23816,.F.);
#24263=ADVANCED_FACE('',(#2310),#23817,.F.);
#24264=ADVANCED_FACE('',(#2311),#23818,.F.);
#24265=ADVANCED_FACE('',(#2312),#23819,.F.);
#24266=ADVANCED_FACE('',(#2313),#23820,.F.);
#24267=ADVANCED_FACE('',(#2314),#23821,.F.);
#24268=ADVANCED_FACE('',(#2315,#1188,#1189,#1190,#1191,#1192,#1193,#1194,
#1195,#1196),#1524,.T.);
#24269=ADVANCED_FACE('',(#2316),#1525,.F.);
#24270=ADVANCED_FACE('',(#2317),#1526,.F.);
#24271=ADVANCED_FACE('',(#2318),#1527,.F.);
#24272=ADVANCED_FACE('',(#2319),#1528,.F.);
#24273=ADVANCED_FACE('',(#2320,#1197,#1198,#1199,#1200,#1201,#1202,#1203,
#1204,#1205),#1529,.F.);
#24274=ADVANCED_FACE('',(#2321,#1206),#1530,.T.);
#24275=ADVANCED_FACE('',(#2322,#1207),#1531,.F.);
#24276=ADVANCED_FACE('',(#2323,#1208),#1532,.F.);
#24277=ADVANCED_FACE('',(#2324),#23822,.F.);
#24278=ADVANCED_FACE('',(#2325),#23823,.F.);
#24279=ADVANCED_FACE('',(#2326),#23824,.F.);
#24280=ADVANCED_FACE('',(#2327),#23825,.F.);
#24281=ADVANCED_FACE('',(#2328),#23826,.F.);
#24282=ADVANCED_FACE('',(#2329),#23827,.F.);
#24283=ADVANCED_FACE('',(#2330),#23828,.F.);
#24284=ADVANCED_FACE('',(#2331,#1209,#1210,#1211,#1212,#1213,#1214,#1215),
#1533,.F.);
#24285=ADVANCED_FACE('',(#2332),#1534,.F.);
#24286=ADVANCED_FACE('',(#2333,#1216,#1217,#1218,#1219,#1220,#1221,#1222),
#1535,.F.);
#24287=ADVANCED_FACE('',(#2334),#1536,.F.);
#24288=ADVANCED_FACE('',(#2335),#1537,.F.);
#24289=ADVANCED_FACE('',(#2336),#1538,.T.);
#24290=ADVANCED_FACE('',(#2337),#23829,.T.);
#24291=ADVANCED_FACE('',(#2338),#23830,.T.);
#24292=ADVANCED_FACE('',(#2339),#23831,.F.);
#24293=ADVANCED_FACE('',(#2340),#23832,.F.);
#24294=ADVANCED_FACE('',(#2341),#23833,.F.);
#24295=ADVANCED_FACE('',(#2342),#23834,.F.);
#24296=ADVANCED_FACE('',(#2343),#23835,.F.);
#24297=ADVANCED_FACE('',(#2344),#23836,.F.);
#24298=ADVANCED_FACE('',(#2345),#1539,.F.);
#24299=ADVANCED_FACE('',(#2346),#1540,.F.);
#24300=ADVANCED_FACE('',(#2347),#1541,.F.);
#24301=ADVANCED_FACE('',(#2348),#1542,.F.);
#24302=ADVANCED_FACE('',(#2349,#1223,#1224,#1225,#1226,#1227,#1228),#1543,
 .T.);
#24303=ADVANCED_FACE('',(#2350,#1229,#1230,#1231,#1232,#1233,#1234),#1544,
 .F.);
#24304=ADVANCED_FACE('',(#2351),#23837,.F.);
#24305=ADVANCED_FACE('',(#2352),#23838,.F.);
#24306=ADVANCED_FACE('',(#2353),#23839,.F.);
#24307=ADVANCED_FACE('',(#2354),#23840,.F.);
#24308=ADVANCED_FACE('',(#2355),#23841,.F.);
#24309=ADVANCED_FACE('',(#2356),#23842,.F.);
#24310=ADVANCED_FACE('',(#2357),#1545,.F.);
#24311=ADVANCED_FACE('',(#2358),#1546,.F.);
#24312=ADVANCED_FACE('',(#2359),#1547,.F.);
#24313=ADVANCED_FACE('',(#2360),#1548,.F.);
#24314=ADVANCED_FACE('',(#2361,#1235,#1236,#1237,#1238,#1239,#1240),#1549,
 .T.);
#24315=ADVANCED_FACE('',(#2362,#1241,#1242,#1243,#1244,#1245,#1246),#1550,
 .F.);
#24316=ADVANCED_FACE('',(#2363),#23843,.F.);
#24317=ADVANCED_FACE('',(#2364),#23844,.F.);
#24318=ADVANCED_FACE('',(#2365),#23845,.F.);
#24319=ADVANCED_FACE('',(#2366),#23846,.F.);
#24320=ADVANCED_FACE('',(#2367),#23847,.F.);
#24321=ADVANCED_FACE('',(#2368),#23848,.F.);
#24322=ADVANCED_FACE('',(#2369),#23849,.F.);
#24323=ADVANCED_FACE('',(#2370),#23850,.F.);
#24324=ADVANCED_FACE('',(#2371),#23851,.F.);
#24325=ADVANCED_FACE('',(#2372),#23852,.F.);
#24326=ADVANCED_FACE('',(#2373),#23853,.F.);
#24327=ADVANCED_FACE('',(#2374),#23854,.F.);
#24328=ADVANCED_FACE('',(#2375),#23855,.F.);
#24329=ADVANCED_FACE('',(#2376),#23856,.F.);
#24330=ADVANCED_FACE('',(#2377),#23857,.F.);
#24331=ADVANCED_FACE('',(#2378),#23858,.F.);
#24332=ADVANCED_FACE('',(#2379),#23859,.F.);
#24333=ADVANCED_FACE('',(#2380),#23860,.F.);
#24334=ADVANCED_FACE('',(#2381),#23861,.F.);
#24335=ADVANCED_FACE('',(#2382),#23862,.F.);
#24336=ADVANCED_FACE('',(#2383),#23863,.F.);
#24337=ADVANCED_FACE('',(#2384),#23864,.F.);
#24338=ADVANCED_FACE('',(#2385),#23865,.F.);
#24339=ADVANCED_FACE('',(#2386),#23866,.F.);
#24340=ADVANCED_FACE('',(#2387),#23867,.F.);
#24341=ADVANCED_FACE('',(#2388),#23868,.F.);
#24342=ADVANCED_FACE('',(#2389),#23869,.F.);
#24343=ADVANCED_FACE('',(#2390),#23870,.F.);
#24344=ADVANCED_FACE('',(#2391),#23871,.F.);
#24345=ADVANCED_FACE('',(#2392),#23872,.F.);
#24346=ADVANCED_FACE('',(#2393),#1551,.F.);
#24347=ADVANCED_FACE('',(#2394),#1552,.F.);
#24348=ADVANCED_FACE('',(#2395),#1553,.T.);
#24349=ADVANCED_FACE('',(#2396),#1554,.F.);
#24350=ADVANCED_FACE('',(#2397),#1555,.T.);
#24351=ADVANCED_FACE('',(#2398),#1556,.F.);
#24352=ADVANCED_FACE('',(#2399),#1557,.F.);
#24353=ADVANCED_FACE('',(#2400),#1558,.F.);
#24354=ADVANCED_FACE('',(#2401),#1559,.F.);
#24355=ADVANCED_FACE('',(#2402),#1560,.F.);
#24356=ADVANCED_FACE('',(#2403),#1561,.F.);
#24357=ADVANCED_FACE('',(#2404),#1562,.F.);
#24358=ADVANCED_FACE('',(#2405),#1563,.F.);
#24359=ADVANCED_FACE('',(#2406),#1564,.F.);
#24360=ADVANCED_FACE('',(#2407),#1565,.F.);
#24361=ADVANCED_FACE('',(#2408),#1566,.F.);
#24362=ADVANCED_FACE('',(#2409),#1567,.F.);
#24363=ADVANCED_FACE('',(#2410),#1568,.F.);
#24364=ADVANCED_FACE('',(#2411),#1569,.F.);
#24365=ADVANCED_FACE('',(#2412),#1570,.F.);
#24366=ADVANCED_FACE('',(#2413),#1571,.F.);
#24367=ADVANCED_FACE('',(#2414),#1572,.F.);
#24368=ADVANCED_FACE('',(#2415),#1573,.F.);
#24369=ADVANCED_FACE('',(#2416),#1574,.F.);
#24370=ADVANCED_FACE('',(#2417),#1575,.F.);
#24371=ADVANCED_FACE('',(#2418),#1576,.F.);
#24372=ADVANCED_FACE('',(#2419),#1577,.F.);
#24373=ADVANCED_FACE('',(#2420),#1578,.F.);
#24374=ADVANCED_FACE('',(#2421),#1579,.F.);
#24375=ADVANCED_FACE('',(#2422),#1580,.F.);
#24376=ADVANCED_FACE('',(#2423),#1581,.F.);
#24377=ADVANCED_FACE('',(#2424),#1582,.F.);
#24378=ADVANCED_FACE('',(#2425),#1583,.F.);
#24379=ADVANCED_FACE('',(#2426),#1584,.F.);
#24380=ADVANCED_FACE('',(#2427),#1585,.F.);
#24381=ADVANCED_FACE('',(#2428),#1586,.F.);
#24382=ADVANCED_FACE('',(#2429),#1587,.F.);
#24383=ADVANCED_FACE('',(#2430),#1588,.F.);
#24384=ADVANCED_FACE('',(#2431),#1589,.F.);
#24385=ADVANCED_FACE('',(#2432),#1590,.F.);
#24386=ADVANCED_FACE('',(#2433),#1591,.F.);
#24387=ADVANCED_FACE('',(#2434),#1592,.F.);
#24388=ADVANCED_FACE('',(#2435),#1593,.F.);
#24389=ADVANCED_FACE('',(#2436),#1594,.F.);
#24390=ADVANCED_FACE('',(#2437),#1595,.F.);
#24391=ADVANCED_FACE('',(#2438),#1596,.F.);
#24392=ADVANCED_FACE('',(#2439),#1597,.F.);
#24393=ADVANCED_FACE('',(#2440),#1598,.T.);
#24394=ADVANCED_FACE('',(#2441),#1599,.F.);
#24395=ADVANCED_FACE('',(#2442),#1600,.F.);
#24396=ADVANCED_FACE('',(#2443),#1601,.F.);
#24397=ADVANCED_FACE('',(#2444),#1602,.F.);
#24398=ADVANCED_FACE('',(#2445),#1603,.F.);
#24399=ADVANCED_FACE('',(#2446),#1604,.T.);
#24400=ADVANCED_FACE('',(#2447),#1605,.T.);
#24401=ADVANCED_FACE('',(#2448,#1247,#1248,#1249,#1250,#1251,#1252,#1253,
#1254,#1255,#1256,#1257,#1258,#1259,#1260,#1261),#1606,.T.);
#24402=ADVANCED_FACE('',(#2449),#1607,.T.);
#24403=ADVANCED_FACE('',(#2450),#1608,.T.);
#24404=ADVANCED_FACE('',(#2451),#1609,.T.);
#24405=ADVANCED_FACE('',(#2452),#1610,.T.);
#24406=ADVANCED_FACE('',(#2453),#1611,.T.);
#24407=ADVANCED_FACE('',(#2454),#1612,.T.);
#24408=ADVANCED_FACE('',(#2455),#1613,.T.);
#24409=ADVANCED_FACE('',(#2456),#23873,.F.);
#24410=ADVANCED_FACE('',(#2457),#23874,.F.);
#24411=ADVANCED_FACE('',(#2458),#23875,.T.);
#24412=ADVANCED_FACE('',(#2459),#23876,.T.);
#24413=ADVANCED_FACE('',(#2460),#23877,.T.);
#24414=ADVANCED_FACE('',(#2461),#23878,.T.);
#24415=ADVANCED_FACE('',(#2462),#23879,.F.);
#24416=ADVANCED_FACE('',(#2463),#23880,.F.);
#24417=ADVANCED_FACE('',(#2464),#23881,.T.);
#24418=ADVANCED_FACE('',(#2465),#23882,.T.);
#24419=ADVANCED_FACE('',(#2466),#23883,.T.);
#24420=ADVANCED_FACE('',(#2467),#1614,.F.);
#24421=ADVANCED_FACE('',(#2468),#1615,.F.);
#24422=ADVANCED_FACE('',(#2469),#1616,.F.);
#24423=ADVANCED_FACE('',(#2470),#1617,.F.);
#24424=ADVANCED_FACE('',(#2471),#1618,.F.);
#24425=ADVANCED_FACE('',(#2472),#23884,.F.);
#24426=ADVANCED_FACE('',(#2473),#23885,.F.);
#24427=ADVANCED_FACE('',(#2474),#23886,.T.);
#24428=ADVANCED_FACE('',(#2475),#23887,.T.);
#24429=ADVANCED_FACE('',(#2476),#23888,.T.);
#24430=ADVANCED_FACE('',(#2477),#23889,.T.);
#24431=ADVANCED_FACE('',(#2478),#23890,.F.);
#24432=ADVANCED_FACE('',(#2479),#23891,.F.);
#24433=ADVANCED_FACE('',(#2480),#23892,.T.);
#24434=ADVANCED_FACE('',(#2481),#23893,.T.);
#24435=ADVANCED_FACE('',(#2482),#23894,.T.);
#24436=ADVANCED_FACE('',(#2483),#1619,.F.);
#24437=ADVANCED_FACE('',(#2484),#1620,.F.);
#24438=ADVANCED_FACE('',(#2485),#1621,.F.);
#24439=ADVANCED_FACE('',(#2486,#1262),#1622,.F.);
#24440=ADVANCED_FACE('',(#2487,#1263),#1623,.F.);
#24441=ADVANCED_FACE('',(#2488,#1264),#1624,.F.);
#24442=ADVANCED_FACE('',(#2489,#1265),#1625,.F.);
#24443=ADVANCED_FACE('',(#2490,#1266),#1626,.F.);
#24444=ADVANCED_FACE('',(#2491,#1267),#1627,.F.);
#24445=ADVANCED_FACE('',(#2492,#1268),#1628,.F.);
#24446=ADVANCED_FACE('',(#2493,#1269),#1629,.F.);
#24447=ADVANCED_FACE('',(#2494,#1270),#1630,.F.);
#24448=ADVANCED_FACE('',(#2495,#1271),#1631,.F.);
#24449=ADVANCED_FACE('',(#2496,#1272),#1632,.F.);
#24450=ADVANCED_FACE('',(#2497,#1273),#1633,.F.);
#24451=ADVANCED_FACE('',(#2498,#1274),#1634,.F.);
#24452=ADVANCED_FACE('',(#2499,#1275),#1635,.F.);
#24453=ADVANCED_FACE('',(#2500,#1276),#1636,.F.);
#24454=ADVANCED_FACE('',(#2501),#23895,.F.);
#24455=ADVANCED_FACE('',(#2502),#23896,.F.);
#24456=ADVANCED_FACE('',(#2503),#23897,.F.);
#24457=ADVANCED_FACE('',(#2504),#524,.F.);
#24458=ADVANCED_FACE('',(#2505),#525,.F.);
#24459=ADVANCED_FACE('',(#2506),#23898,.F.);
#24460=ADVANCED_FACE('',(#2507),#23899,.F.);
#24461=ADVANCED_FACE('',(#2508),#23900,.F.);
#24462=ADVANCED_FACE('',(#2509),#23901,.F.);
#24463=ADVANCED_FACE('',(#2510),#23902,.F.);
#24464=ADVANCED_FACE('',(#2511),#23903,.F.);
#24465=ADVANCED_FACE('',(#2512),#23904,.F.);
#24466=ADVANCED_FACE('',(#2513),#23905,.F.);
#24467=ADVANCED_FACE('',(#2514),#526,.F.);
#24468=ADVANCED_FACE('',(#2515),#527,.F.);
#24469=ADVANCED_FACE('',(#2516),#23906,.F.);
#24470=ADVANCED_FACE('',(#2517),#402,.F.);
#24471=ADVANCED_FACE('',(#2518),#23907,.T.);
#24472=ADVANCED_FACE('',(#2519),#23908,.F.);
#24473=ADVANCED_FACE('',(#2520),#1637,.T.);
#24474=ADVANCED_FACE('',(#2521),#1638,.T.);
#24475=ADVANCED_FACE('',(#2522),#1639,.T.);
#24476=ADVANCED_FACE('',(#2523),#1640,.T.);
#24477=ADVANCED_FACE('',(#2524),#1641,.T.);
#24478=ADVANCED_FACE('',(#2525),#1642,.T.);
#24479=ADVANCED_FACE('',(#2526),#1643,.T.);
#24480=ADVANCED_FACE('',(#2527),#1644,.T.);
#24481=ADVANCED_FACE('',(#2528),#1645,.T.);
#24482=ADVANCED_FACE('',(#2529),#1646,.T.);
#24483=ADVANCED_FACE('',(#2530),#1647,.T.);
#24484=ADVANCED_FACE('',(#2531),#1648,.T.);
#24485=ADVANCED_FACE('',(#2532),#1649,.T.);
#24486=ADVANCED_FACE('',(#2533),#1650,.T.);
#24487=ADVANCED_FACE('',(#2534),#1651,.T.);
#24488=ADVANCED_FACE('',(#2535),#1652,.T.);
#24489=ADVANCED_FACE('',(#2536),#1653,.T.);
#24490=ADVANCED_FACE('',(#2537),#1654,.T.);
#24491=ADVANCED_FACE('',(#2538),#1655,.T.);
#24492=ADVANCED_FACE('',(#2539),#1656,.T.);
#24493=ADVANCED_FACE('',(#2540),#1657,.T.);
#24494=ADVANCED_FACE('',(#2541),#23909,.T.);
#24495=ADVANCED_FACE('',(#2542),#23910,.T.);
#24496=ADVANCED_FACE('',(#2543),#23911,.T.);
#24497=ADVANCED_FACE('',(#2544),#23912,.T.);
#24498=ADVANCED_FACE('',(#2545),#23913,.T.);
#24499=ADVANCED_FACE('',(#2546),#23914,.T.);
#24500=ADVANCED_FACE('',(#2547),#23915,.F.);
#24501=ADVANCED_FACE('',(#2548),#23916,.F.);
#24502=ADVANCED_FACE('',(#2549),#23917,.F.);
#24503=ADVANCED_FACE('',(#2550),#23918,.F.);
#24504=ADVANCED_FACE('',(#2551),#23919,.F.);
#24505=ADVANCED_FACE('',(#2552),#23920,.F.);
#24506=ADVANCED_FACE('',(#2553),#23921,.T.);
#24507=ADVANCED_FACE('',(#2554),#23922,.T.);
#24508=ADVANCED_FACE('',(#2555),#23923,.F.);
#24509=ADVANCED_FACE('',(#2556),#23924,.F.);
#24510=ADVANCED_FACE('',(#2557),#23925,.F.);
#24511=ADVANCED_FACE('',(#2558),#23926,.F.);
#24512=ADVANCED_FACE('',(#2559),#23927,.F.);
#24513=ADVANCED_FACE('',(#2560),#23928,.F.);
#24514=ADVANCED_FACE('',(#2561,#1277),#1658,.T.);
#24515=ADVANCED_FACE('',(#2562),#1659,.F.);
#24516=ADVANCED_FACE('',(#2563,#1278),#1660,.T.);
#24517=ADVANCED_FACE('',(#2564),#1661,.F.);
#24518=ADVANCED_FACE('',(#2565),#1662,.F.);
#24519=ADVANCED_FACE('',(#2566),#1663,.F.);
#24520=ADVANCED_FACE('',(#2567),#1664,.F.);
#24521=ADVANCED_FACE('',(#2568),#1665,.F.);
#24522=ADVANCED_FACE('',(#2569),#1666,.F.);
#24523=ADVANCED_FACE('',(#2570),#1667,.F.);
#24524=ADVANCED_FACE('',(#2571),#1668,.F.);
#24525=ADVANCED_FACE('',(#2572),#1669,.F.);
#24526=ADVANCED_FACE('',(#2573),#1670,.F.);
#24527=ADVANCED_FACE('',(#2574),#1671,.F.);
#24528=ADVANCED_FACE('',(#2575),#1672,.F.);
#24529=ADVANCED_FACE('',(#2576),#1673,.T.);
#24530=ADVANCED_FACE('',(#2577,#1279),#1674,.F.);
#24531=ADVANCED_FACE('',(#2578),#1675,.T.);
#24532=ADVANCED_FACE('',(#2579),#23929,.T.);
#24533=ADVANCED_FACE('',(#2580),#1676,.T.);
#24534=ADVANCED_FACE('',(#2581),#23930,.T.);
#24535=ADVANCED_FACE('',(#2582),#1677,.T.);
#24536=ADVANCED_FACE('',(#2583),#23931,.F.);
#24537=ADVANCED_FACE('',(#2584),#23932,.T.);
#24538=ADVANCED_FACE('',(#2585),#23933,.F.);
#24539=ADVANCED_FACE('',(#2586),#1678,.T.);
#24540=ADVANCED_FACE('',(#2587),#23934,.F.);
#24541=ADVANCED_FACE('',(#2588),#1679,.T.);
#24542=ADVANCED_FACE('',(#2589),#23935,.F.);
#24543=ADVANCED_FACE('',(#2590),#1680,.T.);
#24544=ADVANCED_FACE('',(#2591),#23936,.F.);
#24545=ADVANCED_FACE('',(#2592),#23937,.T.);
#24546=ADVANCED_FACE('',(#2593),#23938,.F.);
#24547=ADVANCED_FACE('',(#2594),#1681,.T.);
#24548=ADVANCED_FACE('',(#2595),#1682,.T.);
#24549=ADVANCED_FACE('',(#2596),#1683,.T.);
#24550=ADVANCED_FACE('',(#2597),#23939,.F.);
#24551=ADVANCED_FACE('',(#2598),#23940,.T.);
#24552=ADVANCED_FACE('',(#2599),#23941,.F.);
#24553=ADVANCED_FACE('',(#2600),#1684,.T.);
#24554=ADVANCED_FACE('',(#2601),#23942,.F.);
#24555=ADVANCED_FACE('',(#2602),#1685,.T.);
#24556=ADVANCED_FACE('',(#2603),#23943,.F.);
#24557=ADVANCED_FACE('',(#2604),#1686,.T.);
#24558=ADVANCED_FACE('',(#2605),#23944,.F.);
#24559=ADVANCED_FACE('',(#2606),#23945,.T.);
#24560=ADVANCED_FACE('',(#2607),#23946,.F.);
#24561=ADVANCED_FACE('',(#2608),#1687,.T.);
#24562=ADVANCED_FACE('',(#2609),#23947,.T.);
#24563=ADVANCED_FACE('',(#2610),#1688,.T.);
#24564=ADVANCED_FACE('',(#2611),#23948,.T.);
#24565=ADVANCED_FACE('',(#2612),#1689,.T.);
#24566=ADVANCED_FACE('',(#2613),#1690,.T.);
#24567=ADVANCED_FACE('',(#2614),#1691,.T.);
#24568=ADVANCED_FACE('',(#2615),#1692,.T.);
#24569=ADVANCED_FACE('',(#2616),#1693,.T.);
#24570=ADVANCED_FACE('',(#2617),#1694,.T.);
#24571=ADVANCED_FACE('',(#2618),#1695,.T.);
#24572=ADVANCED_FACE('',(#2619),#1696,.T.);
#24573=ADVANCED_FACE('',(#2620),#1697,.T.);
#24574=ADVANCED_FACE('',(#2621),#1698,.T.);
#24575=ADVANCED_FACE('',(#2622),#1699,.T.);
#24576=ADVANCED_FACE('',(#2623),#1700,.T.);
#24577=ADVANCED_FACE('',(#2624),#1701,.F.);
#24578=ADVANCED_FACE('',(#2625),#1702,.F.);
#24579=ADVANCED_FACE('',(#2626),#1703,.F.);
#24580=ADVANCED_FACE('',(#2627),#23949,.F.);
#24581=ADVANCED_FACE('',(#2628),#1704,.T.);
#24582=ADVANCED_FACE('',(#2629),#1705,.T.);
#24583=ADVANCED_FACE('',(#2630),#1706,.T.);
#24584=ADVANCED_FACE('',(#2631),#1707,.F.);
#24585=ADVANCED_FACE('',(#2632),#1708,.F.);
#24586=ADVANCED_FACE('',(#2633),#1709,.F.);
#24587=ADVANCED_FACE('',(#2634),#1710,.F.);
#24588=ADVANCED_FACE('',(#2635),#1711,.F.);
#24589=ADVANCED_FACE('',(#2636),#1712,.F.);
#24590=ADVANCED_FACE('',(#2637),#1713,.F.);
#24591=ADVANCED_FACE('',(#2638),#1714,.T.);
#24592=ADVANCED_FACE('',(#2639),#1715,.T.);
#24593=ADVANCED_FACE('',(#2640),#23950,.T.);
#24594=ADVANCED_FACE('',(#2641),#1716,.T.);
#24595=ADVANCED_FACE('',(#2642),#23951,.T.);
#24596=ADVANCED_FACE('',(#2643),#1717,.T.);
#24597=ADVANCED_FACE('',(#2644),#23952,.F.);
#24598=ADVANCED_FACE('',(#2645),#23953,.T.);
#24599=ADVANCED_FACE('',(#2646),#23954,.F.);
#24600=ADVANCED_FACE('',(#2647),#1718,.T.);
#24601=ADVANCED_FACE('',(#2648),#23955,.F.);
#24602=ADVANCED_FACE('',(#2649),#1719,.T.);
#24603=ADVANCED_FACE('',(#2650),#23956,.F.);
#24604=ADVANCED_FACE('',(#2651),#1720,.T.);
#24605=ADVANCED_FACE('',(#2652),#23957,.F.);
#24606=ADVANCED_FACE('',(#2653),#23958,.T.);
#24607=ADVANCED_FACE('',(#2654),#23959,.F.);
#24608=ADVANCED_FACE('',(#2655),#1721,.T.);
#24609=ADVANCED_FACE('',(#2656),#1722,.T.);
#24610=ADVANCED_FACE('',(#2657),#1723,.T.);
#24611=ADVANCED_FACE('',(#2658),#23960,.F.);
#24612=ADVANCED_FACE('',(#2659),#23961,.T.);
#24613=ADVANCED_FACE('',(#2660),#23962,.F.);
#24614=ADVANCED_FACE('',(#2661),#1724,.T.);
#24615=ADVANCED_FACE('',(#2662),#23963,.F.);
#24616=ADVANCED_FACE('',(#2663),#1725,.T.);
#24617=ADVANCED_FACE('',(#2664),#23964,.F.);
#24618=ADVANCED_FACE('',(#2665),#1726,.T.);
#24619=ADVANCED_FACE('',(#2666),#23965,.F.);
#24620=ADVANCED_FACE('',(#2667),#23966,.T.);
#24621=ADVANCED_FACE('',(#2668),#23967,.F.);
#24622=ADVANCED_FACE('',(#2669),#1727,.T.);
#24623=ADVANCED_FACE('',(#2670),#23968,.T.);
#24624=ADVANCED_FACE('',(#2671),#1728,.T.);
#24625=ADVANCED_FACE('',(#2672),#23969,.T.);
#24626=ADVANCED_FACE('',(#2673),#1729,.T.);
#24627=ADVANCED_FACE('',(#2674,#1280),#1730,.T.);
#24628=ADVANCED_FACE('',(#2675),#1731,.T.);
#24629=ADVANCED_FACE('',(#2676),#1732,.T.);
#24630=ADVANCED_FACE('',(#2677),#1733,.F.);
#24631=ADVANCED_FACE('',(#2678),#1734,.F.);
#24632=ADVANCED_FACE('',(#2679),#23970,.F.);
#24633=ADVANCED_FACE('',(#2680),#23971,.F.);
#24634=ADVANCED_FACE('',(#2681),#1735,.T.);
#24635=ADVANCED_FACE('',(#2682),#1736,.F.);
#24636=ADVANCED_FACE('',(#2683),#1737,.F.);
#24637=ADVANCED_FACE('',(#2684),#1738,.T.);
#24638=ADVANCED_FACE('',(#2685),#23972,.F.);
#24639=ADVANCED_FACE('',(#2686,#1281),#1739,.F.);
#24640=ADVANCED_FACE('',(#2687),#1740,.F.);
#24641=ADVANCED_FACE('',(#2688),#1741,.F.);
#24642=ADVANCED_FACE('',(#2689),#1742,.T.);
#24643=ADVANCED_FACE('',(#2690),#1743,.F.);
#24644=ADVANCED_FACE('',(#2691),#1744,.F.);
#24645=ADVANCED_FACE('',(#2692),#1745,.F.);
#24646=ADVANCED_FACE('',(#2693,#1282),#1746,.T.);
#24647=ADVANCED_FACE('',(#2694),#1747,.T.);
#24648=ADVANCED_FACE('',(#2695,#1283),#1748,.F.);
#24649=ADVANCED_FACE('',(#2696),#1749,.F.);
#24650=ADVANCED_FACE('',(#2697),#1750,.T.);
#24651=ADVANCED_FACE('',(#2698),#1751,.F.);
#24652=ADVANCED_FACE('',(#2699,#1284),#1752,.F.);
#24653=ADVANCED_FACE('',(#2700),#1753,.T.);
#24654=ADVANCED_FACE('',(#2701),#1754,.T.);
#24655=ADVANCED_FACE('',(#2702),#1755,.F.);
#24656=ADVANCED_FACE('',(#2703),#1756,.F.);
#24657=ADVANCED_FACE('',(#2704),#1757,.F.);
#24658=ADVANCED_FACE('',(#2705),#1758,.F.);
#24659=ADVANCED_FACE('',(#2706),#1759,.F.);
#24660=ADVANCED_FACE('',(#2707),#1760,.F.);
#24661=ADVANCED_FACE('',(#2708),#1761,.F.);
#24662=ADVANCED_FACE('',(#2709),#1762,.F.);
#24663=ADVANCED_FACE('',(#2710),#1763,.F.);
#24664=ADVANCED_FACE('',(#2711),#1764,.F.);
#24665=ADVANCED_FACE('',(#2712),#23973,.T.);
#24666=ADVANCED_FACE('',(#2713),#1765,.F.);
#24667=ADVANCED_FACE('',(#2714),#23974,.T.);
#24668=ADVANCED_FACE('',(#2715),#1766,.F.);
#24669=ADVANCED_FACE('',(#2716),#23975,.F.);
#24670=ADVANCED_FACE('',(#2717),#23976,.T.);
#24671=ADVANCED_FACE('',(#2718),#23977,.F.);
#24672=ADVANCED_FACE('',(#2719),#1767,.F.);
#24673=ADVANCED_FACE('',(#2720),#23978,.F.);
#24674=ADVANCED_FACE('',(#2721),#1768,.F.);
#24675=ADVANCED_FACE('',(#2722),#23979,.F.);
#24676=ADVANCED_FACE('',(#2723),#1769,.F.);
#24677=ADVANCED_FACE('',(#2724),#23980,.F.);
#24678=ADVANCED_FACE('',(#2725),#23981,.T.);
#24679=ADVANCED_FACE('',(#2726),#23982,.F.);
#24680=ADVANCED_FACE('',(#2727),#1770,.F.);
#24681=ADVANCED_FACE('',(#2728),#1771,.F.);
#24682=ADVANCED_FACE('',(#2729),#1772,.F.);
#24683=ADVANCED_FACE('',(#2730),#23983,.F.);
#24684=ADVANCED_FACE('',(#2731),#23984,.T.);
#24685=ADVANCED_FACE('',(#2732),#23985,.F.);
#24686=ADVANCED_FACE('',(#2733),#1773,.F.);
#24687=ADVANCED_FACE('',(#2734),#23986,.F.);
#24688=ADVANCED_FACE('',(#2735),#1774,.F.);
#24689=ADVANCED_FACE('',(#2736),#23987,.F.);
#24690=ADVANCED_FACE('',(#2737),#1775,.F.);
#24691=ADVANCED_FACE('',(#2738),#23988,.F.);
#24692=ADVANCED_FACE('',(#2739),#23989,.T.);
#24693=ADVANCED_FACE('',(#2740),#23990,.F.);
#24694=ADVANCED_FACE('',(#2741),#1776,.F.);
#24695=ADVANCED_FACE('',(#2742),#23991,.T.);
#24696=ADVANCED_FACE('',(#2743),#1777,.F.);
#24697=ADVANCED_FACE('',(#2744),#23992,.T.);
#24698=ADVANCED_FACE('',(#2745),#1778,.F.);
#24699=ADVANCED_FACE('',(#2746,#1285),#1779,.T.);
#24700=ADVANCED_FACE('',(#2747),#1780,.T.);
#24701=ADVANCED_FACE('',(#2748),#1781,.F.);
#24702=ADVANCED_FACE('',(#2749),#1782,.F.);
#24703=ADVANCED_FACE('',(#2750,#1286),#1783,.F.);
#24704=ADVANCED_FACE('',(#2751,#1287),#1784,.F.);
#24705=ADVANCED_FACE('',(#2752),#1785,.F.);
#24706=ADVANCED_FACE('',(#2753),#1786,.F.);
#24707=ADVANCED_FACE('',(#2754),#1787,.T.);
#24708=ADVANCED_FACE('',(#2755),#1788,.T.);
#24709=ADVANCED_FACE('',(#2756),#1789,.T.);
#24710=ADVANCED_FACE('',(#2757,#1288,#1289),#1790,.T.);
#24711=ADVANCED_FACE('',(#2758),#1791,.F.);
#24712=ADVANCED_FACE('',(#2759),#1792,.F.);
#24713=ADVANCED_FACE('',(#2760),#1793,.F.);
#24714=ADVANCED_FACE('',(#2761),#1794,.T.);
#24715=ADVANCED_FACE('',(#2762),#1795,.F.);
#24716=ADVANCED_FACE('',(#2763),#1796,.F.);
#24717=ADVANCED_FACE('',(#2764),#1797,.F.);
#24718=ADVANCED_FACE('',(#2765,#1290,#1291),#1798,.T.);
#24719=ADVANCED_FACE('',(#2766),#1799,.T.);
#24720=ADVANCED_FACE('',(#2767),#1800,.T.);
#24721=ADVANCED_FACE('',(#2768),#1801,.T.);
#24722=ADVANCED_FACE('',(#2769),#1802,.T.);
#24723=ADVANCED_FACE('',(#2770,#1292),#1803,.F.);
#24724=ADVANCED_FACE('',(#2771),#1804,.F.);
#24725=ADVANCED_FACE('',(#2772),#1805,.T.);
#24726=ADVANCED_FACE('',(#2773),#1806,.T.);
#24727=ADVANCED_FACE('',(#2774),#1807,.F.);
#24728=ADVANCED_FACE('',(#2775,#1293),#1808,.F.);
#24729=ADVANCED_FACE('',(#2776),#1809,.T.);
#24730=ADVANCED_FACE('',(#2777),#1810,.F.);
#24731=ADVANCED_FACE('',(#2778),#1811,.F.);
#24732=ADVANCED_FACE('',(#2779),#1812,.T.);
#24733=ADVANCED_FACE('',(#2780),#1813,.T.);
#24734=ADVANCED_FACE('',(#2781,#1294),#1814,.F.);
#24735=ADVANCED_FACE('',(#2782),#1815,.T.);
#24736=ADVANCED_FACE('',(#2783),#1816,.T.);
#24737=ADVANCED_FACE('',(#2784),#1817,.F.);
#24738=ADVANCED_FACE('',(#2785,#1295),#1818,.F.);
#24739=ADVANCED_FACE('',(#2786),#1819,.F.);
#24740=ADVANCED_FACE('',(#2787),#1820,.F.);
#24741=ADVANCED_FACE('',(#2788),#23993,.T.);
#24742=ADVANCED_FACE('',(#2789),#23994,.T.);
#24743=ADVANCED_FACE('',(#2790),#1821,.T.);
#24744=ADVANCED_FACE('',(#2791),#1822,.T.);
#24745=ADVANCED_FACE('',(#2792),#1823,.T.);
#24746=ADVANCED_FACE('',(#2793),#23995,.F.);
#24747=ADVANCED_FACE('',(#2794),#23996,.F.);
#24748=ADVANCED_FACE('',(#2795),#23997,.T.);
#24749=ADVANCED_FACE('',(#2796),#23998,.F.);
#24750=ADVANCED_FACE('',(#2797),#23999,.F.);
#24751=ADVANCED_FACE('',(#2798),#1824,.T.);
#24752=ADVANCED_FACE('',(#2799),#1825,.T.);
#24753=ADVANCED_FACE('',(#2800),#24000,.F.);
#24754=ADVANCED_FACE('',(#2801),#24001,.F.);
#24755=ADVANCED_FACE('',(#2802),#24002,.T.);
#24756=ADVANCED_FACE('',(#2803),#1826,.T.);
#24757=ADVANCED_FACE('',(#2804),#1827,.T.);
#24758=ADVANCED_FACE('',(#2805),#24003,.F.);
#24759=ADVANCED_FACE('',(#2806),#24004,.F.);
#24760=ADVANCED_FACE('',(#2807),#24005,.T.);
#24761=ADVANCED_FACE('',(#2808),#24006,.F.);
#24762=ADVANCED_FACE('',(#2809),#24007,.F.);
#24763=ADVANCED_FACE('',(#2810),#1828,.T.);
#24764=ADVANCED_FACE('',(#2811),#1829,.T.);
#24765=ADVANCED_FACE('',(#2812),#1830,.T.);
#24766=ADVANCED_FACE('',(#2813),#24008,.F.);
#24767=ADVANCED_FACE('',(#2814),#24009,.F.);
#24768=ADVANCED_FACE('',(#2815),#24010,.T.);
#24769=ADVANCED_FACE('',(#2816),#24011,.T.);
#24770=ADVANCED_FACE('',(#2817),#24012,.T.);
#24771=ADVANCED_FACE('',(#2818),#1831,.F.);
#24772=ADVANCED_FACE('',(#2819,#1296),#1832,.F.);
#24773=ADVANCED_FACE('',(#2820),#1833,.F.);
#24774=ADVANCED_FACE('',(#2821),#1834,.F.);
#24775=ADVANCED_FACE('',(#2822),#1835,.T.);
#24776=ADVANCED_FACE('',(#2823),#1836,.T.);
#24777=ADVANCED_FACE('',(#2824),#1837,.T.);
#24778=ADVANCED_FACE('',(#2825),#1838,.T.);
#24779=ADVANCED_FACE('',(#2826),#1839,.T.);
#24780=ADVANCED_FACE('',(#2827),#1840,.T.);
#24781=ADVANCED_FACE('',(#2828),#1841,.T.);
#24782=ADVANCED_FACE('',(#2829),#1842,.T.);
#24783=ADVANCED_FACE('',(#2830,#1297),#1843,.T.);
#24784=ADVANCED_FACE('',(#2831,#1298),#1844,.F.);
#24785=ADVANCED_FACE('',(#2832),#1845,.F.);
#24786=ADVANCED_FACE('',(#2833),#24013,.F.);
#24787=ADVANCED_FACE('',(#2834),#1846,.F.);
#24788=ADVANCED_FACE('',(#2835),#1847,.T.);
#24789=ADVANCED_FACE('',(#2836),#24014,.F.);
#24790=ADVANCED_FACE('',(#2837),#24015,.F.);
#24791=ADVANCED_FACE('',(#2838),#24016,.F.);
#24792=ADVANCED_FACE('',(#2839),#24017,.F.);
#24793=ADVANCED_FACE('',(#2840),#69,.F.);
#24794=ADVANCED_FACE('',(#2841),#403,.F.);
#24795=ADVANCED_FACE('',(#2842),#528,.T.);
#24796=ADVANCED_FACE('',(#2843),#35,.T.);
#24797=ADVANCED_FACE('',(#2844),#529,.T.);
#24798=ADVANCED_FACE('',(#2845),#530,.T.);
#24799=ADVANCED_FACE('',(#2846),#24018,.T.);
#24800=ADVANCED_FACE('',(#2847),#24019,.T.);
#24801=ADVANCED_FACE('',(#2848),#36,.T.);
#24802=ADVANCED_FACE('',(#2849,#1299),#1848,.F.);
#24803=ADVANCED_FACE('',(#2850,#1300),#1849,.F.);
#24804=ADVANCED_FACE('',(#2851),#1850,.F.);
#24805=ADVANCED_FACE('',(#2852),#1851,.F.);
#24806=ADVANCED_FACE('',(#2853),#1852,.F.);
#24807=ADVANCED_FACE('',(#2854),#1853,.F.);
#24808=ADVANCED_FACE('',(#2855),#1854,.F.);
#24809=ADVANCED_FACE('',(#2856),#1855,.F.);
#24810=ADVANCED_FACE('',(#2857),#1856,.T.);
#24811=ADVANCED_FACE('',(#2858),#1857,.T.);
#24812=ADVANCED_FACE('',(#2859),#1858,.T.);
#24813=ADVANCED_FACE('',(#2860),#1859,.T.);
#24814=ADVANCED_FACE('',(#2861),#1860,.T.);
#24815=ADVANCED_FACE('',(#2862),#1861,.T.);
#24816=ADVANCED_FACE('',(#2863),#1862,.T.);
#24817=ADVANCED_FACE('',(#2864),#531,.T.);
#24818=ADVANCED_FACE('',(#2865),#532,.T.);
#24819=ADVANCED_FACE('',(#2866),#533,.T.);
#24820=ADVANCED_FACE('',(#2867),#534,.T.);
#24821=ADVANCED_FACE('',(#2868),#535,.T.);
#24822=ADVANCED_FACE('',(#2869),#536,.T.);
#24823=ADVANCED_FACE('',(#2870),#537,.T.);
#24824=ADVANCED_FACE('',(#2871),#538,.T.);
#24825=ADVANCED_FACE('',(#2872),#539,.T.);
#24826=ADVANCED_FACE('',(#2873),#540,.T.);
#24827=ADVANCED_FACE('',(#2874),#1863,.T.);
#24828=ADVANCED_FACE('',(#2875),#1864,.T.);
#24829=ADVANCED_FACE('',(#2876),#1865,.T.);
#24830=ADVANCED_FACE('',(#2877),#1866,.T.);
#24831=ADVANCED_FACE('',(#2878),#1867,.T.);
#24832=ADVANCED_FACE('',(#2879),#1868,.T.);
#24833=ADVANCED_FACE('',(#2880,#1301),#1869,.F.);
#24834=ADVANCED_FACE('',(#2881),#24020,.T.);
#24835=ADVANCED_FACE('',(#2882),#70,.F.);
#24836=ADVANCED_FACE('',(#2883),#541,.T.);
#24837=ADVANCED_FACE('',(#2884),#24021,.T.);
#24838=ADVANCED_FACE('',(#2885),#71,.F.);
#24839=ADVANCED_FACE('',(#2886),#542,.T.);
#24840=ADVANCED_FACE('',(#2887),#24022,.T.);
#24841=ADVANCED_FACE('',(#2888),#543,.T.);
#24842=ADVANCED_FACE('',(#2889),#72,.F.);
#24843=ADVANCED_FACE('',(#2890),#24023,.T.);
#24844=ADVANCED_FACE('',(#2891),#24024,.T.);
#24845=ADVANCED_FACE('',(#2892),#24025,.T.);
#24846=ADVANCED_FACE('',(#2893),#544,.T.);
#24847=ADVANCED_FACE('',(#2894,#1302),#1870,.F.);
#24848=ADVANCED_FACE('',(#2895,#1303),#1871,.F.);
#24849=ADVANCED_FACE('',(#2896,#1304),#1872,.F.);
#24850=ADVANCED_FACE('',(#2897,#1305),#1873,.F.);
#24851=ADVANCED_FACE('',(#2898,#1306),#1874,.F.);
#24852=ADVANCED_FACE('',(#2899),#545,.T.);
#24853=ADVANCED_FACE('',(#2900),#1875,.F.);
#24854=ADVANCED_FACE('',(#2901),#1876,.F.);
#24855=ADVANCED_FACE('',(#2902),#1877,.F.);
#24856=ADVANCED_FACE('',(#2903),#1878,.F.);
#24857=ADVANCED_FACE('',(#2904),#1879,.F.);
#24858=ADVANCED_FACE('',(#2905),#24026,.F.);
#24859=ADVANCED_FACE('',(#2906),#24027,.F.);
#24860=ADVANCED_FACE('',(#2907),#24028,.F.);
#24861=ADVANCED_FACE('',(#2908),#24029,.F.);
#24862=ADVANCED_FACE('',(#2909),#24030,.F.);
#24863=ADVANCED_FACE('',(#2910),#24031,.F.);
#24864=ADVANCED_FACE('',(#2911),#24032,.F.);
#24865=ADVANCED_FACE('',(#2912),#24033,.F.);
#24866=ADVANCED_FACE('',(#2913),#24034,.T.);
#24867=ADVANCED_FACE('',(#2914),#24035,.F.);
#24868=ADVANCED_FACE('',(#2915),#24036,.T.);
#24869=ADVANCED_FACE('',(#2916,#1307),#24037,.F.);
#24870=ADVANCED_FACE('',(#2917),#24038,.T.);
#24871=ADVANCED_FACE('',(#2918),#24039,.F.);
#24872=ADVANCED_FACE('',(#2919),#73,.T.);
#24873=ADVANCED_FACE('',(#2920,#1308,#1309,#1310,#1311,#1312,#1313,#1314),
#1880,.F.);
#24874=ADVANCED_FACE('',(#2921),#74,.T.);
#24875=ADVANCED_FACE('',(#2922),#75,.T.);
#24876=ADVANCED_FACE('',(#2923,#1315),#24040,.T.);
#24877=ADVANCED_FACE('',(#2924),#24041,.T.);
#24878=ADVANCED_FACE('',(#2925),#76,.T.);
#24879=ADVANCED_FACE('',(#2926),#77,.T.);
#24880=ADVANCED_FACE('',(#2927,#1316,#1317,#1318,#1319,#1320,#1321,#1322),
#1881,.F.);
#24881=ADVANCED_FACE('',(#2928,#1323),#1882,.F.);
#24882=ADVANCED_FACE('',(#2929,#1324),#1883,.F.);
#24883=ADVANCED_FACE('',(#2930,#1325),#1884,.F.);
#24884=ADVANCED_FACE('',(#2931,#1326),#1885,.F.);
#24885=ADVANCED_FACE('',(#2932,#1327),#1886,.F.);
#24886=ADVANCED_FACE('',(#2933),#1887,.T.);
#24887=ADVANCED_FACE('',(#2934),#1888,.T.);
#24888=ADVANCED_FACE('',(#2935),#24042,.F.);
#24889=ADVANCED_FACE('',(#2936),#24043,.F.);
#24890=ADVANCED_FACE('',(#2937),#24044,.F.);
#24891=ADVANCED_FACE('',(#2938),#24045,.F.);
#24892=ADVANCED_FACE('',(#2939),#24046,.F.);
#24893=ADVANCED_FACE('',(#2940),#24047,.F.);
#24894=ADVANCED_FACE('',(#2941),#24048,.F.);
#24895=ADVANCED_FACE('',(#2942,#1328),#1889,.F.);
#24896=ADVANCED_FACE('',(#2943),#1890,.F.);
#24897=ADVANCED_FACE('',(#2944),#1891,.F.);
#24898=ADVANCED_FACE('',(#2945,#1329,#1330),#1892,.F.);
#24899=ADVANCED_FACE('',(#2946),#1893,.F.);
#24900=ADVANCED_FACE('',(#2947),#1894,.F.);
#24901=ADVANCED_FACE('',(#2948,#1331),#1895,.F.);
#24902=ADVANCED_FACE('',(#2949),#1896,.F.);
#24903=ADVANCED_FACE('',(#2950),#1897,.F.);
#24904=ADVANCED_FACE('',(#2951),#1898,.F.);
#24905=ADVANCED_FACE('',(#2952),#1899,.F.);
#24906=ADVANCED_FACE('',(#2953),#1900,.F.);
#24907=ADVANCED_FACE('',(#2954,#1332),#1901,.T.);
#24908=ADVANCED_FACE('',(#2955,#1333),#1902,.F.);
#24909=ADVANCED_FACE('',(#2956,#1334),#1903,.F.);
#24910=ADVANCED_FACE('',(#2957,#1335),#1904,.F.);
#24911=ADVANCED_FACE('',(#2958,#1336),#1905,.F.);
#24912=ADVANCED_FACE('',(#2959,#1337),#1906,.F.);
#24913=ADVANCED_FACE('',(#2960),#24049,.F.);
#24914=ADVANCED_FACE('',(#2961),#24050,.F.);
#24915=ADVANCED_FACE('',(#2962),#24051,.F.);
#24916=ADVANCED_FACE('',(#2963),#24052,.T.);
#24917=ADVANCED_FACE('',(#2964,#1338,#1339),#1907,.T.);
#24918=ADVANCED_FACE('',(#2965,#1340,#1341),#1908,.F.);
#24919=ADVANCED_FACE('',(#2966),#1909,.F.);
#24920=ADVANCED_FACE('',(#2967),#24053,.T.);
#24921=ADVANCED_FACE('',(#2968),#1910,.F.);
#24922=ADVANCED_FACE('',(#2969),#24054,.F.);
#24923=ADVANCED_FACE('',(#2970),#24055,.F.);
#24924=ADVANCED_FACE('',(#2971),#1911,.F.);
#24925=ADVANCED_FACE('',(#2972),#24056,.T.);
#24926=ADVANCED_FACE('',(#2973),#1912,.F.);
#24927=ADVANCED_FACE('',(#2974),#1913,.F.);
#24928=ADVANCED_FACE('',(#2975),#1914,.F.);
#24929=ADVANCED_FACE('',(#2976),#24057,.F.);
#24930=ADVANCED_FACE('',(#2977),#24058,.F.);
#24931=ADVANCED_FACE('',(#2978),#24059,.F.);
#24932=ADVANCED_FACE('',(#2979),#24060,.F.);
#24933=ADVANCED_FACE('',(#2980),#24061,.F.);
#24934=ADVANCED_FACE('',(#2981),#24062,.T.);
#24935=ADVANCED_FACE('',(#2982),#24063,.T.);
#24936=ADVANCED_FACE('',(#2983),#24064,.T.);
#24937=ADVANCED_FACE('',(#2984),#24065,.T.);
#24938=ADVANCED_FACE('',(#2985),#24066,.F.);
#24939=ADVANCED_FACE('',(#2986),#24067,.F.);
#24940=ADVANCED_FACE('',(#2987),#24068,.F.);
#24941=ADVANCED_FACE('',(#2988),#24069,.F.);
#24942=ADVANCED_FACE('',(#2989),#24070,.F.);
#24943=ADVANCED_FACE('',(#2990),#24071,.F.);
#24944=ADVANCED_FACE('',(#2991),#24072,.F.);
#24945=ADVANCED_FACE('',(#2992),#24073,.F.);
#24946=ADVANCED_FACE('',(#2993),#24074,.F.);
#24947=ADVANCED_FACE('',(#2994),#24075,.F.);
#24948=ADVANCED_FACE('',(#2995),#24076,.F.);
#24949=ADVANCED_FACE('',(#2996),#24077,.F.);
#24950=ADVANCED_FACE('',(#2997,#1342),#1915,.T.);
#24951=ADVANCED_FACE('',(#2998,#1343),#1916,.T.);
#24952=ADVANCED_FACE('',(#2999,#1344),#1917,.T.);
#24953=ADVANCED_FACE('',(#3000,#1345),#1918,.T.);
#24954=ADVANCED_FACE('',(#3001,#1346),#1919,.T.);
#24955=ADVANCED_FACE('',(#3002,#1347,#1348),#1920,.F.);
#24956=ADVANCED_FACE('',(#3003),#1921,.F.);
#24957=ADVANCED_FACE('',(#3004),#1922,.F.);
#24958=ADVANCED_FACE('',(#3005,#1349,#1350,#1351,#1352),#1923,.F.);
#24959=ADVANCED_FACE('',(#3006),#1924,.F.);
#24960=ADVANCED_FACE('',(#3007),#1925,.F.);
#24961=ADVANCED_FACE('',(#3008,#1353,#1354),#1926,.F.);
#24962=ADVANCED_FACE('',(#3009),#1927,.F.);
#24963=ADVANCED_FACE('',(#3010),#1928,.F.);
#24964=ADVANCED_FACE('',(#3011),#1929,.F.);
#24965=ADVANCED_FACE('',(#3012),#1930,.F.);
#24966=ADVANCED_FACE('',(#3013),#1931,.F.);
#24967=ADVANCED_FACE('',(#3014,#1355),#1932,.F.);
#24968=ADVANCED_FACE('',(#3015,#1356),#1933,.F.);
#24969=ADVANCED_FACE('',(#3016,#1357),#1934,.F.);
#24970=ADVANCED_FACE('',(#3017,#1358),#1935,.F.);
#24971=ADVANCED_FACE('',(#3018,#1359),#1936,.F.);
#24972=ADVANCED_FACE('',(#3019,#1360,#1361,#1362,#1363,#1364),#1937,.F.);
#24973=ADVANCED_FACE('',(#3020),#1938,.F.);
#24974=ADVANCED_FACE('',(#3021),#1939,.F.);
#24975=ADVANCED_FACE('',(#3022),#1940,.F.);
#24976=ADVANCED_FACE('',(#3023),#1941,.F.);
#24977=ADVANCED_FACE('',(#3024),#1942,.F.);
#24978=ADVANCED_FACE('',(#3025),#1943,.F.);
#24979=ADVANCED_FACE('',(#3026),#1944,.F.);
#24980=ADVANCED_FACE('',(#3027),#1945,.F.);
#24981=ADVANCED_FACE('',(#3028,#1365),#1946,.T.);
#24982=ADVANCED_FACE('',(#3029,#1366),#1947,.T.);
#24983=ADVANCED_FACE('',(#3030,#1367),#1948,.T.);
#24984=ADVANCED_FACE('',(#3031,#1368),#1949,.T.);
#24985=ADVANCED_FACE('',(#3032),#1950,.F.);
#24986=ADVANCED_FACE('',(#3033),#1951,.F.);
#24987=ADVANCED_FACE('',(#3034),#1952,.F.);
#24988=ADVANCED_FACE('',(#3035),#1953,.F.);
#24989=ADVANCED_FACE('',(#3036),#1954,.F.);
#24990=ADVANCED_FACE('',(#3037),#1955,.F.);
#24991=ADVANCED_FACE('',(#3038),#1956,.T.);
#24992=ADVANCED_FACE('',(#3039),#1957,.F.);
#24993=ADVANCED_FACE('',(#3040),#1958,.F.);
#24994=ADVANCED_FACE('',(#3041),#1959,.F.);
#24995=ADVANCED_FACE('',(#3042),#1960,.F.);
#24996=ADVANCED_FACE('',(#3043),#1961,.F.);
#24997=ADVANCED_FACE('',(#3044),#1962,.F.);
#24998=ADVANCED_FACE('',(#3045),#1963,.T.);
#24999=ADVANCED_FACE('',(#3046),#1964,.F.);
#25000=ADVANCED_FACE('',(#3047),#1965,.F.);
#25001=ADVANCED_FACE('',(#3048),#1966,.F.);
#25002=ADVANCED_FACE('',(#3049),#1967,.F.);
#25003=ADVANCED_FACE('',(#3050),#1968,.F.);
#25004=ADVANCED_FACE('',(#3051),#1969,.F.);
#25005=ADVANCED_FACE('',(#3052),#1970,.T.);
#25006=ADVANCED_FACE('',(#3053),#1971,.F.);
#25007=ADVANCED_FACE('',(#3054),#1972,.F.);
#25008=ADVANCED_FACE('',(#3055),#1973,.F.);
#25009=ADVANCED_FACE('',(#3056),#1974,.F.);
#25010=ADVANCED_FACE('',(#3057),#1975,.F.);
#25011=ADVANCED_FACE('',(#3058),#1976,.F.);
#25012=ADVANCED_FACE('',(#3059),#1977,.T.);
#25013=ADVANCED_FACE('',(#3060,#1369),#1978,.F.);
#25014=ADVANCED_FACE('',(#3061,#1370),#1979,.F.);
#25015=ADVANCED_FACE('',(#3062,#1371),#1980,.F.);
#25016=ADVANCED_FACE('',(#3063,#1372),#1981,.F.);
#25017=ADVANCED_FACE('',(#3064),#546,.F.);
#25018=ADVANCED_FACE('',(#3065),#24078,.F.);
#25019=ADVANCED_FACE('',(#3066),#547,.T.);
#25020=ADVANCED_FACE('',(#3067),#548,.T.);
#25021=ADVANCED_FACE('',(#3068),#24079,.F.);
#25022=ADVANCED_FACE('',(#3069),#549,.F.);
#25023=ADVANCED_FACE('',(#3070),#550,.F.);
#25024=ADVANCED_FACE('',(#3071),#24080,.T.);
#25025=ADVANCED_FACE('',(#3072),#24081,.T.);
#25026=ADVANCED_FACE('',(#3073,#1373),#24082,.F.);
#25027=ADVANCED_FACE('',(#3074,#1374),#24083,.T.);
#25028=ADVANCED_FACE('',(#3075,#1375),#24084,.T.);
#25029=ADVANCED_FACE('',(#3076),#24085,.T.);
#25030=ADVANCED_FACE('',(#3077),#24086,.T.);
#25031=ADVANCED_FACE('',(#3078,#1376),#1982,.F.);
#25032=ADVANCED_FACE('',(#3079,#1377),#1983,.F.);
#25033=ADVANCED_FACE('',(#3080,#1378),#1984,.F.);
#25034=ADVANCED_FACE('',(#3081),#1985,.F.);
#25035=ADVANCED_FACE('',(#3082),#1986,.F.);
#25036=ADVANCED_FACE('',(#3083),#1987,.F.);
#25037=ADVANCED_FACE('',(#3084),#1988,.F.);
#25038=ADVANCED_FACE('',(#3085),#1989,.T.);
#25039=ADVANCED_FACE('',(#3086),#1990,.F.);
#25040=ADVANCED_FACE('',(#3087),#1991,.F.);
#25041=ADVANCED_FACE('',(#3088),#1992,.F.);
#25042=ADVANCED_FACE('',(#3089),#1993,.F.);
#25043=ADVANCED_FACE('',(#3090),#1994,.F.);
#25044=ADVANCED_FACE('',(#3091),#1995,.F.);
#25045=ADVANCED_FACE('',(#3092),#1996,.T.);
#25046=ADVANCED_FACE('',(#3093),#1997,.T.);
#25047=ADVANCED_FACE('',(#3094),#1998,.T.);
#25048=ADVANCED_FACE('',(#3095),#1999,.T.);
#25049=ADVANCED_FACE('',(#3096),#2000,.T.);
#25050=ADVANCED_FACE('',(#3097),#2001,.T.);
#25051=ADVANCED_FACE('',(#3098),#24087,.T.);
#25052=ADVANCED_FACE('',(#3099),#24088,.F.);
#25053=ADVANCED_FACE('',(#3100,#1379),#2002,.F.);
#25054=ADVANCED_FACE('',(#3101,#1380),#2003,.F.);
#25055=ADVANCED_FACE('',(#3102),#24089,.F.);
#25056=ADVANCED_FACE('',(#3103),#24090,.F.);
#25057=ADVANCED_FACE('',(#3104),#24091,.F.);
#25058=ADVANCED_FACE('',(#3105),#24092,.F.);
#25059=ADVANCED_FACE('',(#3106),#24093,.F.);
#25060=ADVANCED_FACE('',(#3107),#24094,.F.);
#25061=ADVANCED_FACE('',(#3108),#2004,.T.);
#25062=ADVANCED_FACE('',(#3109),#2005,.F.);
#25063=ADVANCED_FACE('',(#3110),#2006,.F.);
#25064=ADVANCED_FACE('',(#3111),#2007,.F.);
#25065=ADVANCED_FACE('',(#3112),#2008,.F.);
#25066=ADVANCED_FACE('',(#3113),#2009,.T.);
#25067=ADVANCED_FACE('',(#3114,#1381,#1382,#1383,#1384,#1385,#1386),#2010,
 .F.);
#25068=ADVANCED_FACE('',(#3115),#2011,.F.);
#25069=ADVANCED_FACE('',(#3116),#2012,.F.);
#25070=ADVANCED_FACE('',(#3117),#2013,.F.);
#25071=ADVANCED_FACE('',(#3118),#2014,.F.);
#25072=ADVANCED_FACE('',(#3119,#1387,#1388,#1389,#1390,#1391,#1392),#2015,
 .T.);
#25073=ADVANCED_FACE('',(#3120),#2016,.F.);
#25074=ADVANCED_FACE('',(#3121),#24095,.T.);
#25075=ADVANCED_FACE('',(#3122),#2017,.T.);
#25076=ADVANCED_FACE('',(#3123),#24096,.T.);
#25077=ADVANCED_FACE('',(#3124),#404,.F.);
#25078=ADVANCED_FACE('',(#3125),#405,.T.);
#25079=ADVANCED_FACE('',(#3126),#406,.T.);
#25080=ADVANCED_FACE('',(#3127),#37,.T.);
#25081=ADVANCED_FACE('',(#3128),#407,.T.);
#25082=ADVANCED_FACE('',(#3129),#11,.T.);
#25083=ADVANCED_FACE('',(#3130),#408,.F.);
#25084=ADVANCED_FACE('',(#3131),#409,.F.);
#25085=ADVANCED_FACE('',(#3132),#410,.T.);
#25086=ADVANCED_FACE('',(#3133),#38,.T.);
#25087=ADVANCED_FACE('',(#3134),#411,.F.);
#25088=ADVANCED_FACE('',(#3135),#412,.T.);
#25089=ADVANCED_FACE('',(#3136),#39,.T.);
#25090=ADVANCED_FACE('',(#3137),#413,.T.);
#25091=ADVANCED_FACE('',(#3138),#12,.T.);
#25092=ADVANCED_FACE('',(#3139),#414,.T.);
#25093=ADVANCED_FACE('',(#3140),#40,.T.);
#25094=ADVANCED_FACE('',(#3141),#415,.F.);
#25095=ADVANCED_FACE('',(#3142),#416,.T.);
#25096=ADVANCED_FACE('',(#3143),#13,.T.);
#25097=ADVANCED_FACE('',(#3144),#417,.F.);
#25098=ADVANCED_FACE('',(#3145),#418,.F.);
#25099=ADVANCED_FACE('',(#3146),#419,.T.);
#25100=ADVANCED_FACE('',(#3147),#420,.T.);
#25101=ADVANCED_FACE('',(#3148),#41,.T.);
#25102=ADVANCED_FACE('',(#3149),#421,.T.);
#25103=ADVANCED_FACE('',(#3150),#14,.T.);
#25104=ADVANCED_FACE('',(#3151),#422,.F.);
#25105=ADVANCED_FACE('',(#3152),#423,.F.);
#25106=ADVANCED_FACE('',(#3153),#424,.T.);
#25107=ADVANCED_FACE('',(#3154),#42,.T.);
#25108=ADVANCED_FACE('',(#3155),#425,.F.);
#25109=ADVANCED_FACE('',(#3156),#426,.T.);
#25110=ADVANCED_FACE('',(#3157),#43,.T.);
#25111=ADVANCED_FACE('',(#3158),#427,.T.);
#25112=ADVANCED_FACE('',(#3159),#15,.T.);
#25113=ADVANCED_FACE('',(#3160),#428,.T.);
#25114=ADVANCED_FACE('',(#3161),#44,.T.);
#25115=ADVANCED_FACE('',(#3162),#429,.F.);
#25116=ADVANCED_FACE('',(#3163),#430,.T.);
#25117=ADVANCED_FACE('',(#3164),#16,.T.);
#25118=ADVANCED_FACE('',(#3165),#431,.F.);
#25119=ADVANCED_FACE('',(#3166),#432,.F.);
#25120=ADVANCED_FACE('',(#3167),#433,.T.);
#25121=ADVANCED_FACE('',(#3168),#434,.T.);
#25122=ADVANCED_FACE('',(#3169),#45,.T.);
#25123=ADVANCED_FACE('',(#3170),#435,.T.);
#25124=ADVANCED_FACE('',(#3171),#17,.T.);
#25125=ADVANCED_FACE('',(#3172),#436,.F.);
#25126=ADVANCED_FACE('',(#3173),#437,.F.);
#25127=ADVANCED_FACE('',(#3174),#438,.T.);
#25128=ADVANCED_FACE('',(#3175),#46,.T.);
#25129=ADVANCED_FACE('',(#3176),#439,.F.);
#25130=ADVANCED_FACE('',(#3177),#440,.T.);
#25131=ADVANCED_FACE('',(#3178),#47,.T.);
#25132=ADVANCED_FACE('',(#3179),#441,.T.);
#25133=ADVANCED_FACE('',(#3180),#18,.T.);
#25134=ADVANCED_FACE('',(#3181),#442,.T.);
#25135=ADVANCED_FACE('',(#3182),#48,.T.);
#25136=ADVANCED_FACE('',(#3183),#443,.F.);
#25137=ADVANCED_FACE('',(#3184),#444,.T.);
#25138=ADVANCED_FACE('',(#3185),#19,.T.);
#25139=ADVANCED_FACE('',(#3186),#445,.F.);
#25140=ADVANCED_FACE('',(#3187),#446,.F.);
#25141=ADVANCED_FACE('',(#3188),#447,.T.);
#25142=ADVANCED_FACE('',(#3189),#448,.T.);
#25143=ADVANCED_FACE('',(#3190),#49,.T.);
#25144=ADVANCED_FACE('',(#3191),#449,.T.);
#25145=ADVANCED_FACE('',(#3192),#20,.T.);
#25146=ADVANCED_FACE('',(#3193),#450,.F.);
#25147=ADVANCED_FACE('',(#3194),#451,.F.);
#25148=ADVANCED_FACE('',(#3195),#452,.T.);
#25149=ADVANCED_FACE('',(#3196),#50,.T.);
#25150=ADVANCED_FACE('',(#3197),#453,.F.);
#25151=ADVANCED_FACE('',(#3198),#454,.T.);
#25152=ADVANCED_FACE('',(#3199),#51,.T.);
#25153=ADVANCED_FACE('',(#3200),#455,.T.);
#25154=ADVANCED_FACE('',(#3201),#21,.T.);
#25155=ADVANCED_FACE('',(#3202),#456,.T.);
#25156=ADVANCED_FACE('',(#3203),#52,.T.);
#25157=ADVANCED_FACE('',(#3204),#457,.F.);
#25158=ADVANCED_FACE('',(#3205),#458,.T.);
#25159=ADVANCED_FACE('',(#3206),#22,.T.);
#25160=ADVANCED_FACE('',(#3207),#459,.F.);
#25161=ADVANCED_FACE('',(#3208),#460,.F.);
#25162=ADVANCED_FACE('',(#3209),#461,.T.);
#25163=ADVANCED_FACE('',(#3210),#462,.T.);
#25164=ADVANCED_FACE('',(#3211),#53,.T.);
#25165=ADVANCED_FACE('',(#3212),#463,.T.);
#25166=ADVANCED_FACE('',(#3213),#23,.T.);
#25167=ADVANCED_FACE('',(#3214),#464,.F.);
#25168=ADVANCED_FACE('',(#3215),#465,.F.);
#25169=ADVANCED_FACE('',(#3216),#466,.T.);
#25170=ADVANCED_FACE('',(#3217),#54,.T.);
#25171=ADVANCED_FACE('',(#3218),#467,.F.);
#25172=ADVANCED_FACE('',(#3219),#468,.T.);
#25173=ADVANCED_FACE('',(#3220),#55,.T.);
#25174=ADVANCED_FACE('',(#3221),#469,.T.);
#25175=ADVANCED_FACE('',(#3222),#24,.T.);
#25176=ADVANCED_FACE('',(#3223),#470,.T.);
#25177=ADVANCED_FACE('',(#3224),#56,.T.);
#25178=ADVANCED_FACE('',(#3225),#471,.F.);
#25179=ADVANCED_FACE('',(#3226),#472,.T.);
#25180=ADVANCED_FACE('',(#3227),#25,.T.);
#25181=ADVANCED_FACE('',(#3228),#473,.F.);
#25182=ADVANCED_FACE('',(#3229),#474,.F.);
#25183=ADVANCED_FACE('',(#3230),#475,.T.);
#25184=ADVANCED_FACE('',(#3231),#476,.T.);
#25185=ADVANCED_FACE('',(#3232),#57,.T.);
#25186=ADVANCED_FACE('',(#3233),#477,.T.);
#25187=ADVANCED_FACE('',(#3234),#26,.T.);
#25188=ADVANCED_FACE('',(#3235),#478,.F.);
#25189=ADVANCED_FACE('',(#3236),#479,.F.);
#25190=ADVANCED_FACE('',(#3237),#480,.T.);
#25191=ADVANCED_FACE('',(#3238),#58,.T.);
#25192=ADVANCED_FACE('',(#3239),#481,.F.);
#25193=ADVANCED_FACE('',(#3240),#482,.T.);
#25194=ADVANCED_FACE('',(#3241),#59,.T.);
#25195=ADVANCED_FACE('',(#3242),#483,.T.);
#25196=ADVANCED_FACE('',(#3243),#27,.T.);
#25197=ADVANCED_FACE('',(#3244),#484,.T.);
#25198=ADVANCED_FACE('',(#3245),#60,.T.);
#25199=ADVANCED_FACE('',(#3246),#485,.F.);
#25200=ADVANCED_FACE('',(#3247),#486,.T.);
#25201=ADVANCED_FACE('',(#3248),#28,.T.);
#25202=ADVANCED_FACE('',(#3249),#487,.F.);
#25203=ADVANCED_FACE('',(#3250),#488,.T.);
#25204=ADVANCED_FACE('',(#3251),#489,.F.);
#25205=ADVANCED_FACE('',(#3252),#490,.F.);
#25206=ADVANCED_FACE('',(#3253),#29,.T.);
#25207=ADVANCED_FACE('',(#3254),#491,.T.);
#25208=ADVANCED_FACE('',(#3255),#61,.T.);
#25209=ADVANCED_FACE('',(#3256),#492,.T.);
#25210=ADVANCED_FACE('',(#3257),#30,.T.);
#25211=ADVANCED_FACE('',(#3258),#493,.T.);
#25212=ADVANCED_FACE('',(#3259),#62,.T.);
#25213=ADVANCED_FACE('',(#3260),#494,.F.);
#25214=ADVANCED_FACE('',(#3261),#495,.T.);
#25215=ADVANCED_FACE('',(#3262),#31,.T.);
#25216=ADVANCED_FACE('',(#3263),#496,.F.);
#25217=ADVANCED_FACE('',(#3264),#497,.F.);
#25218=ADVANCED_FACE('',(#3265),#498,.T.);
#25219=ADVANCED_FACE('',(#3266),#63,.T.);
#25220=ADVANCED_FACE('',(#3267),#499,.T.);
#25221=ADVANCED_FACE('',(#3268),#64,.T.);
#25222=ADVANCED_FACE('',(#3269),#500,.T.);
#25223=ADVANCED_FACE('',(#3270),#501,.F.);
#25224=ADVANCED_FACE('',(#3271),#502,.F.);
#25225=ADVANCED_FACE('',(#3272),#503,.T.);
#25226=ADVANCED_FACE('',(#3273),#504,.T.);
#25227=ADVANCED_FACE('',(#3274),#65,.T.);
#25228=ADVANCED_FACE('',(#3275),#505,.T.);
#25229=ADVANCED_FACE('',(#3276),#32,.T.);
#25230=ADVANCED_FACE('',(#3277),#506,.F.);
#25231=ADVANCED_FACE('',(#3278),#507,.F.);
#25232=ADVANCED_FACE('',(#3279),#508,.T.);
#25233=ADVANCED_FACE('',(#3280),#66,.T.);
#25234=ADVANCED_FACE('',(#3281),#509,.F.);
#25235=ADVANCED_FACE('',(#3282),#510,.T.);
#25236=ADVANCED_FACE('',(#3283),#67,.T.);
#25237=ADVANCED_FACE('',(#3284),#511,.T.);
#25238=ADVANCED_FACE('',(#3285),#33,.T.);
#25239=ADVANCED_FACE('',(#3286),#512,.T.);
#25240=ADVANCED_FACE('',(#3287),#68,.T.);
#25241=ADVANCED_FACE('',(#3288),#513,.F.);
#25242=ADVANCED_FACE('',(#3289),#514,.T.);
#25243=ADVANCED_FACE('',(#3290),#34,.T.);
#25244=ADVANCED_FACE('',(#3291),#515,.F.);
#25245=ADVANCED_FACE('',(#3292),#516,.F.);
#25246=ADVANCED_FACE('',(#3293),#517,.F.);
#25247=ADVANCED_FACE('',(#3294),#518,.F.);
#25248=ADVANCED_FACE('',(#3295),#519,.F.);
#25249=ADVANCED_FACE('',(#3296),#520,.F.);
#25250=ADVANCED_FACE('',(#3297),#521,.F.);
#25251=ADVANCED_FACE('',(#3298),#522,.F.);
#25252=ADVANCED_FACE('',(#3299),#523,.F.);
#25253=ADVANCED_FACE('',(#3300),#2018,.T.);
#25254=ADVANCED_FACE('',(#3301),#24097,.T.);
#25255=ADVANCED_FACE('',(#3302),#2019,.T.);
#25256=ADVANCED_FACE('',(#3303),#24098,.T.);
#25257=ADVANCED_FACE('',(#3304),#2020,.T.);
#25258=ADVANCED_FACE('',(#3305),#24099,.T.);
#25259=ADVANCED_FACE('',(#3306,#1393,#1394,#1395,#1396,#1397),#2021,.F.);
#25260=ADVANCED_FACE('',(#3307),#24100,.F.);
#25261=ADVANCED_FACE('',(#3308),#2022,.F.);
#25262=ADVANCED_FACE('',(#3309),#24101,.T.);
#25263=ADVANCED_FACE('',(#3310),#2023,.F.);
#25264=ADVANCED_FACE('',(#3311),#24102,.T.);
#25265=ADVANCED_FACE('',(#3312),#2024,.F.);
#25266=ADVANCED_FACE('',(#3313),#24103,.T.);
#25267=ADVANCED_FACE('',(#3314,#1398,#1399,#1400,#1401,#1402),#2025,.T.);
#25268=ADVANCED_FACE('',(#3315,#1403),#2026,.T.);
#25269=ADVANCED_FACE('',(#3316),#2027,.T.);
#25270=ADVANCED_FACE('',(#3317),#24104,.T.);
#25271=ADVANCED_FACE('',(#3318),#2028,.F.);
#25272=ADVANCED_FACE('',(#3319),#2029,.F.);
#25273=ADVANCED_FACE('',(#3320),#2030,.F.);
#25274=ADVANCED_FACE('',(#3321),#2031,.F.);
#25275=ADVANCED_FACE('',(#3322),#2032,.F.);
#25276=ADVANCED_FACE('',(#3323),#2033,.F.);
#25277=ADVANCED_FACE('',(#3324),#2034,.F.);
#25278=ADVANCED_FACE('',(#3325,#1404),#2035,.T.);
#25279=ADVANCED_FACE('',(#3326),#24105,.T.);
#25280=ADVANCED_FACE('',(#3327),#78,.T.);
#25281=ADVANCED_FACE('',(#3328,#1405),#2036,.T.);
#25282=ADVANCED_FACE('',(#3329),#2037,.F.);
#25283=ADVANCED_FACE('',(#3330),#2038,.F.);
#25284=ADVANCED_FACE('',(#3331),#2039,.F.);
#25285=ADVANCED_FACE('',(#3332),#2040,.F.);
#25286=ADVANCED_FACE('',(#3333),#2041,.F.);
#25287=ADVANCED_FACE('',(#3334),#2042,.F.);
#25288=ADVANCED_FACE('',(#3335),#2043,.F.);
#25289=ADVANCED_FACE('',(#3336),#2044,.T.);
#25290=ADVANCED_FACE('',(#3337),#551,.T.);
#25291=ADVANCED_FACE('',(#3338),#24106,.T.);
#25292=ADVANCED_FACE('',(#3339,#1406),#2045,.T.);
#25293=ADVANCED_FACE('',(#3340),#24107,.T.);
#25294=ADVANCED_FACE('',(#3341),#79,.T.);
#25295=ADVANCED_FACE('',(#3342,#1407),#2046,.T.);
#25296=ADVANCED_FACE('',(#3343),#2047,.F.);
#25297=ADVANCED_FACE('',(#3344),#2048,.F.);
#25298=ADVANCED_FACE('',(#3345),#2049,.F.);
#25299=ADVANCED_FACE('',(#3346),#2050,.F.);
#25300=ADVANCED_FACE('',(#3347),#2051,.F.);
#25301=ADVANCED_FACE('',(#3348),#2052,.F.);
#25302=ADVANCED_FACE('',(#3349),#2053,.F.);
#25303=ADVANCED_FACE('',(#3350),#2054,.T.);
#25304=ADVANCED_FACE('',(#3351),#552,.T.);
#25305=ADVANCED_FACE('',(#3352),#24108,.T.);
#25306=ADVANCED_FACE('',(#3353),#2055,.T.);
#25307=ADVANCED_FACE('',(#3354),#553,.T.);
#25308=ADVANCED_FACE('',(#3355),#2056,.T.);
#25309=ADVANCED_FACE('',(#3356),#2057,.T.);
#25310=ADVANCED_FACE('',(#3357),#24109,.F.);
#25311=ADVANCED_FACE('',(#3358),#24110,.F.);
#25312=ADVANCED_FACE('',(#3359),#24111,.F.);
#25313=ADVANCED_FACE('',(#3360),#24112,.F.);
#25314=ADVANCED_FACE('',(#3361),#24113,.F.);
#25315=ADVANCED_FACE('',(#3362),#24114,.F.);
#25316=ADVANCED_FACE('',(#3363,#1408,#1409),#24115,.T.);
#25317=ADVANCED_FACE('',(#3364),#24116,.F.);
#25318=ADVANCED_FACE('',(#3365),#2058,.F.);
#25319=ADVANCED_FACE('',(#3366),#24117,.F.);
#25320=ADVANCED_FACE('',(#3367,#1410),#2059,.F.);
#25321=ADVANCED_FACE('',(#3368),#24118,.F.);
#25322=ADVANCED_FACE('',(#3369,#1411),#2060,.F.);
#25323=ADVANCED_FACE('',(#3370),#24119,.F.);
#25324=ADVANCED_FACE('',(#3371,#1412),#2061,.T.);
#25325=ADVANCED_FACE('',(#3372,#1413),#2062,.T.);
#25326=ADVANCED_FACE('',(#3373),#24120,.F.);
#25327=ADVANCED_FACE('',(#3374),#24121,.F.);
#25328=ADVANCED_FACE('',(#3375,#1414),#2063,.T.);
#25329=ADVANCED_FACE('',(#3376),#24122,.F.);
#25330=ADVANCED_FACE('',(#3377),#24123,.F.);
#25331=ADVANCED_FACE('',(#3378,#1415),#2064,.F.);
#25332=ADVANCED_FACE('',(#3379),#24124,.F.);
#25333=ADVANCED_FACE('',(#3380,#1416),#2065,.F.);
#25334=ADVANCED_FACE('',(#3381,#1417),#2066,.T.);
#25335=ADVANCED_FACE('',(#3382),#2067,.T.);
#25336=ADVANCED_FACE('',(#3383),#554,.T.);
#25337=ADVANCED_FACE('',(#3384),#2068,.F.);
#25338=ADVANCED_FACE('',(#3385),#24125,.F.);
#25339=ADVANCED_FACE('',(#3386),#24126,.F.);
#25340=ADVANCED_FACE('',(#3387),#24127,.T.);
#25341=ADVANCED_FACE('',(#3388),#24128,.F.);
#25342=ADVANCED_FACE('',(#3389),#2069,.T.);
#25343=ADVANCED_FACE('',(#3390),#2070,.T.);
#25344=ADVANCED_FACE('',(#3391),#2071,.F.);
#25345=ADVANCED_FACE('',(#3392),#2072,.F.);
#25346=ADVANCED_FACE('',(#3393),#2073,.T.);
#25347=ADVANCED_FACE('',(#3394),#2074,.T.);
#25348=ADVANCED_FACE('',(#3395),#24129,.F.);
#25349=ADVANCED_FACE('',(#3396),#24130,.F.);
#25350=ADVANCED_FACE('',(#3397),#24131,.F.);
#25351=ADVANCED_FACE('',(#3398),#24132,.F.);
#25352=ADVANCED_FACE('',(#3399),#24133,.F.);
#25353=ADVANCED_FACE('',(#3400),#24134,.F.);
#25354=ADVANCED_FACE('',(#3401),#2075,.T.);
#25355=ADVANCED_FACE('',(#3402),#2076,.T.);
#25356=ADVANCED_FACE('',(#3403,#1418,#1419,#1420,#1421,#1422,#1423,#1424,
#1425),#24135,.T.);
#25357=ADVANCED_FACE('',(#3404),#24136,.T.);
#25358=ADVANCED_FACE('',(#3405),#2077,.F.);
#25359=ADVANCED_FACE('',(#3406),#2078,.F.);
#25360=ADVANCED_FACE('',(#3407),#2079,.F.);
#25361=ADVANCED_FACE('',(#3408),#2080,.F.);
#25362=ADVANCED_FACE('',(#3409),#2081,.F.);
#25363=ADVANCED_FACE('',(#3410),#2082,.F.);
#25364=ADVANCED_FACE('',(#3411),#2083,.F.);
#25365=ADVANCED_FACE('',(#3412),#2084,.F.);
#25366=ADVANCED_FACE('',(#3413),#2085,.F.);
#25367=ADVANCED_FACE('',(#3414),#2086,.F.);
#25368=ADVANCED_FACE('',(#3415),#2087,.F.);
#25369=ADVANCED_FACE('',(#3416),#2088,.F.);
#25370=ADVANCED_FACE('',(#3417),#2089,.F.);
#25371=ADVANCED_FACE('',(#3418),#2090,.F.);
#25372=ADVANCED_FACE('',(#3419),#2091,.F.);
#25373=ADVANCED_FACE('',(#3420),#2092,.F.);
#25374=ADVANCED_FACE('',(#3421),#2093,.F.);
#25375=ADVANCED_FACE('',(#3422),#2094,.F.);
#25376=ADVANCED_FACE('',(#3423),#2095,.F.);
#25377=ADVANCED_FACE('',(#3424),#24137,.T.);
#25378=ADVANCED_FACE('',(#3425),#24138,.T.);
#25379=ADVANCED_FACE('',(#3426),#2096,.F.);
#25380=ADVANCED_FACE('',(#3427),#2097,.F.);
#25381=ADVANCED_FACE('',(#3428),#2098,.F.);
#25382=ADVANCED_FACE('',(#3429),#2099,.F.);
#25383=ADVANCED_FACE('',(#3430),#2100,.F.);
#25384=ADVANCED_FACE('',(#3431),#2101,.F.);
#25385=ADVANCED_FACE('',(#3432),#2102,.F.);
#25386=ADVANCED_FACE('',(#3433),#2103,.F.);
#25387=ADVANCED_FACE('',(#3434),#2104,.F.);
#25388=ADVANCED_FACE('',(#3435),#2105,.F.);
#25389=ADVANCED_FACE('',(#3436),#2106,.F.);
#25390=ADVANCED_FACE('',(#3437),#2107,.F.);
#25391=ADVANCED_FACE('',(#3438),#24139,.T.);
#25392=ADVANCED_FACE('',(#3439),#2108,.F.);
#25393=ADVANCED_FACE('',(#3440),#2109,.F.);
#25394=ADVANCED_FACE('',(#3441),#2110,.F.);
#25395=ADVANCED_FACE('',(#3442),#24140,.F.);
#25396=ADVANCED_FACE('',(#3443),#2111,.F.);
#25397=ADVANCED_FACE('',(#3444),#2112,.T.);
#25398=ADVANCED_FACE('',(#3445),#2113,.T.);
#25399=ADVANCED_FACE('',(#3446),#2114,.F.);
#25400=ADVANCED_FACE('',(#3447),#2115,.F.);
#25401=ADVANCED_FACE('',(#3448),#2116,.F.);
#25402=ADVANCED_FACE('',(#3449),#2117,.F.);
#25403=ADVANCED_FACE('',(#3450),#24141,.T.);
#25404=ADVANCED_FACE('',(#3451),#2118,.T.);
#25405=ADVANCED_FACE('',(#3452,#1426),#24142,.T.);
#25406=ADVANCED_FACE('',(#3453,#1427),#2119,.T.);
#25407=ADVANCED_FACE('',(#3454),#2120,.T.);
#25408=ADVANCED_FACE('',(#3455),#24143,.T.);
#25409=ADVANCED_FACE('',(#3456),#2121,.F.);
#25410=ADVANCED_FACE('',(#3457),#2122,.F.);
#25411=ADVANCED_FACE('',(#3458),#2123,.F.);
#25412=ADVANCED_FACE('',(#3459),#2124,.F.);
#25413=ADVANCED_FACE('',(#3460),#2125,.F.);
#25414=ADVANCED_FACE('',(#3461),#2126,.F.);
#25415=ADVANCED_FACE('',(#3462),#2127,.F.);
#25416=ADVANCED_FACE('',(#3463,#1428),#2128,.T.);
#25417=ADVANCED_FACE('',(#3464),#24144,.T.);
#25418=ADVANCED_FACE('',(#3465),#80,.T.);
#25419=ADVANCED_FACE('',(#3466,#1429),#2129,.T.);
#25420=ADVANCED_FACE('',(#3467),#2130,.F.);
#25421=ADVANCED_FACE('',(#3468),#2131,.F.);
#25422=ADVANCED_FACE('',(#3469),#2132,.F.);
#25423=ADVANCED_FACE('',(#3470),#2133,.F.);
#25424=ADVANCED_FACE('',(#3471),#2134,.F.);
#25425=ADVANCED_FACE('',(#3472),#2135,.F.);
#25426=ADVANCED_FACE('',(#3473),#2136,.F.);
#25427=ADVANCED_FACE('',(#3474),#2137,.T.);
#25428=ADVANCED_FACE('',(#3475),#555,.T.);
#25429=ADVANCED_FACE('',(#3476),#24145,.T.);
#25430=ADVANCED_FACE('',(#3477,#1430),#2138,.T.);
#25431=ADVANCED_FACE('',(#3478),#24146,.T.);
#25432=ADVANCED_FACE('',(#3479),#81,.T.);
#25433=ADVANCED_FACE('',(#3480,#1431),#2139,.T.);
#25434=ADVANCED_FACE('',(#3481),#2140,.F.);
#25435=ADVANCED_FACE('',(#3482),#2141,.F.);
#25436=ADVANCED_FACE('',(#3483),#2142,.F.);
#25437=ADVANCED_FACE('',(#3484),#2143,.F.);
#25438=ADVANCED_FACE('',(#3485),#2144,.F.);
#25439=ADVANCED_FACE('',(#3486),#2145,.F.);
#25440=ADVANCED_FACE('',(#3487),#2146,.F.);
#25441=ADVANCED_FACE('',(#3488),#2147,.T.);
#25442=ADVANCED_FACE('',(#3489),#556,.T.);
#25443=ADVANCED_FACE('',(#3490),#24147,.T.);
#25444=ADVANCED_FACE('',(#3491),#2148,.T.);
#25445=ADVANCED_FACE('',(#3492),#557,.T.);
#25446=ADVANCED_FACE('',(#3493),#2149,.T.);
#25447=ADVANCED_FACE('',(#3494),#2150,.T.);
#25448=ADVANCED_FACE('',(#3495),#24148,.F.);
#25449=ADVANCED_FACE('',(#3496),#24149,.F.);
#25450=ADVANCED_FACE('',(#3497),#24150,.F.);
#25451=ADVANCED_FACE('',(#3498),#24151,.F.);
#25452=ADVANCED_FACE('',(#3499),#24152,.F.);
#25453=ADVANCED_FACE('',(#3500),#24153,.F.);
#25454=ADVANCED_FACE('',(#3501,#1432,#1433),#24154,.T.);
#25455=ADVANCED_FACE('',(#3502),#24155,.F.);
#25456=ADVANCED_FACE('',(#3503),#2151,.F.);
#25457=ADVANCED_FACE('',(#3504),#24156,.F.);
#25458=ADVANCED_FACE('',(#3505,#1434),#2152,.F.);
#25459=ADVANCED_FACE('',(#3506),#24157,.F.);
#25460=ADVANCED_FACE('',(#3507,#1435),#2153,.F.);
#25461=ADVANCED_FACE('',(#3508),#24158,.F.);
#25462=ADVANCED_FACE('',(#3509,#1436),#2154,.T.);
#25463=ADVANCED_FACE('',(#3510,#1437),#2155,.T.);
#25464=ADVANCED_FACE('',(#3511),#24159,.F.);
#25465=ADVANCED_FACE('',(#3512),#24160,.F.);
#25466=ADVANCED_FACE('',(#3513,#1438),#2156,.T.);
#25467=ADVANCED_FACE('',(#3514),#24161,.F.);
#25468=ADVANCED_FACE('',(#3515),#24162,.F.);
#25469=ADVANCED_FACE('',(#3516,#1439),#2157,.F.);
#25470=ADVANCED_FACE('',(#3517),#24163,.F.);
#25471=ADVANCED_FACE('',(#3518,#1440),#2158,.F.);
#25472=ADVANCED_FACE('',(#3519,#1441),#2159,.T.);
#25473=ADVANCED_FACE('',(#3520),#2160,.T.);
#25474=ADVANCED_FACE('',(#3521),#558,.T.);
#25475=ADVANCED_FACE('',(#3522),#2161,.F.);
#25476=ADVANCED_FACE('',(#3523),#24164,.F.);
#25477=ADVANCED_FACE('',(#3524),#24165,.F.);
#25478=ADVANCED_FACE('',(#3525),#24166,.T.);
#25479=ADVANCED_FACE('',(#3526),#24167,.F.);
#25480=ADVANCED_FACE('',(#3527),#2162,.T.);
#25481=ADVANCED_FACE('',(#3528),#2163,.T.);
#25482=ADVANCED_FACE('',(#3529,#1442),#2164,.F.);
#25483=ADVANCED_FACE('',(#3530),#24168,.F.);
#25484=ADVANCED_FACE('',(#3531),#24169,.F.);
#25485=ADVANCED_FACE('',(#3532),#24170,.F.);
#25486=ADVANCED_FACE('',(#3533),#24171,.F.);
#25487=ADVANCED_FACE('',(#3534),#24172,.F.);
#25488=ADVANCED_FACE('',(#3535),#24173,.F.);
#25489=ADVANCED_FACE('',(#3536),#2165,.T.);
#25490=ADVANCED_FACE('',(#3537),#2166,.T.);
#25491=ADVANCED_FACE('',(#3538,#1443,#1444,#1445,#1446,#1447,#1448,#1449,
#1450),#24174,.T.);
#25492=ADVANCED_FACE('',(#3539),#24175,.T.);
#25493=ADVANCED_FACE('',(#3540),#2167,.F.);
#25494=ADVANCED_FACE('',(#3541),#2168,.F.);
#25495=ADVANCED_FACE('',(#3542),#2169,.F.);
#25496=ADVANCED_FACE('',(#3543),#2170,.F.);
#25497=ADVANCED_FACE('',(#3544),#2171,.F.);
#25498=ADVANCED_FACE('',(#3545),#2172,.F.);
#25499=ADVANCED_FACE('',(#3546),#2173,.F.);
#25500=ADVANCED_FACE('',(#3547),#2174,.F.);
#25501=ADVANCED_FACE('',(#3548),#2175,.F.);
#25502=ADVANCED_FACE('',(#3549),#2176,.F.);
#25503=ADVANCED_FACE('',(#3550),#2177,.F.);
#25504=ADVANCED_FACE('',(#3551),#2178,.F.);
#25505=ADVANCED_FACE('',(#3552),#2179,.F.);
#25506=ADVANCED_FACE('',(#3553),#2180,.F.);
#25507=ADVANCED_FACE('',(#3554),#2181,.F.);
#25508=ADVANCED_FACE('',(#3555),#2182,.F.);
#25509=ADVANCED_FACE('',(#3556),#2183,.F.);
#25510=ADVANCED_FACE('',(#3557),#2184,.F.);
#25511=ADVANCED_FACE('',(#3558),#2185,.F.);
#25512=ADVANCED_FACE('',(#3559),#24176,.T.);
#25513=ADVANCED_FACE('',(#3560),#24177,.T.);
#25514=ADVANCED_FACE('',(#3561),#2186,.F.);
#25515=ADVANCED_FACE('',(#3562),#2187,.F.);
#25516=ADVANCED_FACE('',(#3563),#2188,.F.);
#25517=ADVANCED_FACE('',(#3564),#2189,.F.);
#25518=ADVANCED_FACE('',(#3565),#2190,.F.);
#25519=ADVANCED_FACE('',(#3566),#2191,.F.);
#25520=ADVANCED_FACE('',(#3567),#2192,.F.);
#25521=ADVANCED_FACE('',(#3568),#2193,.F.);
#25522=ADVANCED_FACE('',(#3569),#2194,.F.);
#25523=ADVANCED_FACE('',(#3570),#2195,.F.);
#25524=ADVANCED_FACE('',(#3571),#2196,.F.);
#25525=ADVANCED_FACE('',(#3572),#2197,.F.);
#25526=ADVANCED_FACE('',(#3573),#24178,.T.);
#25527=ADVANCED_FACE('',(#3574),#2198,.F.);
#25528=ADVANCED_FACE('',(#3575),#2199,.F.);
#25529=ADVANCED_FACE('',(#3576),#2200,.F.);
#25530=ADVANCED_FACE('',(#3577),#24179,.F.);
#25531=ADVANCED_FACE('',(#3578),#2201,.F.);
#25532=ADVANCED_FACE('',(#3579),#2202,.T.);
#25533=ADVANCED_FACE('',(#3580),#2203,.T.);
#25534=ADVANCED_FACE('',(#3581),#2204,.F.);
#25535=ADVANCED_FACE('',(#3582),#2205,.F.);
#25536=ADVANCED_FACE('',(#3583),#2206,.F.);
#25537=ADVANCED_FACE('',(#3584),#2207,.F.);
#25538=ADVANCED_FACE('',(#3585),#24180,.T.);
#25539=ADVANCED_FACE('',(#3586),#2208,.T.);
#25540=ADVANCED_FACE('',(#3587,#1451),#24181,.T.);
#25541=ADVANCED_FACE('',(#3588),#24182,.F.);
#25542=ADVANCED_FACE('',(#3589),#559,.F.);
#25543=ADVANCED_FACE('',(#3590),#24183,.F.);
#25544=ADVANCED_FACE('',(#3591),#560,.F.);
#25545=ADVANCED_FACE('',(#3592),#24184,.F.);
#25546=ADVANCED_FACE('',(#3593),#561,.F.);
#25547=ADVANCED_FACE('',(#3594),#24185,.F.);
#25548=ADVANCED_FACE('',(#3595),#562,.F.);
#25549=ADVANCED_FACE('',(#3596),#24186,.F.);
#25550=ADVANCED_FACE('',(#3597),#563,.F.);
#25551=ADVANCED_FACE('',(#3598),#24187,.F.);
#25552=ADVANCED_FACE('',(#3599),#564,.F.);
#25553=ADVANCED_FACE('',(#3600),#24188,.F.);
#25554=ADVANCED_FACE('',(#3601),#565,.F.);
#25555=ADVANCED_FACE('',(#3602),#24189,.F.);
#25556=ADVANCED_FACE('',(#3603),#566,.F.);
#25557=ADVANCED_FACE('',(#3604),#24190,.F.);
#25558=ADVANCED_FACE('',(#3605),#567,.F.);
#25559=ADVANCED_FACE('',(#3606),#24191,.F.);
#25560=ADVANCED_FACE('',(#3607),#568,.F.);
#25561=ADVANCED_FACE('',(#3608),#24192,.F.);
#25562=ADVANCED_FACE('',(#3609),#569,.F.);
#25563=ADVANCED_FACE('',(#3610),#24193,.F.);
#25564=ADVANCED_FACE('',(#3611),#570,.F.);
#25565=ADVANCED_FACE('',(#3612),#24194,.F.);
#25566=ADVANCED_FACE('',(#3613),#571,.F.);
#25567=ADVANCED_FACE('',(#3614),#24195,.F.);
#25568=ADVANCED_FACE('',(#3615),#572,.F.);
#25569=ADVANCED_FACE('',(#3616),#24196,.F.);
#25570=ADVANCED_FACE('',(#3617),#573,.F.);
#25571=ADVANCED_FACE('',(#3618),#24197,.F.);
#25572=ADVANCED_FACE('',(#3619),#574,.F.);
#25573=ADVANCED_FACE('',(#3620),#24198,.F.);
#25574=ADVANCED_FACE('',(#3621),#575,.F.);
#25575=ADVANCED_FACE('',(#3622),#2209,.F.);
#25576=ADVANCED_FACE('',(#3623),#2210,.F.);
#25577=ADVANCED_FACE('',(#3624),#2211,.F.);
#25578=ADVANCED_FACE('',(#3625),#2212,.F.);
#25579=ADVANCED_FACE('',(#3626),#2213,.F.);
#25580=ADVANCED_FACE('',(#3627),#2214,.T.);
#25581=ADVANCED_FACE('',(#3628),#2215,.F.);
#25582=ADVANCED_FACE('',(#3629),#2216,.F.);
#25583=ADVANCED_FACE('',(#3630,#1452,#1453,#1454,#1455,#1456,#1457,#1458,
#1459,#1460,#1461,#1462,#1463,#1464,#1465,#1466,#1467,#1468),#2217,.F.);
#25584=ADVANCED_FACE('',(#3631),#2218,.F.);
#25585=ADVANCED_FACE('',(#3632),#24199,.F.);
#25586=ADVANCED_FACE('',(#3633),#24200,.F.);
#25587=ADVANCED_FACE('',(#3634),#24201,.T.);
#25588=ADVANCED_FACE('',(#3635),#576,.T.);
#25589=ADVANCED_FACE('',(#3636),#577,.T.);
#25590=ADVANCED_FACE('',(#3637),#24202,.T.);
#25591=ADVANCED_FACE('',(#3638),#2219,.T.);
#25592=ADVANCED_FACE('',(#3639,#1469),#2220,.T.);
#25593=ADVANCED_FACE('',(#3640,#1470),#2221,.T.);
#25594=ADVANCED_FACE('',(#3641),#2222,.F.);
#25595=ADVANCED_FACE('',(#3642),#2223,.F.);
#25596=ADVANCED_FACE('',(#3643),#2224,.F.);
#25597=ADVANCED_FACE('',(#3644),#2225,.F.);
#25598=ADVANCED_FACE('',(#3645),#2226,.F.);
#25599=ADVANCED_FACE('',(#3646),#2227,.F.);
#25600=ADVANCED_FACE('',(#3647),#2228,.T.);
#25601=ADVANCED_FACE('',(#3648),#578,.T.);
#25602=ADVANCED_FACE('',(#3649),#579,.F.);
#25603=ADVANCED_FACE('',(#3650),#24203,.T.);
#25604=ADVANCED_FACE('',(#3651),#24204,.T.);
#25605=ADVANCED_FACE('',(#3652),#24205,.T.);
#25606=ADVANCED_FACE('',(#3653,#1471),#2229,.F.);
#25607=ADVANCED_FACE('',(#3654),#2230,.F.);
#25608=ADVANCED_FACE('',(#3655,#1472),#2231,.F.);
#25609=ADVANCED_FACE('',(#3656,#1473),#2232,.F.);
#25610=ADVANCED_FACE('',(#3657),#2233,.F.);
#25611=ADVANCED_FACE('',(#3658),#2234,.F.);
#25612=ADVANCED_FACE('',(#3659),#2235,.F.);
#25613=ADVANCED_FACE('',(#3660),#2236,.F.);
#25614=ADVANCED_FACE('',(#3661),#2237,.F.);
#25615=ADVANCED_FACE('',(#3662),#2238,.F.);
#25616=ADVANCED_FACE('',(#3663),#2239,.T.);
#25617=ADVANCED_FACE('',(#3664),#2240,.T.);
#25618=ADVANCED_FACE('',(#3665),#2241,.T.);
#25619=ADVANCED_FACE('',(#3666),#2242,.T.);
#25620=ADVANCED_FACE('',(#3667),#2243,.T.);
#25621=ADVANCED_FACE('',(#3668),#2244,.T.);
#25622=ADVANCED_FACE('',(#3669),#24206,.T.);
#25623=ADVANCED_FACE('',(#3670),#24207,.F.);
#25624=ADVANCED_FACE('',(#3671,#1474),#2245,.F.);
#25625=ADVANCED_FACE('',(#3672,#1475),#2246,.F.);
#25626=ADVANCED_FACE('',(#3673),#24208,.T.);
#25627=ADVANCED_FACE('',(#3674),#24209,.F.);
#25628=ADVANCED_FACE('',(#3675),#2247,.F.);
#25629=ADVANCED_FACE('',(#3676),#2248,.F.);
#25630=ADVANCED_FACE('',(#3677),#2249,.F.);
#25631=ADVANCED_FACE('',(#3678),#2250,.F.);
#25632=ADVANCED_FACE('',(#3679),#24210,.F.);
#25633=ADVANCED_FACE('',(#3680),#24211,.F.);
#25634=ADVANCED_FACE('',(#3681),#24212,.F.);
#25635=ADVANCED_FACE('',(#3682),#24213,.F.);
#25636=ADVANCED_FACE('',(#3683),#24214,.F.);
#25637=ADVANCED_FACE('',(#3684),#24215,.F.);
#25638=ADVANCED_FACE('',(#3685),#24216,.F.);
#25639=ADVANCED_FACE('',(#3686),#24217,.F.);
#25640=ADVANCED_FACE('',(#3687),#24218,.F.);
#25641=ADVANCED_FACE('',(#3688),#24219,.F.);
#25642=ADVANCED_FACE('',(#3689,#1476,#1477,#1478,#1479,#1480,#1481,#1482,
#1483,#1484,#1485),#2251,.F.);
#25643=ADVANCED_FACE('',(#3690),#2252,.F.);
#25644=ADVANCED_FACE('',(#3691),#2253,.F.);
#25645=ADVANCED_FACE('',(#3692),#2254,.F.);
#25646=ADVANCED_FACE('',(#3693),#2255,.F.);
#25647=ADVANCED_FACE('',(#3694,#1486,#1487,#1488,#1489,#1490,#1491,#1492,
#1493,#1494,#1495),#2256,.T.);
#25648=ADVANCED_FACE('',(#3695),#2257,.T.);
#25649=ADVANCED_FACE('',(#3696),#2258,.T.);
#25650=ADVANCED_FACE('',(#3697),#24220,.T.);
#25651=ADVANCED_FACE('',(#3698),#580,.T.);
#25652=ADVANCED_FACE('',(#3699),#581,.T.);
#25653=ADVANCED_FACE('',(#3700),#24221,.T.);
#25654=ADVANCED_FACE('',(#3701),#2259,.T.);
#25655=ADVANCED_FACE('',(#3702,#1496),#2260,.T.);
#25656=ADVANCED_FACE('',(#3703,#1497),#2261,.T.);
#25657=ADVANCED_FACE('',(#3704),#2262,.F.);
#25658=ADVANCED_FACE('',(#3705),#2263,.F.);
#25659=ADVANCED_FACE('',(#3706),#2264,.F.);
#25660=ADVANCED_FACE('',(#3707),#2265,.F.);
#25661=ADVANCED_FACE('',(#3708),#2266,.F.);
#25662=ADVANCED_FACE('',(#3709),#2267,.F.);
#25663=ADVANCED_FACE('',(#3710),#2268,.T.);
#25664=CLOSED_SHELL('',(#24222,#24223,#24224,#24225,#24226,#24227,#24228,
#24229,#24230,#24231,#24232,#24233,#24234,#24235,#24236,#24237,#24238,#24239));
#25665=CLOSED_SHELL('',(#24240,#24241,#24242,#24243,#24244,#24245,#24246,
#24247,#24248,#24249,#24250,#24251,#24252,#24253,#24254,#24255));
#25666=CLOSED_SHELL('',(#24256,#24257,#24258,#24259,#24260,#24261,#24262,
#24263,#24264,#24265,#24266,#24267,#24268,#24269,#24270,#24271,#24272,#24273,
#24274,#24275,#24276));
#25667=CLOSED_SHELL('',(#24277,#24278,#24279,#24280,#24281,#24282,#24283,
#24284,#24285,#24286,#24287,#24288,#24289,#24290,#24291));
#25668=CLOSED_SHELL('',(#24292,#24293,#24294,#24295,#24296,#24297,#24298,
#24299,#24300,#24301,#24302,#24303));
#25669=CLOSED_SHELL('',(#24304,#24305,#24306,#24307,#24308,#24309,#24310,
#24311,#24312,#24313,#24314,#24315));
#25670=CLOSED_SHELL('',(#24316,#24317,#24318,#24319,#24320,#24321,#24322,
#24323,#24324,#24325,#24326,#24327,#24328,#24329,#24330,#24331,#24332,#24333,
#24334,#24335,#24336,#24337,#24338,#24339,#24340,#24341,#24342,#24343,#24344,
#24345,#24346,#24347,#24348,#24349,#24350,#24351,#24352,#24353,#24354,#24355,
#24356,#24357,#24358,#24359,#24360,#24361,#24362,#24363,#24364,#24365,#24366,
#24367,#24368,#24369,#24370,#24371,#24372,#24373,#24374,#24375,#24376,#24377,
#24378,#24379,#24380,#24381,#24382,#24383,#24384,#24385,#24386,#24387,#24388,
#24389,#24390,#24391,#24392,#24393,#24394,#24395,#24396,#24397,#24398,#24399,
#24400,#24401,#24402,#24403,#24404,#24405,#24406,#24407,#24408,#24409,#24410,
#24411,#24412,#24413,#24414,#24415,#24416,#24417,#24418,#24419,#24420,#24421,
#24422,#24423,#24424,#24425,#24426,#24427,#24428,#24429,#24430,#24431,#24432,
#24433,#24434,#24435,#24436,#24437,#24438,#24439,#24440,#24441,#24442,#24443,
#24444,#24445,#24446,#24447,#24448,#24449,#24450,#24451,#24452,#24453));
#25671=CLOSED_SHELL('',(#24454,#24455,#24456,#24457,#24458,#24459,#24460,
#24461,#24462,#24463,#24464,#24465,#24466,#24467,#24468,#24469,#24470,#24471,
#24472,#24473,#24474,#24475,#24476,#24477,#24478,#24479,#24480,#24481,#24482,
#24483,#24484,#24485,#24486,#24487,#24488,#24489,#24490,#24491,#24492,#24493,
#24494,#24495,#24496,#24497,#24498,#24499,#24500,#24501,#24502,#24503,#24504,
#24505,#24506,#24507,#24508,#24509,#24510,#24511,#24512,#24513,#24514,#24515,
#24516,#24517,#24518,#24519,#24520,#24521,#24522,#24523,#24524,#24525,#24526,
#24527,#24528,#24529,#24530,#24531,#24532,#24533,#24534,#24535,#24536,#24537,
#24538,#24539,#24540,#24541,#24542,#24543,#24544,#24545,#24546,#24547,#24548,
#24549,#24550,#24551,#24552,#24553,#24554,#24555,#24556,#24557,#24558,#24559,
#24560,#24561,#24562,#24563,#24564,#24565,#24566,#24567,#24568,#24569,#24570,
#24571,#24572,#24573,#24574,#24575,#24576,#24577,#24578,#24579,#24580,#24581,
#24582,#24583,#24584,#24585,#24586,#24587,#24588,#24589,#24590,#24591,#24592,
#24593,#24594,#24595,#24596,#24597,#24598,#24599,#24600,#24601,#24602,#24603,
#24604,#24605,#24606,#24607,#24608,#24609,#24610,#24611,#24612,#24613,#24614,
#24615,#24616,#24617,#24618,#24619,#24620,#24621,#24622,#24623,#24624,#24625,
#24626,#24627,#24628,#24629,#24630,#24631,#24632,#24633,#24634,#24635,#24636,
#24637,#24638,#24639,#24640,#24641,#24642,#24643,#24644,#24645,#24646,#24647,
#24648,#24649,#24650,#24651,#24652,#24653,#24654,#24655,#24656,#24657,#24658,
#24659,#24660,#24661,#24662,#24663,#24664,#24665,#24666,#24667,#24668,#24669,
#24670,#24671,#24672,#24673,#24674,#24675,#24676,#24677,#24678,#24679,#24680,
#24681,#24682,#24683,#24684,#24685,#24686,#24687,#24688,#24689,#24690,#24691,
#24692,#24693,#24694,#24695,#24696,#24697,#24698,#24699,#24700,#24701,#24702,
#24703,#24704,#24705,#24706,#24707,#24708,#24709,#24710,#24711,#24712,#24713,
#24714,#24715,#24716,#24717,#24718,#24719,#24720,#24721,#24722,#24723,#24724,
#24725,#24726,#24727,#24728,#24729,#24730,#24731,#24732,#24733,#24734,#24735,
#24736,#24737,#24738,#24739,#24740,#24741,#24742,#24743,#24744,#24745,#24746,
#24747,#24748,#24749,#24750,#24751,#24752,#24753,#24754,#24755,#24756,#24757,
#24758,#24759,#24760,#24761,#24762,#24763,#24764,#24765,#24766,#24767,#24768,
#24769,#24770,#24771,#24772,#24773,#24774,#24775,#24776,#24777,#24778,#24779,
#24780,#24781,#24782,#24783,#24784,#24785,#24786,#24787,#24788,#24789,#24790,
#24791,#24792));
#25672=CLOSED_SHELL('',(#24793,#24794,#24795,#24796,#24797,#24798,#24799,
#24800,#24801,#24802,#24803,#24804,#24805,#24806,#24807,#24808,#24809,#24810,
#24811,#24812,#24813,#24814,#24815,#24816,#24817,#24818,#24819,#24820,#24821,
#24822,#24823,#24824,#24825,#24826,#24827,#24828,#24829,#24830,#24831,#24832,
#24833));
#25673=CLOSED_SHELL('',(#24834,#24835,#24836,#24837,#24838,#24839,#24840,
#24841,#24842,#24843,#24844,#24845,#24846,#24847,#24848,#24849,#24850,#24851,
#24852,#24853,#24854,#24855,#24856,#24857,#24858));
#25674=CLOSED_SHELL('',(#24859,#24860,#24861,#24862,#24863,#24864,#24865,
#24866,#24867,#24868,#24869,#24870,#24871,#24872,#24873,#24874,#24875,#24876,
#24877,#24878,#24879,#24880,#24881,#24882,#24883,#24884,#24885,#24886,#24887));
#25675=CLOSED_SHELL('',(#24888,#24889,#24890,#24891,#24892,#24893,#24894,
#24895,#24896,#24897,#24898,#24899,#24900,#24901,#24902,#24903,#24904,#24905,
#24906,#24907,#24908,#24909,#24910,#24911,#24912));
#25676=CLOSED_SHELL('',(#24913,#24914,#24915,#24916,#24917,#24918,#24919,
#24920,#24921,#24922,#24923,#24924,#24925,#24926,#24927,#24928));
#25677=CLOSED_SHELL('',(#24929,#24930,#24931,#24932,#24933,#24934,#24935,
#24936,#24937,#24938,#24939,#24940,#24941,#24942,#24943,#24944,#24945,#24946,
#24947,#24948,#24949,#24950,#24951,#24952,#24953,#24954,#24955,#24956,#24957,
#24958,#24959,#24960,#24961,#24962,#24963,#24964,#24965,#24966,#24967,#24968,
#24969,#24970,#24971,#24972,#24973,#24974,#24975,#24976,#24977,#24978,#24979,
#24980,#24981,#24982,#24983,#24984,#24985,#24986,#24987,#24988,#24989,#24990,
#24991,#24992,#24993,#24994,#24995,#24996,#24997,#24998,#24999,#25000,#25001,
#25002,#25003,#25004,#25005,#25006,#25007,#25008,#25009,#25010,#25011,#25012,
#25013,#25014,#25015,#25016));
#25678=CLOSED_SHELL('',(#25017,#25018,#25019,#25020,#25021,#25022,#25023,
#25024,#25025,#25026,#25027,#25028,#25029,#25030,#25031,#25032,#25033,#25034,
#25035,#25036,#25037,#25038,#25039,#25040,#25041,#25042,#25043,#25044,#25045,
#25046,#25047,#25048,#25049,#25050));
#25679=CLOSED_SHELL('',(#25051,#25052,#25053,#25054));
#25680=CLOSED_SHELL('',(#25055,#25056,#25057,#25058,#25059,#25060,#25061,
#25062,#25063,#25064,#25065,#25066,#25067,#25068,#25069,#25070,#25071,#25072));
#25681=CLOSED_SHELL('',(#25073,#25074,#25075,#25076,#25077,#25078,#25079,
#25080,#25081,#25082,#25083,#25084,#25085,#25086,#25087,#25088,#25089,#25090,
#25091,#25092,#25093,#25094,#25095,#25096,#25097,#25098,#25099,#25100,#25101,
#25102,#25103,#25104,#25105,#25106,#25107,#25108,#25109,#25110,#25111,#25112,
#25113,#25114,#25115,#25116,#25117,#25118,#25119,#25120,#25121,#25122,#25123,
#25124,#25125,#25126,#25127,#25128,#25129,#25130,#25131,#25132,#25133,#25134,
#25135,#25136,#25137,#25138,#25139,#25140,#25141,#25142,#25143,#25144,#25145,
#25146,#25147,#25148,#25149,#25150,#25151,#25152,#25153,#25154,#25155,#25156,
#25157,#25158,#25159,#25160,#25161,#25162,#25163,#25164,#25165,#25166,#25167,
#25168,#25169,#25170,#25171,#25172,#25173,#25174,#25175,#25176,#25177,#25178,
#25179,#25180,#25181,#25182,#25183,#25184,#25185,#25186,#25187,#25188,#25189,
#25190,#25191,#25192,#25193,#25194,#25195,#25196,#25197,#25198,#25199,#25200,
#25201,#25202,#25203,#25204,#25205,#25206,#25207,#25208,#25209,#25210,#25211,
#25212,#25213,#25214,#25215,#25216,#25217,#25218,#25219,#25220,#25221,#25222,
#25223,#25224,#25225,#25226,#25227,#25228,#25229,#25230,#25231,#25232,#25233,
#25234,#25235,#25236,#25237,#25238,#25239,#25240,#25241,#25242,#25243,#25244,
#25245,#25246,#25247,#25248,#25249,#25250,#25251,#25252,#25253,#25254,#25255,
#25256,#25257,#25258,#25259,#25260,#25261,#25262,#25263,#25264,#25265,#25266,
#25267));
#25682=CLOSED_SHELL('',(#25268,#25269,#25270,#25271,#25272,#25273,#25274,
#25275,#25276,#25277));
#25683=CLOSED_SHELL('',(#25278,#25279,#25280,#25281,#25282,#25283,#25284,
#25285,#25286,#25287,#25288,#25289,#25290,#25291));
#25684=CLOSED_SHELL('',(#25292,#25293,#25294,#25295,#25296,#25297,#25298,
#25299,#25300,#25301,#25302,#25303,#25304,#25305));
#25685=CLOSED_SHELL('',(#25306,#25307,#25308,#25309,#25310,#25311,#25312,
#25313,#25314,#25315,#25316,#25317,#25318,#25319,#25320,#25321,#25322,#25323,
#25324,#25325,#25326));
#25686=CLOSED_SHELL('',(#25327,#25328,#25329,#25330,#25331,#25332,#25333,
#25334,#25335,#25336,#25337,#25338,#25339,#25340,#25341,#25342,#25343,#25344,
#25345,#25346,#25347,#25348,#25349,#25350,#25351,#25352,#25353,#25354,#25355,
#25356,#25357,#25358,#25359,#25360,#25361,#25362,#25363,#25364,#25365,#25366,
#25367,#25368,#25369,#25370,#25371,#25372,#25373,#25374,#25375,#25376,#25377,
#25378,#25379,#25380,#25381,#25382,#25383,#25384,#25385,#25386,#25387,#25388,
#25389,#25390,#25391,#25392,#25393,#25394,#25395,#25396,#25397,#25398,#25399,
#25400,#25401,#25402,#25403,#25404,#25405));
#25687=CLOSED_SHELL('',(#25406,#25407,#25408,#25409,#25410,#25411,#25412,
#25413,#25414,#25415));
#25688=CLOSED_SHELL('',(#25416,#25417,#25418,#25419,#25420,#25421,#25422,
#25423,#25424,#25425,#25426,#25427,#25428,#25429));
#25689=CLOSED_SHELL('',(#25430,#25431,#25432,#25433,#25434,#25435,#25436,
#25437,#25438,#25439,#25440,#25441,#25442,#25443));
#25690=CLOSED_SHELL('',(#25444,#25445,#25446,#25447,#25448,#25449,#25450,
#25451,#25452,#25453,#25454,#25455,#25456,#25457,#25458,#25459,#25460,#25461,
#25462,#25463,#25464));
#25691=CLOSED_SHELL('',(#25465,#25466,#25467,#25468,#25469,#25470,#25471,
#25472,#25473,#25474,#25475,#25476,#25477,#25478,#25479,#25480,#25481,#25482,
#25483,#25484,#25485,#25486,#25487,#25488,#25489,#25490,#25491,#25492,#25493,
#25494,#25495,#25496,#25497,#25498,#25499,#25500,#25501,#25502,#25503,#25504,
#25505,#25506,#25507,#25508,#25509,#25510,#25511,#25512,#25513,#25514,#25515,
#25516,#25517,#25518,#25519,#25520,#25521,#25522,#25523,#25524,#25525,#25526,
#25527,#25528,#25529,#25530,#25531,#25532,#25533,#25534,#25535,#25536,#25537,
#25538,#25539,#25540));
#25692=CLOSED_SHELL('',(#25541,#25542,#25543,#25544,#25545,#25546,#25547,
#25548,#25549,#25550,#25551,#25552,#25553,#25554,#25555,#25556,#25557,#25558,
#25559,#25560,#25561,#25562,#25563,#25564,#25565,#25566,#25567,#25568,#25569,
#25570,#25571,#25572,#25573,#25574,#25575,#25576,#25577,#25578,#25579,#25580,
#25581,#25582,#25583,#25584,#25585,#25586));
#25693=CLOSED_SHELL('',(#25587,#25588,#25589,#25590,#25591,#25592,#25593,
#25594,#25595,#25596,#25597,#25598,#25599,#25600));
#25694=CLOSED_SHELL('',(#25601,#25602,#25603,#25604,#25605,#25606,#25607,
#25608,#25609,#25610,#25611,#25612,#25613,#25614,#25615,#25616,#25617,#25618,
#25619,#25620,#25621));
#25695=CLOSED_SHELL('',(#25622,#25623,#25624,#25625));
#25696=CLOSED_SHELL('',(#25626,#25627,#25628,#25629,#25630,#25631));
#25697=CLOSED_SHELL('',(#25632,#25633,#25634,#25635,#25636,#25637,#25638,
#25639,#25640,#25641,#25642,#25643,#25644,#25645,#25646,#25647,#25648,#25649));
#25698=CLOSED_SHELL('',(#25650,#25651,#25652,#25653,#25654,#25655,#25656,
#25657,#25658,#25659,#25660,#25661,#25662,#25663));
#25699=DERIVED_UNIT_ELEMENT(#25761,1.);
#25700=DERIVED_UNIT_ELEMENT(#66723,-3.);
#25701=DERIVED_UNIT_ELEMENT(#25761,1.);
#25702=DERIVED_UNIT_ELEMENT(#66723,-3.);
#25703=DERIVED_UNIT_ELEMENT(#25761,1.);
#25704=DERIVED_UNIT_ELEMENT(#66723,-3.);
#25705=DERIVED_UNIT_ELEMENT(#25761,1.);
#25706=DERIVED_UNIT_ELEMENT(#66723,-3.);
#25707=DERIVED_UNIT_ELEMENT(#25761,1.);
#25708=DERIVED_UNIT_ELEMENT(#66723,-3.);
#25709=DERIVED_UNIT_ELEMENT(#25761,1.);
#25710=DERIVED_UNIT_ELEMENT(#66723,-3.);
#25711=DERIVED_UNIT_ELEMENT(#25761,1.);
#25712=DERIVED_UNIT_ELEMENT(#66723,-3.);
#25713=DERIVED_UNIT_ELEMENT(#25761,1.);
#25714=DERIVED_UNIT_ELEMENT(#66723,-3.);
#25715=DERIVED_UNIT_ELEMENT(#25761,1.);
#25716=DERIVED_UNIT_ELEMENT(#66723,-3.);
#25717=DERIVED_UNIT_ELEMENT(#25761,1.);
#25718=DERIVED_UNIT_ELEMENT(#66723,-3.);
#25719=DERIVED_UNIT_ELEMENT(#25761,1.);
#25720=DERIVED_UNIT_ELEMENT(#66723,-3.);
#25721=DERIVED_UNIT_ELEMENT(#25761,1.);
#25722=DERIVED_UNIT_ELEMENT(#66723,-3.);
#25723=DERIVED_UNIT_ELEMENT(#25761,1.);
#25724=DERIVED_UNIT_ELEMENT(#66723,-3.);
#25725=DERIVED_UNIT_ELEMENT(#25761,1.);
#25726=DERIVED_UNIT_ELEMENT(#66723,-3.);
#25727=DERIVED_UNIT_ELEMENT(#25761,1.);
#25728=DERIVED_UNIT_ELEMENT(#66723,-3.);
#25729=DERIVED_UNIT_ELEMENT(#25761,1.);
#25730=DERIVED_UNIT_ELEMENT(#66723,-3.);
#25731=DERIVED_UNIT_ELEMENT(#25761,1.);
#25732=DERIVED_UNIT_ELEMENT(#66723,-3.);
#25733=DERIVED_UNIT_ELEMENT(#25761,1.);
#25734=DERIVED_UNIT_ELEMENT(#66723,-3.);
#25735=DERIVED_UNIT_ELEMENT(#25761,1.);
#25736=DERIVED_UNIT_ELEMENT(#66723,-3.);
#25737=DERIVED_UNIT_ELEMENT(#25761,1.);
#25738=DERIVED_UNIT_ELEMENT(#66723,-3.);
#25739=DERIVED_UNIT_ELEMENT(#25761,1.);
#25740=DERIVED_UNIT_ELEMENT(#66723,-3.);
#25741=DERIVED_UNIT_ELEMENT(#25761,1.);
#25742=DERIVED_UNIT_ELEMENT(#66723,-3.);
#25743=DERIVED_UNIT_ELEMENT(#25761,1.);
#25744=DERIVED_UNIT_ELEMENT(#66723,-3.);
#25745=DERIVED_UNIT_ELEMENT(#25761,1.);
#25746=DERIVED_UNIT_ELEMENT(#66723,-3.);
#25747=DERIVED_UNIT_ELEMENT(#25761,1.);
#25748=DERIVED_UNIT_ELEMENT(#66723,-3.);
#25749=DERIVED_UNIT_ELEMENT(#25761,1.);
#25750=DERIVED_UNIT_ELEMENT(#66723,-3.);
#25751=DERIVED_UNIT_ELEMENT(#25761,1.);
#25752=DERIVED_UNIT_ELEMENT(#66723,-3.);
#25753=DERIVED_UNIT_ELEMENT(#25761,1.);
#25754=DERIVED_UNIT_ELEMENT(#66723,-3.);
#25755=DERIVED_UNIT_ELEMENT(#25761,1.);
#25756=DERIVED_UNIT_ELEMENT(#66723,-3.);
#25757=DERIVED_UNIT_ELEMENT(#25761,1.);
#25758=DERIVED_UNIT_ELEMENT(#66723,-3.);
#25759=DERIVED_UNIT_ELEMENT(#25761,1.);
#25760=DERIVED_UNIT_ELEMENT(#66723,-3.);
#25761=(
MASS_UNIT()
NAMED_UNIT(*)
SI_UNIT(.KILO.,.GRAM.)
);
#25762=DERIVED_UNIT((#25699,#25700));
#25763=DERIVED_UNIT((#25701,#25702));
#25764=DERIVED_UNIT((#25703,#25704));
#25765=DERIVED_UNIT((#25705,#25706));
#25766=DERIVED_UNIT((#25707,#25708));
#25767=DERIVED_UNIT((#25709,#25710));
#25768=DERIVED_UNIT((#25711,#25712));
#25769=DERIVED_UNIT((#25713,#25714));
#25770=DERIVED_UNIT((#25715,#25716));
#25771=DERIVED_UNIT((#25717,#25718));
#25772=DERIVED_UNIT((#25719,#25720));
#25773=DERIVED_UNIT((#25721,#25722));
#25774=DERIVED_UNIT((#25723,#25724));
#25775=DERIVED_UNIT((#25725,#25726));
#25776=DERIVED_UNIT((#25727,#25728));
#25777=DERIVED_UNIT((#25729,#25730));
#25778=DERIVED_UNIT((#25731,#25732));
#25779=DERIVED_UNIT((#25733,#25734));
#25780=DERIVED_UNIT((#25735,#25736));
#25781=DERIVED_UNIT((#25737,#25738));
#25782=DERIVED_UNIT((#25739,#25740));
#25783=DERIVED_UNIT((#25741,#25742));
#25784=DERIVED_UNIT((#25743,#25744));
#25785=DERIVED_UNIT((#25745,#25746));
#25786=DERIVED_UNIT((#25747,#25748));
#25787=DERIVED_UNIT((#25749,#25750));
#25788=DERIVED_UNIT((#25751,#25752));
#25789=DERIVED_UNIT((#25753,#25754));
#25790=DERIVED_UNIT((#25755,#25756));
#25791=DERIVED_UNIT((#25757,#25758));
#25792=DERIVED_UNIT((#25759,#25760));
#25793=MEASURE_REPRESENTATION_ITEM('density measure',
POSITIVE_RATIO_MEASURE(7850.),#25762);
#25794=MEASURE_REPRESENTATION_ITEM('density measure',
POSITIVE_RATIO_MEASURE(7850.),#25763);
#25795=MEASURE_REPRESENTATION_ITEM('density measure',
POSITIVE_RATIO_MEASURE(7850.),#25764);
#25796=MEASURE_REPRESENTATION_ITEM('density measure',
POSITIVE_RATIO_MEASURE(7850.),#25765);
#25797=MEASURE_REPRESENTATION_ITEM('density measure',
POSITIVE_RATIO_MEASURE(7850.),#25766);
#25798=MEASURE_REPRESENTATION_ITEM('density measure',
POSITIVE_RATIO_MEASURE(7850.),#25767);
#25799=MEASURE_REPRESENTATION_ITEM('density measure',
POSITIVE_RATIO_MEASURE(7850.),#25768);
#25800=MEASURE_REPRESENTATION_ITEM('density measure',
POSITIVE_RATIO_MEASURE(7850.),#25769);
#25801=MEASURE_REPRESENTATION_ITEM('density measure',
POSITIVE_RATIO_MEASURE(7850.),#25770);
#25802=MEASURE_REPRESENTATION_ITEM('density measure',
POSITIVE_RATIO_MEASURE(7850.),#25771);
#25803=MEASURE_REPRESENTATION_ITEM('density measure',
POSITIVE_RATIO_MEASURE(7850.),#25772);
#25804=MEASURE_REPRESENTATION_ITEM('density measure',
POSITIVE_RATIO_MEASURE(7850.),#25773);
#25805=MEASURE_REPRESENTATION_ITEM('density measure',
POSITIVE_RATIO_MEASURE(7850.),#25774);
#25806=MEASURE_REPRESENTATION_ITEM('density measure',
POSITIVE_RATIO_MEASURE(7850.),#25775);
#25807=MEASURE_REPRESENTATION_ITEM('density measure',
POSITIVE_RATIO_MEASURE(7850.),#25776);
#25808=MEASURE_REPRESENTATION_ITEM('density measure',
POSITIVE_RATIO_MEASURE(7850.),#25777);
#25809=MEASURE_REPRESENTATION_ITEM('density measure',
POSITIVE_RATIO_MEASURE(7850.),#25778);
#25810=MEASURE_REPRESENTATION_ITEM('density measure',
POSITIVE_RATIO_MEASURE(7850.),#25779);
#25811=MEASURE_REPRESENTATION_ITEM('density measure',
POSITIVE_RATIO_MEASURE(7850.),#25780);
#25812=MEASURE_REPRESENTATION_ITEM('density measure',
POSITIVE_RATIO_MEASURE(7850.),#25781);
#25813=MEASURE_REPRESENTATION_ITEM('density measure',
POSITIVE_RATIO_MEASURE(7850.),#25782);
#25814=MEASURE_REPRESENTATION_ITEM('density measure',
POSITIVE_RATIO_MEASURE(7850.),#25783);
#25815=MEASURE_REPRESENTATION_ITEM('density measure',
POSITIVE_RATIO_MEASURE(7850.),#25784);
#25816=MEASURE_REPRESENTATION_ITEM('density measure',
POSITIVE_RATIO_MEASURE(7850.),#25785);
#25817=MEASURE_REPRESENTATION_ITEM('density measure',
POSITIVE_RATIO_MEASURE(7850.),#25786);
#25818=MEASURE_REPRESENTATION_ITEM('density measure',
POSITIVE_RATIO_MEASURE(7850.),#25787);
#25819=MEASURE_REPRESENTATION_ITEM('density measure',
POSITIVE_RATIO_MEASURE(7850.),#25788);
#25820=MEASURE_REPRESENTATION_ITEM('density measure',
POSITIVE_RATIO_MEASURE(7850.),#25789);
#25821=MEASURE_REPRESENTATION_ITEM('density measure',
POSITIVE_RATIO_MEASURE(7850.),#25790);
#25822=MEASURE_REPRESENTATION_ITEM('density measure',
POSITIVE_RATIO_MEASURE(7850.),#25791);
#25823=MEASURE_REPRESENTATION_ITEM('density measure',
POSITIVE_RATIO_MEASURE(7850.),#25792);
#25824=PROPERTY_DEFINITION_REPRESENTATION(#25979,#25886);
#25825=PROPERTY_DEFINITION_REPRESENTATION(#25980,#25887);
#25826=PROPERTY_DEFINITION_REPRESENTATION(#25981,#25888);
#25827=PROPERTY_DEFINITION_REPRESENTATION(#25982,#25889);
#25828=PROPERTY_DEFINITION_REPRESENTATION(#25983,#25890);
#25829=PROPERTY_DEFINITION_REPRESENTATION(#25984,#25891);
#25830=PROPERTY_DEFINITION_REPRESENTATION(#25985,#25892);
#25831=PROPERTY_DEFINITION_REPRESENTATION(#25986,#25893);
#25832=PROPERTY_DEFINITION_REPRESENTATION(#25987,#25894);
#25833=PROPERTY_DEFINITION_REPRESENTATION(#25988,#25895);
#25834=PROPERTY_DEFINITION_REPRESENTATION(#25989,#25896);
#25835=PROPERTY_DEFINITION_REPRESENTATION(#25990,#25897);
#25836=PROPERTY_DEFINITION_REPRESENTATION(#25991,#25898);
#25837=PROPERTY_DEFINITION_REPRESENTATION(#25992,#25899);
#25838=PROPERTY_DEFINITION_REPRESENTATION(#25993,#25900);
#25839=PROPERTY_DEFINITION_REPRESENTATION(#25994,#25901);
#25840=PROPERTY_DEFINITION_REPRESENTATION(#25995,#25902);
#25841=PROPERTY_DEFINITION_REPRESENTATION(#25996,#25903);
#25842=PROPERTY_DEFINITION_REPRESENTATION(#25997,#25904);
#25843=PROPERTY_DEFINITION_REPRESENTATION(#25998,#25905);
#25844=PROPERTY_DEFINITION_REPRESENTATION(#25999,#25906);
#25845=PROPERTY_DEFINITION_REPRESENTATION(#26000,#25907);
#25846=PROPERTY_DEFINITION_REPRESENTATION(#26001,#25908);
#25847=PROPERTY_DEFINITION_REPRESENTATION(#26002,#25909);
#25848=PROPERTY_DEFINITION_REPRESENTATION(#26003,#25910);
#25849=PROPERTY_DEFINITION_REPRESENTATION(#26004,#25911);
#25850=PROPERTY_DEFINITION_REPRESENTATION(#26005,#25912);
#25851=PROPERTY_DEFINITION_REPRESENTATION(#26006,#25913);
#25852=PROPERTY_DEFINITION_REPRESENTATION(#26007,#25914);
#25853=PROPERTY_DEFINITION_REPRESENTATION(#26008,#25915);
#25854=PROPERTY_DEFINITION_REPRESENTATION(#26009,#25916);
#25855=PROPERTY_DEFINITION_REPRESENTATION(#26010,#25917);
#25856=PROPERTY_DEFINITION_REPRESENTATION(#26011,#25918);
#25857=PROPERTY_DEFINITION_REPRESENTATION(#26012,#25919);
#25858=PROPERTY_DEFINITION_REPRESENTATION(#26013,#25920);
#25859=PROPERTY_DEFINITION_REPRESENTATION(#26014,#25921);
#25860=PROPERTY_DEFINITION_REPRESENTATION(#26015,#25922);
#25861=PROPERTY_DEFINITION_REPRESENTATION(#26016,#25923);
#25862=PROPERTY_DEFINITION_REPRESENTATION(#26017,#25924);
#25863=PROPERTY_DEFINITION_REPRESENTATION(#26018,#25925);
#25864=PROPERTY_DEFINITION_REPRESENTATION(#26019,#25926);
#25865=PROPERTY_DEFINITION_REPRESENTATION(#26020,#25927);
#25866=PROPERTY_DEFINITION_REPRESENTATION(#26021,#25928);
#25867=PROPERTY_DEFINITION_REPRESENTATION(#26022,#25929);
#25868=PROPERTY_DEFINITION_REPRESENTATION(#26023,#25930);
#25869=PROPERTY_DEFINITION_REPRESENTATION(#26024,#25931);
#25870=PROPERTY_DEFINITION_REPRESENTATION(#26025,#25932);
#25871=PROPERTY_DEFINITION_REPRESENTATION(#26026,#25933);
#25872=PROPERTY_DEFINITION_REPRESENTATION(#26027,#25934);
#25873=PROPERTY_DEFINITION_REPRESENTATION(#26028,#25935);
#25874=PROPERTY_DEFINITION_REPRESENTATION(#26029,#25936);
#25875=PROPERTY_DEFINITION_REPRESENTATION(#26030,#25937);
#25876=PROPERTY_DEFINITION_REPRESENTATION(#26031,#25938);
#25877=PROPERTY_DEFINITION_REPRESENTATION(#26032,#25939);
#25878=PROPERTY_DEFINITION_REPRESENTATION(#26033,#25940);
#25879=PROPERTY_DEFINITION_REPRESENTATION(#26034,#25941);
#25880=PROPERTY_DEFINITION_REPRESENTATION(#26035,#25942);
#25881=PROPERTY_DEFINITION_REPRESENTATION(#26036,#25943);
#25882=PROPERTY_DEFINITION_REPRESENTATION(#26037,#25944);
#25883=PROPERTY_DEFINITION_REPRESENTATION(#26038,#25945);
#25884=PROPERTY_DEFINITION_REPRESENTATION(#26039,#25946);
#25885=PROPERTY_DEFINITION_REPRESENTATION(#26040,#25947);
#25886=REPRESENTATION('material name',(#25948),#66682);
#25887=REPRESENTATION('density',(#25793),#66682);
#25888=REPRESENTATION('material name',(#25949),#66684);
#25889=REPRESENTATION('density',(#25794),#66684);
#25890=REPRESENTATION('material name',(#25950),#66685);
#25891=REPRESENTATION('density',(#25795),#66685);
#25892=REPRESENTATION('material name',(#25951),#66687);
#25893=REPRESENTATION('density',(#25796),#66687);
#25894=REPRESENTATION('material name',(#25952),#66688);
#25895=REPRESENTATION('density',(#25797),#66688);
#25896=REPRESENTATION('material name',(#25953),#66689);
#25897=REPRESENTATION('density',(#25798),#66689);
#25898=REPRESENTATION('material name',(#25954),#66691);
#25899=REPRESENTATION('density',(#25799),#66691);
#25900=REPRESENTATION('material name',(#25955),#66692);
#25901=REPRESENTATION('density',(#25800),#66692);
#25902=REPRESENTATION('material name',(#25956),#66693);
#25903=REPRESENTATION('density',(#25801),#66693);
#25904=REPRESENTATION('material name',(#25957),#66695);
#25905=REPRESENTATION('density',(#25802),#66695);
#25906=REPRESENTATION('material name',(#25958),#66696);
#25907=REPRESENTATION('density',(#25803),#66696);
#25908=REPRESENTATION('material name',(#25959),#66698);
#25909=REPRESENTATION('density',(#25804),#66698);
#25910=REPRESENTATION('material name',(#25960),#66699);
#25911=REPRESENTATION('density',(#25805),#66699);
#25912=REPRESENTATION('material name',(#25961),#66701);
#25913=REPRESENTATION('density',(#25806),#66701);
#25914=REPRESENTATION('material name',(#25962),#66702);
#25915=REPRESENTATION('density',(#25807),#66702);
#25916=REPRESENTATION('material name',(#25963),#66703);
#25917=REPRESENTATION('density',(#25808),#66703);
#25918=REPRESENTATION('material name',(#25964),#66704);
#25919=REPRESENTATION('density',(#25809),#66704);
#25920=REPRESENTATION('material name',(#25965),#66707);
#25921=REPRESENTATION('density',(#25810),#66707);
#25922=REPRESENTATION('material name',(#25966),#66708);
#25923=REPRESENTATION('density',(#25811),#66708);
#25924=REPRESENTATION('material name',(#25967),#66709);
#25925=REPRESENTATION('density',(#25812),#66709);
#25926=REPRESENTATION('material name',(#25968),#66710);
#25927=REPRESENTATION('density',(#25813),#66710);
#25928=REPRESENTATION('material name',(#25969),#66711);
#25929=REPRESENTATION('density',(#25814),#66711);
#25930=REPRESENTATION('material name',(#25970),#66712);
#25931=REPRESENTATION('density',(#25815),#66712);
#25932=REPRESENTATION('material name',(#25971),#66713);
#25933=REPRESENTATION('density',(#25816),#66713);
#25934=REPRESENTATION('material name',(#25972),#66714);
#25935=REPRESENTATION('density',(#25817),#66714);
#25936=REPRESENTATION('material name',(#25973),#66715);
#25937=REPRESENTATION('density',(#25818),#66715);
#25938=REPRESENTATION('material name',(#25974),#66716);
#25939=REPRESENTATION('density',(#25819),#66716);
#25940=REPRESENTATION('material name',(#25975),#66717);
#25941=REPRESENTATION('density',(#25820),#66717);
#25942=REPRESENTATION('material name',(#25976),#66718);
#25943=REPRESENTATION('density',(#25821),#66718);
#25944=REPRESENTATION('material name',(#25977),#66719);
#25945=REPRESENTATION('density',(#25822),#66719);
#25946=REPRESENTATION('material name',(#25978),#66720);
#25947=REPRESENTATION('density',(#25823),#66720);
#25948=DESCRIPTIVE_REPRESENTATION_ITEM('Steel','Steel');
#25949=DESCRIPTIVE_REPRESENTATION_ITEM('Steel','Steel');
#25950=DESCRIPTIVE_REPRESENTATION_ITEM('Steel','Steel');
#25951=DESCRIPTIVE_REPRESENTATION_ITEM('Steel','Steel');
#25952=DESCRIPTIVE_REPRESENTATION_ITEM('Steel','Steel');
#25953=DESCRIPTIVE_REPRESENTATION_ITEM('Steel','Steel');
#25954=DESCRIPTIVE_REPRESENTATION_ITEM('Steel','Steel');
#25955=DESCRIPTIVE_REPRESENTATION_ITEM('Steel','Steel');
#25956=DESCRIPTIVE_REPRESENTATION_ITEM('Steel','Steel');
#25957=DESCRIPTIVE_REPRESENTATION_ITEM('Steel','Steel');
#25958=DESCRIPTIVE_REPRESENTATION_ITEM('Steel','Steel');
#25959=DESCRIPTIVE_REPRESENTATION_ITEM('Steel','Steel');
#25960=DESCRIPTIVE_REPRESENTATION_ITEM('Steel','Steel');
#25961=DESCRIPTIVE_REPRESENTATION_ITEM('Steel','Steel');
#25962=DESCRIPTIVE_REPRESENTATION_ITEM('Steel','Steel');
#25963=DESCRIPTIVE_REPRESENTATION_ITEM('Steel','Steel');
#25964=DESCRIPTIVE_REPRESENTATION_ITEM('Steel','Steel');
#25965=DESCRIPTIVE_REPRESENTATION_ITEM('Steel','Steel');
#25966=DESCRIPTIVE_REPRESENTATION_ITEM('Steel','Steel');
#25967=DESCRIPTIVE_REPRESENTATION_ITEM('Steel','Steel');
#25968=DESCRIPTIVE_REPRESENTATION_ITEM('Steel','Steel');
#25969=DESCRIPTIVE_REPRESENTATION_ITEM('Steel','Steel');
#25970=DESCRIPTIVE_REPRESENTATION_ITEM('Steel','Steel');
#25971=DESCRIPTIVE_REPRESENTATION_ITEM('Steel','Steel');
#25972=DESCRIPTIVE_REPRESENTATION_ITEM('Steel','Steel');
#25973=DESCRIPTIVE_REPRESENTATION_ITEM('Steel','Steel');
#25974=DESCRIPTIVE_REPRESENTATION_ITEM('Steel','Steel');
#25975=DESCRIPTIVE_REPRESENTATION_ITEM('Steel','Steel');
#25976=DESCRIPTIVE_REPRESENTATION_ITEM('Steel','Steel');
#25977=DESCRIPTIVE_REPRESENTATION_ITEM('Steel','Steel');
#25978=DESCRIPTIVE_REPRESENTATION_ITEM('Steel','Steel');
#25979=PROPERTY_DEFINITION('material property','material name',#66932);
#25980=PROPERTY_DEFINITION('material property','density of part',#66932);
#25981=PROPERTY_DEFINITION('material property','material name',#66934);
#25982=PROPERTY_DEFINITION('material property','density of part',#66934);
#25983=PROPERTY_DEFINITION('material property','material name',#66935);
#25984=PROPERTY_DEFINITION('material property','density of part',#66935);
#25985=PROPERTY_DEFINITION('material property','material name',#66937);
#25986=PROPERTY_DEFINITION('material property','density of part',#66937);
#25987=PROPERTY_DEFINITION('material property','material name',#66938);
#25988=PROPERTY_DEFINITION('material property','density of part',#66938);
#25989=PROPERTY_DEFINITION('material property','material name',#66939);
#25990=PROPERTY_DEFINITION('material property','density of part',#66939);
#25991=PROPERTY_DEFINITION('material property','material name',#66941);
#25992=PROPERTY_DEFINITION('material property','density of part',#66941);
#25993=PROPERTY_DEFINITION('material property','material name',#66942);
#25994=PROPERTY_DEFINITION('material property','density of part',#66942);
#25995=PROPERTY_DEFINITION('material property','material name',#66943);
#25996=PROPERTY_DEFINITION('material property','density of part',#66943);
#25997=PROPERTY_DEFINITION('material property','material name',#66945);
#25998=PROPERTY_DEFINITION('material property','density of part',#66945);
#25999=PROPERTY_DEFINITION('material property','material name',#66946);
#26000=PROPERTY_DEFINITION('material property','density of part',#66946);
#26001=PROPERTY_DEFINITION('material property','material name',#66948);
#26002=PROPERTY_DEFINITION('material property','density of part',#66948);
#26003=PROPERTY_DEFINITION('material property','material name',#66949);
#26004=PROPERTY_DEFINITION('material property','density of part',#66949);
#26005=PROPERTY_DEFINITION('material property','material name',#66951);
#26006=PROPERTY_DEFINITION('material property','density of part',#66951);
#26007=PROPERTY_DEFINITION('material property','material name',#66952);
#26008=PROPERTY_DEFINITION('material property','density of part',#66952);
#26009=PROPERTY_DEFINITION('material property','material name',#66953);
#26010=PROPERTY_DEFINITION('material property','density of part',#66953);
#26011=PROPERTY_DEFINITION('material property','material name',#66954);
#26012=PROPERTY_DEFINITION('material property','density of part',#66954);
#26013=PROPERTY_DEFINITION('material property','material name',#66957);
#26014=PROPERTY_DEFINITION('material property','density of part',#66957);
#26015=PROPERTY_DEFINITION('material property','material name',#66958);
#26016=PROPERTY_DEFINITION('material property','density of part',#66958);
#26017=PROPERTY_DEFINITION('material property','material name',#66959);
#26018=PROPERTY_DEFINITION('material property','density of part',#66959);
#26019=PROPERTY_DEFINITION('material property','material name',#66960);
#26020=PROPERTY_DEFINITION('material property','density of part',#66960);
#26021=PROPERTY_DEFINITION('material property','material name',#66961);
#26022=PROPERTY_DEFINITION('material property','density of part',#66961);
#26023=PROPERTY_DEFINITION('material property','material name',#66962);
#26024=PROPERTY_DEFINITION('material property','density of part',#66962);
#26025=PROPERTY_DEFINITION('material property','material name',#66963);
#26026=PROPERTY_DEFINITION('material property','density of part',#66963);
#26027=PROPERTY_DEFINITION('material property','material name',#66964);
#26028=PROPERTY_DEFINITION('material property','density of part',#66964);
#26029=PROPERTY_DEFINITION('material property','material name',#66965);
#26030=PROPERTY_DEFINITION('material property','density of part',#66965);
#26031=PROPERTY_DEFINITION('material property','material name',#66966);
#26032=PROPERTY_DEFINITION('material property','density of part',#66966);
#26033=PROPERTY_DEFINITION('material property','material name',#66967);
#26034=PROPERTY_DEFINITION('material property','density of part',#66967);
#26035=PROPERTY_DEFINITION('material property','material name',#66968);
#26036=PROPERTY_DEFINITION('material property','density of part',#66968);
#26037=PROPERTY_DEFINITION('material property','material name',#66969);
#26038=PROPERTY_DEFINITION('material property','density of part',#66969);
#26039=PROPERTY_DEFINITION('material property','material name',#66970);
#26040=PROPERTY_DEFINITION('material property','density of part',#66970);
#26041=AXIS2_PLACEMENT_3D('',#36175,#28756,#28757);
#26042=AXIS2_PLACEMENT_3D('',#36176,#28758,#28759);
#26043=AXIS2_PLACEMENT_3D('',#36177,#28760,#28761);
#26044=AXIS2_PLACEMENT_3D('',#36179,#28762,#28763);
#26045=AXIS2_PLACEMENT_3D('',#36182,#28765,#28766);
#26046=AXIS2_PLACEMENT_3D('',#36183,#28767,#28768);
#26047=AXIS2_PLACEMENT_3D('',#36185,#28769,#28770);
#26048=AXIS2_PLACEMENT_3D('',#36188,#28772,#28773);
#26049=AXIS2_PLACEMENT_3D('',#36189,#28774,#28775);
#26050=AXIS2_PLACEMENT_3D('',#36191,#28776,#28777);
#26051=AXIS2_PLACEMENT_3D('',#36194,#28779,#28780);
#26052=AXIS2_PLACEMENT_3D('',#36195,#28781,#28782);
#26053=AXIS2_PLACEMENT_3D('',#36197,#28783,#28784);
#26054=AXIS2_PLACEMENT_3D('',#36200,#28786,#28787);
#26055=AXIS2_PLACEMENT_3D('',#36201,#28788,#28789);
#26056=AXIS2_PLACEMENT_3D('',#36210,#28794,#28795);
#26057=AXIS2_PLACEMENT_3D('',#36216,#28799,#28800);
#26058=AXIS2_PLACEMENT_3D('',#36222,#28804,#28805);
#26059=AXIS2_PLACEMENT_3D('',#36225,#28808,#28809);
#26060=AXIS2_PLACEMENT_3D('',#36242,#28818,#28819);
#26061=AXIS2_PLACEMENT_3D('',#36259,#28828,#28829);
#26062=AXIS2_PLACEMENT_3D('',#36262,#28832,#28833);
#26063=AXIS2_PLACEMENT_3D('',#36264,#28835,#28836);
#26064=AXIS2_PLACEMENT_3D('',#36266,#28838,#28839);
#26065=AXIS2_PLACEMENT_3D('',#36267,#28840,#28841);
#26066=AXIS2_PLACEMENT_3D('',#36270,#28844,#28845);
#26067=AXIS2_PLACEMENT_3D('',#36272,#28847,#28848);
#26068=AXIS2_PLACEMENT_3D('',#36274,#28850,#28851);
#26069=AXIS2_PLACEMENT_3D('',#36275,#28852,#28853);
#26070=AXIS2_PLACEMENT_3D('',#36276,#28854,#28855);
#26071=AXIS2_PLACEMENT_3D('',#36277,#28856,#28857);
#26072=AXIS2_PLACEMENT_3D('',#36279,#28858,#28859);
#26073=AXIS2_PLACEMENT_3D('',#36282,#28861,#28862);
#26074=AXIS2_PLACEMENT_3D('',#36283,#28863,#28864);
#26075=AXIS2_PLACEMENT_3D('',#36285,#28865,#28866);
#26076=AXIS2_PLACEMENT_3D('',#36288,#28868,#28869);
#26077=AXIS2_PLACEMENT_3D('',#36289,#28870,#28871);
#26078=AXIS2_PLACEMENT_3D('',#36291,#28872,#28873);
#26079=AXIS2_PLACEMENT_3D('',#36294,#28875,#28876);
#26080=AXIS2_PLACEMENT_3D('',#36295,#28877,#28878);
#26081=AXIS2_PLACEMENT_3D('',#36297,#28879,#28880);
#26082=AXIS2_PLACEMENT_3D('',#36300,#28882,#28883);
#26083=AXIS2_PLACEMENT_3D('',#36301,#28884,#28885);
#26084=AXIS2_PLACEMENT_3D('',#36310,#28890,#28891);
#26085=AXIS2_PLACEMENT_3D('',#36320,#28897,#28898);
#26086=AXIS2_PLACEMENT_3D('',#36328,#28903,#28904);
#26087=AXIS2_PLACEMENT_3D('',#36338,#28910,#28911);
#26088=AXIS2_PLACEMENT_3D('',#36345,#28916,#28917);
#26089=AXIS2_PLACEMENT_3D('',#36349,#28920,#28921);
#26090=AXIS2_PLACEMENT_3D('',#36350,#28922,#28923);
#26091=AXIS2_PLACEMENT_3D('',#36354,#28926,#28927);
#26092=AXIS2_PLACEMENT_3D('',#36356,#28929,#28930);
#26093=AXIS2_PLACEMENT_3D('',#36360,#28933,#28934);
#26094=AXIS2_PLACEMENT_3D('',#36362,#28936,#28937);
#26095=AXIS2_PLACEMENT_3D('',#36363,#28938,#28939);
#26096=AXIS2_PLACEMENT_3D('',#36364,#28940,#28941);
#26097=AXIS2_PLACEMENT_3D('',#36366,#28942,#28943);
#26098=AXIS2_PLACEMENT_3D('',#36369,#28945,#28946);
#26099=AXIS2_PLACEMENT_3D('',#36370,#28947,#28948);
#26100=AXIS2_PLACEMENT_3D('',#36372,#28949,#28950);
#26101=AXIS2_PLACEMENT_3D('',#36375,#28952,#28953);
#26102=AXIS2_PLACEMENT_3D('',#36376,#28954,#28955);
#26103=AXIS2_PLACEMENT_3D('',#36378,#28956,#28957);
#26104=AXIS2_PLACEMENT_3D('',#36381,#28959,#28960);
#26105=AXIS2_PLACEMENT_3D('',#36382,#28961,#28962);
#26106=AXIS2_PLACEMENT_3D('',#36384,#28963,#28964);
#26107=AXIS2_PLACEMENT_3D('',#36387,#28966,#28967);
#26108=AXIS2_PLACEMENT_3D('',#36388,#28968,#28969);
#26109=AXIS2_PLACEMENT_3D('',#36390,#28970,#28971);
#26110=AXIS2_PLACEMENT_3D('',#36393,#28973,#28974);
#26111=AXIS2_PLACEMENT_3D('',#36394,#28975,#28976);
#26112=AXIS2_PLACEMENT_3D('',#36396,#28977,#28978);
#26113=AXIS2_PLACEMENT_3D('',#36399,#28980,#28981);
#26114=AXIS2_PLACEMENT_3D('',#36400,#28982,#28983);
#26115=AXIS2_PLACEMENT_3D('',#36402,#28984,#28985);
#26116=AXIS2_PLACEMENT_3D('',#36405,#28987,#28988);
#26117=AXIS2_PLACEMENT_3D('',#36406,#28989,#28990);
#26118=AXIS2_PLACEMENT_3D('',#36408,#28991,#28992);
#26119=AXIS2_PLACEMENT_3D('',#36411,#28994,#28995);
#26120=AXIS2_PLACEMENT_3D('',#36412,#28996,#28997);
#26121=AXIS2_PLACEMENT_3D('',#36414,#28998,#28999);
#26122=AXIS2_PLACEMENT_3D('',#36417,#29001,#29002);
#26123=AXIS2_PLACEMENT_3D('',#36418,#29003,#29004);
#26124=AXIS2_PLACEMENT_3D('',#36420,#29005,#29006);
#26125=AXIS2_PLACEMENT_3D('',#36423,#29008,#29009);
#26126=AXIS2_PLACEMENT_3D('',#36424,#29010,#29011);
#26127=AXIS2_PLACEMENT_3D('',#36426,#29012,#29013);
#26128=AXIS2_PLACEMENT_3D('',#36429,#29015,#29016);
#26129=AXIS2_PLACEMENT_3D('',#36430,#29017,#29018);
#26130=AXIS2_PLACEMENT_3D('',#36432,#29019,#29020);
#26131=AXIS2_PLACEMENT_3D('',#36435,#29022,#29023);
#26132=AXIS2_PLACEMENT_3D('',#36436,#29024,#29025);
#26133=AXIS2_PLACEMENT_3D('',#36445,#29030,#29031);
#26134=AXIS2_PLACEMENT_3D('',#36451,#29035,#29036);
#26135=AXIS2_PLACEMENT_3D('',#36455,#29039,#29040);
#26136=AXIS2_PLACEMENT_3D('',#36459,#29043,#29044);
#26137=AXIS2_PLACEMENT_3D('',#36461,#29046,#29047);
#26138=AXIS2_PLACEMENT_3D('',#36462,#29048,#29049);
#26139=AXIS2_PLACEMENT_3D('',#36463,#29050,#29051);
#26140=AXIS2_PLACEMENT_3D('',#36464,#29052,#29053);
#26141=AXIS2_PLACEMENT_3D('',#36465,#29054,#29055);
#26142=AXIS2_PLACEMENT_3D('',#36466,#29056,#29057);
#26143=AXIS2_PLACEMENT_3D('',#36467,#29058,#29059);
#26144=AXIS2_PLACEMENT_3D('',#36469,#29060,#29061);
#26145=AXIS2_PLACEMENT_3D('',#36472,#29063,#29064);
#26146=AXIS2_PLACEMENT_3D('',#36473,#29065,#29066);
#26147=AXIS2_PLACEMENT_3D('',#36475,#29067,#29068);
#26148=AXIS2_PLACEMENT_3D('',#36478,#29070,#29071);
#26149=AXIS2_PLACEMENT_3D('',#36479,#29072,#29073);
#26150=AXIS2_PLACEMENT_3D('',#36481,#29074,#29075);
#26151=AXIS2_PLACEMENT_3D('',#36484,#29077,#29078);
#26152=AXIS2_PLACEMENT_3D('',#36485,#29079,#29080);
#26153=AXIS2_PLACEMENT_3D('',#36487,#29081,#29082);
#26154=AXIS2_PLACEMENT_3D('',#36490,#29084,#29085);
#26155=AXIS2_PLACEMENT_3D('',#36491,#29086,#29087);
#26156=AXIS2_PLACEMENT_3D('',#36493,#29088,#29089);
#26157=AXIS2_PLACEMENT_3D('',#36496,#29091,#29092);
#26158=AXIS2_PLACEMENT_3D('',#36497,#29093,#29094);
#26159=AXIS2_PLACEMENT_3D('',#36499,#29095,#29096);
#26160=AXIS2_PLACEMENT_3D('',#36502,#29098,#29099);
#26161=AXIS2_PLACEMENT_3D('',#36503,#29100,#29101);
#26162=AXIS2_PLACEMENT_3D('',#36505,#29102,#29103);
#26163=AXIS2_PLACEMENT_3D('',#36508,#29105,#29106);
#26164=AXIS2_PLACEMENT_3D('',#36509,#29107,#29108);
#26165=AXIS2_PLACEMENT_3D('',#36514,#29110,#29111);
#26166=AXIS2_PLACEMENT_3D('',#36521,#29115,#29116);
#26167=AXIS2_PLACEMENT_3D('',#36522,#29117,#29118);
#26168=AXIS2_PLACEMENT_3D('',#36528,#29122,#29123);
#26169=AXIS2_PLACEMENT_3D('',#36532,#29125,#29126);
#26170=AXIS2_PLACEMENT_3D('',#36534,#29127,#29128);
#26171=AXIS2_PLACEMENT_3D('',#36538,#29131,#29132);
#26172=AXIS2_PLACEMENT_3D('',#36541,#29135,#29136);
#26173=AXIS2_PLACEMENT_3D('',#36543,#29138,#29139);
#26174=AXIS2_PLACEMENT_3D('',#36545,#29141,#29142);
#26175=AXIS2_PLACEMENT_3D('',#36546,#29143,#29144);
#26176=AXIS2_PLACEMENT_3D('',#36547,#29145,#29146);
#26177=AXIS2_PLACEMENT_3D('',#36548,#29147,#29148);
#26178=AXIS2_PLACEMENT_3D('',#36550,#29149,#29150);
#26179=AXIS2_PLACEMENT_3D('',#36553,#29152,#29153);
#26180=AXIS2_PLACEMENT_3D('',#36554,#29154,#29155);
#26181=AXIS2_PLACEMENT_3D('',#36556,#29156,#29157);
#26182=AXIS2_PLACEMENT_3D('',#36559,#29159,#29160);
#26183=AXIS2_PLACEMENT_3D('',#36560,#29161,#29162);
#26184=AXIS2_PLACEMENT_3D('',#36562,#29163,#29164);
#26185=AXIS2_PLACEMENT_3D('',#36565,#29166,#29167);
#26186=AXIS2_PLACEMENT_3D('',#36566,#29168,#29169);
#26187=AXIS2_PLACEMENT_3D('',#36568,#29170,#29171);
#26188=AXIS2_PLACEMENT_3D('',#36571,#29173,#29174);
#26189=AXIS2_PLACEMENT_3D('',#36572,#29175,#29176);
#26190=AXIS2_PLACEMENT_3D('',#36574,#29177,#29178);
#26191=AXIS2_PLACEMENT_3D('',#36577,#29180,#29181);
#26192=AXIS2_PLACEMENT_3D('',#36578,#29182,#29183);
#26193=AXIS2_PLACEMENT_3D('',#36580,#29184,#29185);
#26194=AXIS2_PLACEMENT_3D('',#36583,#29187,#29188);
#26195=AXIS2_PLACEMENT_3D('',#36584,#29189,#29190);
#26196=AXIS2_PLACEMENT_3D('',#36593,#29195,#29196);
#26197=AXIS2_PLACEMENT_3D('',#36599,#29200,#29201);
#26198=AXIS2_PLACEMENT_3D('',#36605,#29205,#29206);
#26199=AXIS2_PLACEMENT_3D('',#36608,#29209,#29210);
#26200=AXIS2_PLACEMENT_3D('',#36609,#29211,#29212);
#26201=AXIS2_PLACEMENT_3D('',#36610,#29213,#29214);
#26202=AXIS2_PLACEMENT_3D('',#36611,#29215,#29216);
#26203=AXIS2_PLACEMENT_3D('',#36612,#29217,#29218);
#26204=AXIS2_PLACEMENT_3D('',#36613,#29219,#29220);
#26205=AXIS2_PLACEMENT_3D('',#36615,#29221,#29222);
#26206=AXIS2_PLACEMENT_3D('',#36618,#29224,#29225);
#26207=AXIS2_PLACEMENT_3D('',#36619,#29226,#29227);
#26208=AXIS2_PLACEMENT_3D('',#36621,#29228,#29229);
#26209=AXIS2_PLACEMENT_3D('',#36624,#29231,#29232);
#26210=AXIS2_PLACEMENT_3D('',#36625,#29233,#29234);
#26211=AXIS2_PLACEMENT_3D('',#36627,#29235,#29236);
#26212=AXIS2_PLACEMENT_3D('',#36630,#29238,#29239);
#26213=AXIS2_PLACEMENT_3D('',#36631,#29240,#29241);
#26214=AXIS2_PLACEMENT_3D('',#36633,#29242,#29243);
#26215=AXIS2_PLACEMENT_3D('',#36636,#29245,#29246);
#26216=AXIS2_PLACEMENT_3D('',#36637,#29247,#29248);
#26217=AXIS2_PLACEMENT_3D('',#36639,#29249,#29250);
#26218=AXIS2_PLACEMENT_3D('',#36642,#29252,#29253);
#26219=AXIS2_PLACEMENT_3D('',#36643,#29254,#29255);
#26220=AXIS2_PLACEMENT_3D('',#36645,#29256,#29257);
#26221=AXIS2_PLACEMENT_3D('',#36648,#29259,#29260);
#26222=AXIS2_PLACEMENT_3D('',#36649,#29261,#29262);
#26223=AXIS2_PLACEMENT_3D('',#36658,#29267,#29268);
#26224=AXIS2_PLACEMENT_3D('',#36664,#29272,#29273);
#26225=AXIS2_PLACEMENT_3D('',#36670,#29277,#29278);
#26226=AXIS2_PLACEMENT_3D('',#36673,#29281,#29282);
#26227=AXIS2_PLACEMENT_3D('',#36674,#29283,#29284);
#26228=AXIS2_PLACEMENT_3D('',#36675,#29285,#29286);
#26229=AXIS2_PLACEMENT_3D('',#36676,#29287,#29288);
#26230=AXIS2_PLACEMENT_3D('',#36677,#29289,#29290);
#26231=AXIS2_PLACEMENT_3D('',#36679,#29291,#29292);
#26232=AXIS2_PLACEMENT_3D('',#36682,#29294,#29295);
#26233=AXIS2_PLACEMENT_3D('',#36683,#29296,#29297);
#26234=AXIS2_PLACEMENT_3D('',#36686,#29298,#29299);
#26235=AXIS2_PLACEMENT_3D('',#36688,#29300,#29301);
#26236=AXIS2_PLACEMENT_3D('',#36690,#29302,#29303);
#26237=AXIS2_PLACEMENT_3D('',#36692,#29304,#29305);
#26238=AXIS2_PLACEMENT_3D('',#36694,#29306,#29307);
#26239=AXIS2_PLACEMENT_3D('',#36697,#29309,#29310);
#26240=AXIS2_PLACEMENT_3D('',#36699,#29311,#29312);
#26241=AXIS2_PLACEMENT_3D('',#36701,#29313,#29314);
#26242=AXIS2_PLACEMENT_3D('',#36703,#29315,#29316);
#26243=AXIS2_PLACEMENT_3D('',#36704,#29317,#29318);
#26244=AXIS2_PLACEMENT_3D('',#36705,#29319,#29320);
#26245=AXIS2_PLACEMENT_3D('',#36707,#29321,#29322);
#26246=AXIS2_PLACEMENT_3D('',#36710,#29324,#29325);
#26247=AXIS2_PLACEMENT_3D('',#36711,#29326,#29327);
#26248=AXIS2_PLACEMENT_3D('',#36714,#29328,#29329);
#26249=AXIS2_PLACEMENT_3D('',#36716,#29330,#29331);
#26250=AXIS2_PLACEMENT_3D('',#36718,#29332,#29333);
#26251=AXIS2_PLACEMENT_3D('',#36720,#29334,#29335);
#26252=AXIS2_PLACEMENT_3D('',#36722,#29336,#29337);
#26253=AXIS2_PLACEMENT_3D('',#36725,#29339,#29340);
#26254=AXIS2_PLACEMENT_3D('',#36727,#29341,#29342);
#26255=AXIS2_PLACEMENT_3D('',#36729,#29343,#29344);
#26256=AXIS2_PLACEMENT_3D('',#36731,#29345,#29346);
#26257=AXIS2_PLACEMENT_3D('',#36732,#29347,#29348);
#26258=AXIS2_PLACEMENT_3D('',#36733,#29349,#29350);
#26259=AXIS2_PLACEMENT_3D('',#36735,#29351,#29352);
#26260=AXIS2_PLACEMENT_3D('',#36738,#29354,#29355);
#26261=AXIS2_PLACEMENT_3D('',#36739,#29356,#29357);
#26262=AXIS2_PLACEMENT_3D('',#36742,#29358,#29359);
#26263=AXIS2_PLACEMENT_3D('',#36744,#29360,#29361);
#26264=AXIS2_PLACEMENT_3D('',#36746,#29362,#29363);
#26265=AXIS2_PLACEMENT_3D('',#36748,#29364,#29365);
#26266=AXIS2_PLACEMENT_3D('',#36750,#29366,#29367);
#26267=AXIS2_PLACEMENT_3D('',#36753,#29369,#29370);
#26268=AXIS2_PLACEMENT_3D('',#36755,#29371,#29372);
#26269=AXIS2_PLACEMENT_3D('',#36757,#29373,#29374);
#26270=AXIS2_PLACEMENT_3D('',#36759,#29375,#29376);
#26271=AXIS2_PLACEMENT_3D('',#36760,#29377,#29378);
#26272=AXIS2_PLACEMENT_3D('',#36761,#29379,#29380);
#26273=AXIS2_PLACEMENT_3D('',#36763,#29381,#29382);
#26274=AXIS2_PLACEMENT_3D('',#36766,#29384,#29385);
#26275=AXIS2_PLACEMENT_3D('',#36767,#29386,#29387);
#26276=AXIS2_PLACEMENT_3D('',#36770,#29388,#29389);
#26277=AXIS2_PLACEMENT_3D('',#36772,#29390,#29391);
#26278=AXIS2_PLACEMENT_3D('',#36774,#29392,#29393);
#26279=AXIS2_PLACEMENT_3D('',#36776,#29394,#29395);
#26280=AXIS2_PLACEMENT_3D('',#36778,#29396,#29397);
#26281=AXIS2_PLACEMENT_3D('',#36781,#29399,#29400);
#26282=AXIS2_PLACEMENT_3D('',#36783,#29401,#29402);
#26283=AXIS2_PLACEMENT_3D('',#36785,#29403,#29404);
#26284=AXIS2_PLACEMENT_3D('',#36787,#29405,#29406);
#26285=AXIS2_PLACEMENT_3D('',#36788,#29407,#29408);
#26286=AXIS2_PLACEMENT_3D('',#36789,#29409,#29410);
#26287=AXIS2_PLACEMENT_3D('',#36791,#29411,#29412);
#26288=AXIS2_PLACEMENT_3D('',#36794,#29414,#29415);
#26289=AXIS2_PLACEMENT_3D('',#36795,#29416,#29417);
#26290=AXIS2_PLACEMENT_3D('',#36798,#29418,#29419);
#26291=AXIS2_PLACEMENT_3D('',#36800,#29420,#29421);
#26292=AXIS2_PLACEMENT_3D('',#36802,#29422,#29423);
#26293=AXIS2_PLACEMENT_3D('',#36804,#29424,#29425);
#26294=AXIS2_PLACEMENT_3D('',#36806,#29426,#29427);
#26295=AXIS2_PLACEMENT_3D('',#36809,#29429,#29430);
#26296=AXIS2_PLACEMENT_3D('',#36811,#29431,#29432);
#26297=AXIS2_PLACEMENT_3D('',#36813,#29433,#29434);
#26298=AXIS2_PLACEMENT_3D('',#36815,#29435,#29436);
#26299=AXIS2_PLACEMENT_3D('',#36816,#29437,#29438);
#26300=AXIS2_PLACEMENT_3D('',#36817,#29439,#29440);
#26301=AXIS2_PLACEMENT_3D('',#36819,#29441,#29442);
#26302=AXIS2_PLACEMENT_3D('',#36822,#29444,#29445);
#26303=AXIS2_PLACEMENT_3D('',#36823,#29446,#29447);
#26304=AXIS2_PLACEMENT_3D('',#36826,#29448,#29449);
#26305=AXIS2_PLACEMENT_3D('',#36828,#29450,#29451);
#26306=AXIS2_PLACEMENT_3D('',#36830,#29452,#29453);
#26307=AXIS2_PLACEMENT_3D('',#36832,#29454,#29455);
#26308=AXIS2_PLACEMENT_3D('',#36834,#29456,#29457);
#26309=AXIS2_PLACEMENT_3D('',#36837,#29459,#29460);
#26310=AXIS2_PLACEMENT_3D('',#36839,#29461,#29462);
#26311=AXIS2_PLACEMENT_3D('',#36841,#29463,#29464);
#26312=AXIS2_PLACEMENT_3D('',#36843,#29465,#29466);
#26313=AXIS2_PLACEMENT_3D('',#36844,#29467,#29468);
#26314=AXIS2_PLACEMENT_3D('',#36845,#29469,#29470);
#26315=AXIS2_PLACEMENT_3D('',#36847,#29471,#29472);
#26316=AXIS2_PLACEMENT_3D('',#36850,#29474,#29475);
#26317=AXIS2_PLACEMENT_3D('',#36851,#29476,#29477);
#26318=AXIS2_PLACEMENT_3D('',#36854,#29478,#29479);
#26319=AXIS2_PLACEMENT_3D('',#36856,#29480,#29481);
#26320=AXIS2_PLACEMENT_3D('',#36858,#29482,#29483);
#26321=AXIS2_PLACEMENT_3D('',#36860,#29484,#29485);
#26322=AXIS2_PLACEMENT_3D('',#36862,#29486,#29487);
#26323=AXIS2_PLACEMENT_3D('',#36865,#29489,#29490);
#26324=AXIS2_PLACEMENT_3D('',#36867,#29491,#29492);
#26325=AXIS2_PLACEMENT_3D('',#36869,#29493,#29494);
#26326=AXIS2_PLACEMENT_3D('',#36871,#29495,#29496);
#26327=AXIS2_PLACEMENT_3D('',#36872,#29497,#29498);
#26328=AXIS2_PLACEMENT_3D('',#36873,#29499,#29500);
#26329=AXIS2_PLACEMENT_3D('',#36875,#29501,#29502);
#26330=AXIS2_PLACEMENT_3D('',#36878,#29504,#29505);
#26331=AXIS2_PLACEMENT_3D('',#36879,#29506,#29507);
#26332=AXIS2_PLACEMENT_3D('',#36882,#29508,#29509);
#26333=AXIS2_PLACEMENT_3D('',#36884,#29510,#29511);
#26334=AXIS2_PLACEMENT_3D('',#36886,#29512,#29513);
#26335=AXIS2_PLACEMENT_3D('',#36888,#29514,#29515);
#26336=AXIS2_PLACEMENT_3D('',#36890,#29516,#29517);
#26337=AXIS2_PLACEMENT_3D('',#36893,#29519,#29520);
#26338=AXIS2_PLACEMENT_3D('',#36895,#29521,#29522);
#26339=AXIS2_PLACEMENT_3D('',#36897,#29523,#29524);
#26340=AXIS2_PLACEMENT_3D('',#36899,#29525,#29526);
#26341=AXIS2_PLACEMENT_3D('',#36900,#29527,#29528);
#26342=AXIS2_PLACEMENT_3D('',#36901,#29529,#29530);
#26343=AXIS2_PLACEMENT_3D('',#36903,#29531,#29532);
#26344=AXIS2_PLACEMENT_3D('',#36906,#29534,#29535);
#26345=AXIS2_PLACEMENT_3D('',#36907,#29536,#29537);
#26346=AXIS2_PLACEMENT_3D('',#36910,#29538,#29539);
#26347=AXIS2_PLACEMENT_3D('',#36912,#29540,#29541);
#26348=AXIS2_PLACEMENT_3D('',#36914,#29542,#29543);
#26349=AXIS2_PLACEMENT_3D('',#36916,#29544,#29545);
#26350=AXIS2_PLACEMENT_3D('',#36918,#29546,#29547);
#26351=AXIS2_PLACEMENT_3D('',#36921,#29549,#29550);
#26352=AXIS2_PLACEMENT_3D('',#36923,#29551,#29552);
#26353=AXIS2_PLACEMENT_3D('',#36925,#29553,#29554);
#26354=AXIS2_PLACEMENT_3D('',#36927,#29555,#29556);
#26355=AXIS2_PLACEMENT_3D('',#36928,#29557,#29558);
#26356=AXIS2_PLACEMENT_3D('',#36929,#29559,#29560);
#26357=AXIS2_PLACEMENT_3D('',#36931,#29561,#29562);
#26358=AXIS2_PLACEMENT_3D('',#36934,#29564,#29565);
#26359=AXIS2_PLACEMENT_3D('',#36935,#29566,#29567);
#26360=AXIS2_PLACEMENT_3D('',#36938,#29568,#29569);
#26361=AXIS2_PLACEMENT_3D('',#36940,#29570,#29571);
#26362=AXIS2_PLACEMENT_3D('',#36942,#29572,#29573);
#26363=AXIS2_PLACEMENT_3D('',#36944,#29574,#29575);
#26364=AXIS2_PLACEMENT_3D('',#36946,#29576,#29577);
#26365=AXIS2_PLACEMENT_3D('',#36949,#29579,#29580);
#26366=AXIS2_PLACEMENT_3D('',#36951,#29581,#29582);
#26367=AXIS2_PLACEMENT_3D('',#36953,#29583,#29584);
#26368=AXIS2_PLACEMENT_3D('',#36955,#29585,#29586);
#26369=AXIS2_PLACEMENT_3D('',#36956,#29587,#29588);
#26370=AXIS2_PLACEMENT_3D('',#36957,#29589,#29590);
#26371=AXIS2_PLACEMENT_3D('',#36959,#29591,#29592);
#26372=AXIS2_PLACEMENT_3D('',#36962,#29594,#29595);
#26373=AXIS2_PLACEMENT_3D('',#36963,#29596,#29597);
#26374=AXIS2_PLACEMENT_3D('',#36966,#29598,#29599);
#26375=AXIS2_PLACEMENT_3D('',#36968,#29600,#29601);
#26376=AXIS2_PLACEMENT_3D('',#36970,#29602,#29603);
#26377=AXIS2_PLACEMENT_3D('',#36972,#29604,#29605);
#26378=AXIS2_PLACEMENT_3D('',#36974,#29606,#29607);
#26379=AXIS2_PLACEMENT_3D('',#36977,#29609,#29610);
#26380=AXIS2_PLACEMENT_3D('',#36979,#29611,#29612);
#26381=AXIS2_PLACEMENT_3D('',#36981,#29613,#29614);
#26382=AXIS2_PLACEMENT_3D('',#36983,#29615,#29616);
#26383=AXIS2_PLACEMENT_3D('',#36984,#29617,#29618);
#26384=AXIS2_PLACEMENT_3D('',#36985,#29619,#29620);
#26385=AXIS2_PLACEMENT_3D('',#36987,#29621,#29622);
#26386=AXIS2_PLACEMENT_3D('',#36990,#29624,#29625);
#26387=AXIS2_PLACEMENT_3D('',#36991,#29626,#29627);
#26388=AXIS2_PLACEMENT_3D('',#36994,#29628,#29629);
#26389=AXIS2_PLACEMENT_3D('',#36996,#29630,#29631);
#26390=AXIS2_PLACEMENT_3D('',#36998,#29632,#29633);
#26391=AXIS2_PLACEMENT_3D('',#37000,#29634,#29635);
#26392=AXIS2_PLACEMENT_3D('',#37002,#29636,#29637);
#26393=AXIS2_PLACEMENT_3D('',#37005,#29639,#29640);
#26394=AXIS2_PLACEMENT_3D('',#37007,#29641,#29642);
#26395=AXIS2_PLACEMENT_3D('',#37009,#29643,#29644);
#26396=AXIS2_PLACEMENT_3D('',#37011,#29645,#29646);
#26397=AXIS2_PLACEMENT_3D('',#37012,#29647,#29648);
#26398=AXIS2_PLACEMENT_3D('',#37013,#29649,#29650);
#26399=AXIS2_PLACEMENT_3D('',#37015,#29651,#29652);
#26400=AXIS2_PLACEMENT_3D('',#37018,#29654,#29655);
#26401=AXIS2_PLACEMENT_3D('',#37019,#29656,#29657);
#26402=AXIS2_PLACEMENT_3D('',#37022,#29658,#29659);
#26403=AXIS2_PLACEMENT_3D('',#37024,#29660,#29661);
#26404=AXIS2_PLACEMENT_3D('',#37026,#29662,#29663);
#26405=AXIS2_PLACEMENT_3D('',#37028,#29664,#29665);
#26406=AXIS2_PLACEMENT_3D('',#37030,#29666,#29667);
#26407=AXIS2_PLACEMENT_3D('',#37033,#29669,#29670);
#26408=AXIS2_PLACEMENT_3D('',#37035,#29671,#29672);
#26409=AXIS2_PLACEMENT_3D('',#37037,#29673,#29674);
#26410=AXIS2_PLACEMENT_3D('',#37039,#29675,#29676);
#26411=AXIS2_PLACEMENT_3D('',#37040,#29677,#29678);
#26412=AXIS2_PLACEMENT_3D('',#37041,#29679,#29680);
#26413=AXIS2_PLACEMENT_3D('',#37043,#29681,#29682);
#26414=AXIS2_PLACEMENT_3D('',#37046,#29684,#29685);
#26415=AXIS2_PLACEMENT_3D('',#37047,#29686,#29687);
#26416=AXIS2_PLACEMENT_3D('',#37050,#29688,#29689);
#26417=AXIS2_PLACEMENT_3D('',#37052,#29690,#29691);
#26418=AXIS2_PLACEMENT_3D('',#37054,#29692,#29693);
#26419=AXIS2_PLACEMENT_3D('',#37056,#29694,#29695);
#26420=AXIS2_PLACEMENT_3D('',#37058,#29696,#29697);
#26421=AXIS2_PLACEMENT_3D('',#37061,#29699,#29700);
#26422=AXIS2_PLACEMENT_3D('',#37063,#29701,#29702);
#26423=AXIS2_PLACEMENT_3D('',#37065,#29703,#29704);
#26424=AXIS2_PLACEMENT_3D('',#37067,#29705,#29706);
#26425=AXIS2_PLACEMENT_3D('',#37068,#29707,#29708);
#26426=AXIS2_PLACEMENT_3D('',#37069,#29709,#29710);
#26427=AXIS2_PLACEMENT_3D('',#37071,#29711,#29712);
#26428=AXIS2_PLACEMENT_3D('',#37074,#29714,#29715);
#26429=AXIS2_PLACEMENT_3D('',#37075,#29716,#29717);
#26430=AXIS2_PLACEMENT_3D('',#37078,#29718,#29719);
#26431=AXIS2_PLACEMENT_3D('',#37080,#29720,#29721);
#26432=AXIS2_PLACEMENT_3D('',#37082,#29722,#29723);
#26433=AXIS2_PLACEMENT_3D('',#37084,#29724,#29725);
#26434=AXIS2_PLACEMENT_3D('',#37086,#29726,#29727);
#26435=AXIS2_PLACEMENT_3D('',#37089,#29729,#29730);
#26436=AXIS2_PLACEMENT_3D('',#37091,#29731,#29732);
#26437=AXIS2_PLACEMENT_3D('',#37093,#29733,#29734);
#26438=AXIS2_PLACEMENT_3D('',#37095,#29735,#29736);
#26439=AXIS2_PLACEMENT_3D('',#37096,#29737,#29738);
#26440=AXIS2_PLACEMENT_3D('',#37097,#29739,#29740);
#26441=AXIS2_PLACEMENT_3D('',#37103,#29744,#29745);
#26442=AXIS2_PLACEMENT_3D('',#37106,#29748,#29749);
#26443=AXIS2_PLACEMENT_3D('',#37128,#29768,#29769);
#26444=AXIS2_PLACEMENT_3D('',#37130,#29771,#29772);
#26445=AXIS2_PLACEMENT_3D('',#37153,#29791,#29792);
#26446=AXIS2_PLACEMENT_3D('',#37154,#29793,#29794);
#26447=AXIS2_PLACEMENT_3D('',#37157,#29797,#29798);
#26448=AXIS2_PLACEMENT_3D('',#37158,#29799,#29800);
#26449=AXIS2_PLACEMENT_3D('',#37159,#29801,#29802);
#26450=AXIS2_PLACEMENT_3D('',#37162,#29805,#29806);
#26451=AXIS2_PLACEMENT_3D('',#37163,#29807,#29808);
#26452=AXIS2_PLACEMENT_3D('',#37164,#29809,#29810);
#26453=AXIS2_PLACEMENT_3D('',#37167,#29813,#29814);
#26454=AXIS2_PLACEMENT_3D('',#37168,#29815,#29816);
#26455=AXIS2_PLACEMENT_3D('',#37169,#29817,#29818);
#26456=AXIS2_PLACEMENT_3D('',#37172,#29821,#29822);
#26457=AXIS2_PLACEMENT_3D('',#37173,#29823,#29824);
#26458=AXIS2_PLACEMENT_3D('',#37174,#29825,#29826);
#26459=AXIS2_PLACEMENT_3D('',#37177,#29829,#29830);
#26460=AXIS2_PLACEMENT_3D('',#37178,#29831,#29832);
#26461=AXIS2_PLACEMENT_3D('',#37179,#29833,#29834);
#26462=AXIS2_PLACEMENT_3D('',#37182,#29837,#29838);
#26463=AXIS2_PLACEMENT_3D('',#37183,#29839,#29840);
#26464=AXIS2_PLACEMENT_3D('',#37184,#29841,#29842);
#26465=AXIS2_PLACEMENT_3D('',#37187,#29845,#29846);
#26466=AXIS2_PLACEMENT_3D('',#37188,#29847,#29848);
#26467=AXIS2_PLACEMENT_3D('',#37189,#29849,#29850);
#26468=AXIS2_PLACEMENT_3D('',#37192,#29853,#29854);
#26469=AXIS2_PLACEMENT_3D('',#37193,#29855,#29856);
#26470=AXIS2_PLACEMENT_3D('',#37194,#29857,#29858);
#26471=AXIS2_PLACEMENT_3D('',#37197,#29861,#29862);
#26472=AXIS2_PLACEMENT_3D('',#37198,#29863,#29864);
#26473=AXIS2_PLACEMENT_3D('',#37201,#29867,#29868);
#26474=AXIS2_PLACEMENT_3D('',#37202,#29869,#29870);
#26475=AXIS2_PLACEMENT_3D('',#37203,#29871,#29872);
#26476=AXIS2_PLACEMENT_3D('',#37204,#29873,#29874);
#26477=AXIS2_PLACEMENT_3D('',#37207,#29877,#29878);
#26478=AXIS2_PLACEMENT_3D('',#37208,#29879,#29880);
#26479=AXIS2_PLACEMENT_3D('',#37209,#29881,#29882);
#26480=AXIS2_PLACEMENT_3D('',#37212,#29885,#29886);
#26481=AXIS2_PLACEMENT_3D('',#37213,#29887,#29888);
#26482=AXIS2_PLACEMENT_3D('',#37216,#29891,#29892);
#26483=AXIS2_PLACEMENT_3D('',#37217,#29893,#29894);
#26484=AXIS2_PLACEMENT_3D('',#37218,#29895,#29896);
#26485=AXIS2_PLACEMENT_3D('',#37224,#29900,#29901);
#26486=AXIS2_PLACEMENT_3D('',#37225,#29902,#29903);
#26487=AXIS2_PLACEMENT_3D('',#37227,#29905,#29906);
#26488=AXIS2_PLACEMENT_3D('',#37233,#29909,#29910);
#26489=AXIS2_PLACEMENT_3D('',#37237,#29912,#29913);
#26490=AXIS2_PLACEMENT_3D('',#37241,#29915,#29916);
#26491=AXIS2_PLACEMENT_3D('',#37245,#29918,#29919);
#26492=AXIS2_PLACEMENT_3D('',#37247,#29920,#29921);
#26493=AXIS2_PLACEMENT_3D('',#37249,#29922,#29923);
#26494=AXIS2_PLACEMENT_3D('',#37253,#29925,#29926);
#26495=AXIS2_PLACEMENT_3D('',#37257,#29928,#29929);
#26496=AXIS2_PLACEMENT_3D('',#37261,#29931,#29932);
#26497=AXIS2_PLACEMENT_3D('',#37263,#29933,#29934);
#26498=AXIS2_PLACEMENT_3D('',#37265,#29935,#29936);
#26499=AXIS2_PLACEMENT_3D('',#37273,#29940,#29941);
#26500=AXIS2_PLACEMENT_3D('',#37275,#29942,#29943);
#26501=AXIS2_PLACEMENT_3D('',#37277,#29944,#29945);
#26502=AXIS2_PLACEMENT_3D('',#37281,#29947,#29948);
#26503=AXIS2_PLACEMENT_3D('',#37285,#29950,#29951);
#26504=AXIS2_PLACEMENT_3D('',#37289,#29953,#29954);
#26505=AXIS2_PLACEMENT_3D('',#37291,#29955,#29956);
#26506=AXIS2_PLACEMENT_3D('',#37293,#29957,#29958);
#26507=AXIS2_PLACEMENT_3D('',#37297,#29960,#29961);
#26508=AXIS2_PLACEMENT_3D('',#37301,#29963,#29964);
#26509=AXIS2_PLACEMENT_3D('',#37305,#29966,#29967);
#26510=AXIS2_PLACEMENT_3D('',#37312,#29972,#29973);
#26511=AXIS2_PLACEMENT_3D('',#37319,#29977,#29978);
#26512=AXIS2_PLACEMENT_3D('',#37323,#29980,#29981);
#26513=AXIS2_PLACEMENT_3D('',#37327,#29983,#29984);
#26514=AXIS2_PLACEMENT_3D('',#37331,#29986,#29987);
#26515=AXIS2_PLACEMENT_3D('',#37333,#29988,#29989);
#26516=AXIS2_PLACEMENT_3D('',#37335,#29990,#29991);
#26517=AXIS2_PLACEMENT_3D('',#37339,#29993,#29994);
#26518=AXIS2_PLACEMENT_3D('',#37343,#29996,#29997);
#26519=AXIS2_PLACEMENT_3D('',#37347,#29999,#30000);
#26520=AXIS2_PLACEMENT_3D('',#37349,#30001,#30002);
#26521=AXIS2_PLACEMENT_3D('',#37351,#30003,#30004);
#26522=AXIS2_PLACEMENT_3D('',#37359,#30008,#30009);
#26523=AXIS2_PLACEMENT_3D('',#37361,#30010,#30011);
#26524=AXIS2_PLACEMENT_3D('',#37363,#30012,#30013);
#26525=AXIS2_PLACEMENT_3D('',#37367,#30015,#30016);
#26526=AXIS2_PLACEMENT_3D('',#37371,#30018,#30019);
#26527=AXIS2_PLACEMENT_3D('',#37375,#30021,#30022);
#26528=AXIS2_PLACEMENT_3D('',#37377,#30023,#30024);
#26529=AXIS2_PLACEMENT_3D('',#37379,#30025,#30026);
#26530=AXIS2_PLACEMENT_3D('',#37383,#30028,#30029);
#26531=AXIS2_PLACEMENT_3D('',#37387,#30031,#30032);
#26532=AXIS2_PLACEMENT_3D('',#37391,#30034,#30035);
#26533=AXIS2_PLACEMENT_3D('',#37395,#30038,#30039);
#26534=AXIS2_PLACEMENT_3D('',#37398,#30042,#30043);
#26535=AXIS2_PLACEMENT_3D('',#37401,#30046,#30047);
#26536=AXIS2_PLACEMENT_3D('',#37404,#30050,#30051);
#26537=AXIS2_PLACEMENT_3D('',#37407,#30054,#30055);
#26538=AXIS2_PLACEMENT_3D('',#37410,#30058,#30059);
#26539=AXIS2_PLACEMENT_3D('',#37413,#30062,#30063);
#26540=AXIS2_PLACEMENT_3D('',#37415,#30065,#30066);
#26541=AXIS2_PLACEMENT_3D('',#37417,#30068,#30069);
#26542=AXIS2_PLACEMENT_3D('',#37419,#30071,#30072);
#26543=AXIS2_PLACEMENT_3D('',#37422,#30075,#30076);
#26544=AXIS2_PLACEMENT_3D('',#37425,#30079,#30080);
#26545=AXIS2_PLACEMENT_3D('',#37428,#30083,#30084);
#26546=AXIS2_PLACEMENT_3D('',#37431,#30087,#30088);
#26547=AXIS2_PLACEMENT_3D('',#37433,#30090,#30091);
#26548=AXIS2_PLACEMENT_3D('',#37436,#30094,#30095);
#26549=AXIS2_PLACEMENT_3D('',#37439,#30098,#30099);
#26550=AXIS2_PLACEMENT_3D('',#37440,#30100,#30101);
#26551=AXIS2_PLACEMENT_3D('',#37441,#30102,#30103);
#26552=AXIS2_PLACEMENT_3D('',#37442,#30104,#30105);
#26553=AXIS2_PLACEMENT_3D('',#37443,#30106,#30107);
#26554=AXIS2_PLACEMENT_3D('',#37444,#30108,#30109);
#26555=AXIS2_PLACEMENT_3D('',#37445,#30110,#30111);
#26556=AXIS2_PLACEMENT_3D('',#37446,#30112,#30113);
#26557=AXIS2_PLACEMENT_3D('',#37447,#30114,#30115);
#26558=AXIS2_PLACEMENT_3D('',#37448,#30116,#30117);
#26559=AXIS2_PLACEMENT_3D('',#37451,#30120,#30121);
#26560=AXIS2_PLACEMENT_3D('',#37454,#30124,#30125);
#26561=AXIS2_PLACEMENT_3D('',#37457,#30128,#30129);
#26562=AXIS2_PLACEMENT_3D('',#37460,#30132,#30133);
#26563=AXIS2_PLACEMENT_3D('',#37461,#30134,#30135);
#26564=AXIS2_PLACEMENT_3D('',#37464,#30138,#30139);
#26565=AXIS2_PLACEMENT_3D('',#37467,#30142,#30143);
#26566=AXIS2_PLACEMENT_3D('',#37468,#30144,#30145);
#26567=AXIS2_PLACEMENT_3D('',#37469,#30146,#30147);
#26568=AXIS2_PLACEMENT_3D('',#37470,#30148,#30149);
#26569=AXIS2_PLACEMENT_3D('',#37471,#30150,#30151);
#26570=AXIS2_PLACEMENT_3D('',#37472,#30152,#30153);
#26571=AXIS2_PLACEMENT_3D('',#37473,#30154,#30155);
#26572=AXIS2_PLACEMENT_3D('',#37474,#30156,#30157);
#26573=AXIS2_PLACEMENT_3D('',#37475,#30158,#30159);
#26574=AXIS2_PLACEMENT_3D('',#37476,#30160,#30161);
#26575=AXIS2_PLACEMENT_3D('',#37477,#30162,#30163);
#26576=AXIS2_PLACEMENT_3D('',#37479,#30165,#30166);
#26577=AXIS2_PLACEMENT_3D('',#37480,#30167,#30168);
#26578=AXIS2_PLACEMENT_3D('',#37481,#30169,#30170);
#26579=AXIS2_PLACEMENT_3D('',#37482,#30171,#30172);
#26580=AXIS2_PLACEMENT_3D('',#37483,#30173,#30174);
#26581=AXIS2_PLACEMENT_3D('',#37484,#30175,#30176);
#26582=AXIS2_PLACEMENT_3D('',#37485,#30177,#30178);
#26583=AXIS2_PLACEMENT_3D('',#37486,#30179,#30180);
#26584=AXIS2_PLACEMENT_3D('',#37487,#30181,#30182);
#26585=AXIS2_PLACEMENT_3D('',#37488,#30183,#30184);
#26586=AXIS2_PLACEMENT_3D('',#37489,#30185,#30186);
#26587=AXIS2_PLACEMENT_3D('',#37490,#30187,#30188);
#26588=AXIS2_PLACEMENT_3D('',#37491,#30189,#30190);
#26589=AXIS2_PLACEMENT_3D('',#37492,#30191,#30192);
#26590=AXIS2_PLACEMENT_3D('',#37493,#30193,#30194);
#26591=AXIS2_PLACEMENT_3D('',#37494,#30195,#30196);
#26592=AXIS2_PLACEMENT_3D('',#37495,#30197,#30198);
#26593=AXIS2_PLACEMENT_3D('',#37496,#30199,#30200);
#26594=AXIS2_PLACEMENT_3D('',#37498,#30201,#30202);
#26595=AXIS2_PLACEMENT_3D('',#37501,#30204,#30205);
#26596=AXIS2_PLACEMENT_3D('',#37502,#30206,#30207);
#26597=AXIS2_PLACEMENT_3D('',#37504,#30208,#30209);
#26598=AXIS2_PLACEMENT_3D('',#37507,#30211,#30212);
#26599=AXIS2_PLACEMENT_3D('',#37508,#30213,#30214);
#26600=AXIS2_PLACEMENT_3D('',#37510,#30215,#30216);
#26601=AXIS2_PLACEMENT_3D('',#37513,#30218,#30219);
#26602=AXIS2_PLACEMENT_3D('',#37514,#30220,#30221);
#26603=AXIS2_PLACEMENT_3D('',#37517,#30223,#30224);
#26604=AXIS2_PLACEMENT_3D('',#37520,#30226,#30227);
#26605=AXIS2_PLACEMENT_3D('',#37522,#30228,#30229);
#26606=AXIS2_PLACEMENT_3D('',#37525,#30231,#30232);
#26607=AXIS2_PLACEMENT_3D('',#37526,#30233,#30234);
#26608=AXIS2_PLACEMENT_3D('',#37528,#30235,#30236);
#26609=AXIS2_PLACEMENT_3D('',#37531,#30238,#30239);
#26610=AXIS2_PLACEMENT_3D('',#37532,#30240,#30241);
#26611=AXIS2_PLACEMENT_3D('',#37534,#30242,#30243);
#26612=AXIS2_PLACEMENT_3D('',#37537,#30245,#30246);
#26613=AXIS2_PLACEMENT_3D('',#37538,#30247,#30248);
#26614=AXIS2_PLACEMENT_3D('',#37540,#30249,#30250);
#26615=AXIS2_PLACEMENT_3D('',#37543,#30252,#30253);
#26616=AXIS2_PLACEMENT_3D('',#37544,#30254,#30255);
#26617=AXIS2_PLACEMENT_3D('',#37546,#30256,#30257);
#26618=AXIS2_PLACEMENT_3D('',#37549,#30259,#30260);
#26619=AXIS2_PLACEMENT_3D('',#37550,#30261,#30262);
#26620=AXIS2_PLACEMENT_3D('',#37552,#30263,#30264);
#26621=AXIS2_PLACEMENT_3D('',#37555,#30266,#30267);
#26622=AXIS2_PLACEMENT_3D('',#37556,#30268,#30269);
#26623=AXIS2_PLACEMENT_3D('',#37558,#30270,#30271);
#26624=AXIS2_PLACEMENT_3D('',#37561,#30273,#30274);
#26625=AXIS2_PLACEMENT_3D('',#37562,#30275,#30276);
#26626=AXIS2_PLACEMENT_3D('',#37564,#30277,#30278);
#26627=AXIS2_PLACEMENT_3D('',#37568,#30280,#30281);
#26628=AXIS2_PLACEMENT_3D('',#37572,#30283,#30284);
#26629=AXIS2_PLACEMENT_3D('',#37574,#30286,#30287);
#26630=AXIS2_PLACEMENT_3D('',#37577,#30289,#30290);
#26631=AXIS2_PLACEMENT_3D('',#37580,#30292,#30293);
#26632=AXIS2_PLACEMENT_3D('',#37582,#30294,#30295);
#26633=AXIS2_PLACEMENT_3D('',#37588,#30298,#30299);
#26634=AXIS2_PLACEMENT_3D('',#37591,#30301,#30302);
#26635=AXIS2_PLACEMENT_3D('',#37658,#30303,#30304);
#26636=AXIS2_PLACEMENT_3D('',#37659,#30305,#30306);
#26637=AXIS2_PLACEMENT_3D('',#37692,#30307,#30308);
#26638=AXIS2_PLACEMENT_3D('',#37694,#30309,#30310);
#26639=AXIS2_PLACEMENT_3D('',#37696,#30312,#30313);
#26640=AXIS2_PLACEMENT_3D('',#37698,#30314,#30315);
#26641=AXIS2_PLACEMENT_3D('',#37701,#30317,#30318);
#26642=AXIS2_PLACEMENT_3D('',#37702,#30319,#30320);
#26643=AXIS2_PLACEMENT_3D('',#37705,#30321,#30322);
#26644=AXIS2_PLACEMENT_3D('',#37711,#30326,#30327);
#26645=AXIS2_PLACEMENT_3D('',#37713,#30328,#30329);
#26646=AXIS2_PLACEMENT_3D('',#37717,#30331,#30332);
#26647=AXIS2_PLACEMENT_3D('',#37719,#30334,#30335);
#26648=AXIS2_PLACEMENT_3D('',#37722,#30336,#30337);
#26649=AXIS2_PLACEMENT_3D('',#37726,#30339,#30340);
#26650=AXIS2_PLACEMENT_3D('',#37728,#30342,#30343);
#26651=AXIS2_PLACEMENT_3D('',#37730,#30344,#30345);
#26652=AXIS2_PLACEMENT_3D('',#37736,#30349,#30350);
#26653=AXIS2_PLACEMENT_3D('',#37745,#30355,#30356);
#26654=AXIS2_PLACEMENT_3D('',#37754,#30361,#30362);
#26655=AXIS2_PLACEMENT_3D('',#37763,#30367,#30368);
#26656=AXIS2_PLACEMENT_3D('',#37772,#30373,#30374);
#26657=AXIS2_PLACEMENT_3D('',#37781,#30379,#30380);
#26658=AXIS2_PLACEMENT_3D('',#37790,#30385,#30386);
#26659=AXIS2_PLACEMENT_3D('',#37799,#30391,#30392);
#26660=AXIS2_PLACEMENT_3D('',#37808,#30397,#30398);
#26661=AXIS2_PLACEMENT_3D('',#37817,#30403,#30404);
#26662=AXIS2_PLACEMENT_3D('',#37823,#30408,#30409);
#26663=AXIS2_PLACEMENT_3D('',#37832,#30414,#30415);
#26664=AXIS2_PLACEMENT_3D('',#37838,#30419,#30420);
#26665=AXIS2_PLACEMENT_3D('',#37847,#30425,#30426);
#26666=AXIS2_PLACEMENT_3D('',#37856,#30431,#30432);
#26667=AXIS2_PLACEMENT_3D('',#37865,#30437,#30438);
#26668=AXIS2_PLACEMENT_3D('',#37874,#30443,#30444);
#26669=AXIS2_PLACEMENT_3D('',#37877,#30447,#30448);
#26670=AXIS2_PLACEMENT_3D('',#37880,#30449,#30450);
#26671=AXIS2_PLACEMENT_3D('',#37884,#30452,#30453);
#26672=AXIS2_PLACEMENT_3D('',#37886,#30455,#30456);
#26673=AXIS2_PLACEMENT_3D('',#37889,#30457,#30458);
#26674=AXIS2_PLACEMENT_3D('',#37893,#30460,#30461);
#26675=AXIS2_PLACEMENT_3D('',#37895,#30463,#30464);
#26676=AXIS2_PLACEMENT_3D('',#37898,#30465,#30466);
#26677=AXIS2_PLACEMENT_3D('',#37902,#30468,#30469);
#26678=AXIS2_PLACEMENT_3D('',#37904,#30471,#30472);
#26679=AXIS2_PLACEMENT_3D('',#37907,#30473,#30474);
#26680=AXIS2_PLACEMENT_3D('',#37911,#30476,#30477);
#26681=AXIS2_PLACEMENT_3D('',#37913,#30479,#30480);
#26682=AXIS2_PLACEMENT_3D('',#37914,#30481,#30482);
#26683=AXIS2_PLACEMENT_3D('',#37915,#30483,#30484);
#26684=AXIS2_PLACEMENT_3D('',#37916,#30485,#30486);
#26685=AXIS2_PLACEMENT_3D('',#37917,#30487,#30488);
#26686=AXIS2_PLACEMENT_3D('',#37918,#30489,#30490);
#26687=AXIS2_PLACEMENT_3D('',#37919,#30491,#30492);
#26688=AXIS2_PLACEMENT_3D('',#37920,#30493,#30494);
#26689=AXIS2_PLACEMENT_3D('',#37921,#30495,#30496);
#26690=AXIS2_PLACEMENT_3D('',#37922,#30497,#30498);
#26691=AXIS2_PLACEMENT_3D('',#37923,#30499,#30500);
#26692=AXIS2_PLACEMENT_3D('',#37924,#30501,#30502);
#26693=AXIS2_PLACEMENT_3D('',#37925,#30503,#30504);
#26694=AXIS2_PLACEMENT_3D('',#37926,#30505,#30506);
#26695=AXIS2_PLACEMENT_3D('',#37927,#30507,#30508);
#26696=AXIS2_PLACEMENT_3D('',#37928,#30509,#30510);
#26697=AXIS2_PLACEMENT_3D('',#37929,#30511,#30512);
#26698=AXIS2_PLACEMENT_3D('',#37930,#30513,#30514);
#26699=AXIS2_PLACEMENT_3D('',#37931,#30515,#30516);
#26700=AXIS2_PLACEMENT_3D('',#37932,#30517,#30518);
#26701=AXIS2_PLACEMENT_3D('',#37933,#30519,#30520);
#26702=AXIS2_PLACEMENT_3D('',#37934,#30521,#30522);
#26703=AXIS2_PLACEMENT_3D('',#37935,#30523,#30524);
#26704=AXIS2_PLACEMENT_3D('',#37936,#30525,#30526);
#26705=AXIS2_PLACEMENT_3D('',#37937,#30527,#30528);
#26706=AXIS2_PLACEMENT_3D('',#37938,#30529,#30530);
#26707=AXIS2_PLACEMENT_3D('',#37939,#30531,#30532);
#26708=AXIS2_PLACEMENT_3D('',#37940,#30533,#30534);
#26709=AXIS2_PLACEMENT_3D('',#37941,#30535,#30536);
#26710=AXIS2_PLACEMENT_3D('',#37942,#30537,#30538);
#26711=AXIS2_PLACEMENT_3D('',#37943,#30539,#30540);
#26712=AXIS2_PLACEMENT_3D('',#37944,#30541,#30542);
#26713=AXIS2_PLACEMENT_3D('',#37945,#30543,#30544);
#26714=AXIS2_PLACEMENT_3D('',#37946,#30545,#30546);
#26715=AXIS2_PLACEMENT_3D('',#37947,#30547,#30548);
#26716=AXIS2_PLACEMENT_3D('',#37948,#30549,#30550);
#26717=AXIS2_PLACEMENT_3D('',#37949,#30551,#30552);
#26718=AXIS2_PLACEMENT_3D('',#37950,#30553,#30554);
#26719=AXIS2_PLACEMENT_3D('',#37951,#30555,#30556);
#26720=AXIS2_PLACEMENT_3D('',#37952,#30557,#30558);
#26721=AXIS2_PLACEMENT_3D('',#37953,#30559,#30560);
#26722=AXIS2_PLACEMENT_3D('',#37954,#30561,#30562);
#26723=AXIS2_PLACEMENT_3D('',#37955,#30563,#30564);
#26724=AXIS2_PLACEMENT_3D('',#37956,#30565,#30566);
#26725=AXIS2_PLACEMENT_3D('',#37957,#30567,#30568);
#26726=AXIS2_PLACEMENT_3D('',#37958,#30569,#30570);
#26727=AXIS2_PLACEMENT_3D('',#37959,#30571,#30572);
#26728=AXIS2_PLACEMENT_3D('',#37960,#30573,#30574);
#26729=AXIS2_PLACEMENT_3D('',#37961,#30575,#30576);
#26730=AXIS2_PLACEMENT_3D('',#37962,#30577,#30578);
#26731=AXIS2_PLACEMENT_3D('',#37971,#30583,#30584);
#26732=AXIS2_PLACEMENT_3D('',#37982,#30591,#30592);
#26733=AXIS2_PLACEMENT_3D('',#37986,#30595,#30596);
#26734=AXIS2_PLACEMENT_3D('',#37990,#30599,#30600);
#26735=AXIS2_PLACEMENT_3D('',#37992,#30602,#30603);
#26736=AXIS2_PLACEMENT_3D('',#37996,#30606,#30607);
#26737=AXIS2_PLACEMENT_3D('',#38000,#30610,#30611);
#26738=AXIS2_PLACEMENT_3D('',#38002,#30613,#30614);
#26739=AXIS2_PLACEMENT_3D('',#38008,#30618,#30619);
#26740=AXIS2_PLACEMENT_3D('',#38012,#30622,#30623);
#26741=AXIS2_PLACEMENT_3D('',#38016,#30626,#30627);
#26742=AXIS2_PLACEMENT_3D('',#38020,#30630,#30631);
#26743=AXIS2_PLACEMENT_3D('',#38024,#30634,#30635);
#26744=AXIS2_PLACEMENT_3D('',#38026,#30637,#30638);
#26745=AXIS2_PLACEMENT_3D('',#38027,#30639,#30640);
#26746=AXIS2_PLACEMENT_3D('',#38032,#30642,#30643);
#26747=AXIS2_PLACEMENT_3D('',#38036,#30645,#30646);
#26748=AXIS2_PLACEMENT_3D('',#38040,#30648,#30649);
#26749=AXIS2_PLACEMENT_3D('',#38042,#30650,#30651);
#26750=AXIS2_PLACEMENT_3D('',#38044,#30652,#30653);
#26751=AXIS2_PLACEMENT_3D('',#38048,#30655,#30656);
#26752=AXIS2_PLACEMENT_3D('',#38052,#30658,#30659);
#26753=AXIS2_PLACEMENT_3D('',#38056,#30661,#30662);
#26754=AXIS2_PLACEMENT_3D('',#38058,#30663,#30664);
#26755=AXIS2_PLACEMENT_3D('',#38060,#30665,#30666);
#26756=AXIS2_PLACEMENT_3D('',#38068,#30670,#30671);
#26757=AXIS2_PLACEMENT_3D('',#38070,#30672,#30673);
#26758=AXIS2_PLACEMENT_3D('',#38072,#30674,#30675);
#26759=AXIS2_PLACEMENT_3D('',#38076,#30677,#30678);
#26760=AXIS2_PLACEMENT_3D('',#38080,#30680,#30681);
#26761=AXIS2_PLACEMENT_3D('',#38084,#30683,#30684);
#26762=AXIS2_PLACEMENT_3D('',#38086,#30685,#30686);
#26763=AXIS2_PLACEMENT_3D('',#38088,#30687,#30688);
#26764=AXIS2_PLACEMENT_3D('',#38092,#30690,#30691);
#26765=AXIS2_PLACEMENT_3D('',#38096,#30693,#30694);
#26766=AXIS2_PLACEMENT_3D('',#38116,#30705,#30706);
#26767=AXIS2_PLACEMENT_3D('',#38122,#30710,#30711);
#26768=AXIS2_PLACEMENT_3D('',#38124,#30712,#30713);
#26769=AXIS2_PLACEMENT_3D('',#38126,#30715,#30716);
#26770=AXIS2_PLACEMENT_3D('',#38130,#30719,#30720);
#26771=AXIS2_PLACEMENT_3D('',#38132,#30721,#30722);
#26772=AXIS2_PLACEMENT_3D('',#38134,#30724,#30725);
#26773=AXIS2_PLACEMENT_3D('',#38138,#30728,#30729);
#26774=AXIS2_PLACEMENT_3D('',#38140,#30730,#30731);
#26775=AXIS2_PLACEMENT_3D('',#38142,#30733,#30734);
#26776=AXIS2_PLACEMENT_3D('',#38144,#30735,#30736);
#26777=AXIS2_PLACEMENT_3D('',#38146,#30738,#30739);
#26778=AXIS2_PLACEMENT_3D('',#38148,#30740,#30741);
#26779=AXIS2_PLACEMENT_3D('',#38150,#30743,#30744);
#26780=AXIS2_PLACEMENT_3D('',#38154,#30747,#30748);
#26781=AXIS2_PLACEMENT_3D('',#38156,#30749,#30750);
#26782=AXIS2_PLACEMENT_3D('',#38158,#30752,#30753);
#26783=AXIS2_PLACEMENT_3D('',#38162,#30756,#30757);
#26784=AXIS2_PLACEMENT_3D('',#38164,#30758,#30759);
#26785=AXIS2_PLACEMENT_3D('',#38166,#30761,#30762);
#26786=AXIS2_PLACEMENT_3D('',#38170,#30765,#30766);
#26787=AXIS2_PLACEMENT_3D('',#38172,#30767,#30768);
#26788=AXIS2_PLACEMENT_3D('',#38174,#30770,#30771);
#26789=AXIS2_PLACEMENT_3D('',#38176,#30772,#30773);
#26790=AXIS2_PLACEMENT_3D('',#38178,#30775,#30776);
#26791=AXIS2_PLACEMENT_3D('',#38180,#30777,#30778);
#26792=AXIS2_PLACEMENT_3D('',#38182,#30780,#30781);
#26793=AXIS2_PLACEMENT_3D('',#38186,#30784,#30785);
#26794=AXIS2_PLACEMENT_3D('',#38190,#30788,#30789);
#26795=AXIS2_PLACEMENT_3D('',#38194,#30792,#30793);
#26796=AXIS2_PLACEMENT_3D('',#38196,#30794,#30795);
#26797=AXIS2_PLACEMENT_3D('',#38198,#30797,#30798);
#26798=AXIS2_PLACEMENT_3D('',#38200,#30799,#30800);
#26799=AXIS2_PLACEMENT_3D('',#38202,#30802,#30803);
#26800=AXIS2_PLACEMENT_3D('',#38204,#30804,#30805);
#26801=AXIS2_PLACEMENT_3D('',#38206,#30807,#30808);
#26802=AXIS2_PLACEMENT_3D('',#38210,#30811,#30812);
#26803=AXIS2_PLACEMENT_3D('',#38212,#30813,#30814);
#26804=AXIS2_PLACEMENT_3D('',#38214,#30816,#30817);
#26805=AXIS2_PLACEMENT_3D('',#38218,#30820,#30821);
#26806=AXIS2_PLACEMENT_3D('',#38220,#30822,#30823);
#26807=AXIS2_PLACEMENT_3D('',#38222,#30825,#30826);
#26808=AXIS2_PLACEMENT_3D('',#38226,#30829,#30830);
#26809=AXIS2_PLACEMENT_3D('',#38228,#30831,#30832);
#26810=AXIS2_PLACEMENT_3D('',#38230,#30834,#30835);
#26811=AXIS2_PLACEMENT_3D('',#38232,#30836,#30837);
#26812=AXIS2_PLACEMENT_3D('',#38234,#30839,#30840);
#26813=AXIS2_PLACEMENT_3D('',#38236,#30841,#30842);
#26814=AXIS2_PLACEMENT_3D('',#38238,#30844,#30845);
#26815=AXIS2_PLACEMENT_3D('',#38242,#30848,#30849);
#26816=AXIS2_PLACEMENT_3D('',#38244,#30850,#30851);
#26817=AXIS2_PLACEMENT_3D('',#38246,#30853,#30854);
#26818=AXIS2_PLACEMENT_3D('',#38250,#30857,#30858);
#26819=AXIS2_PLACEMENT_3D('',#38252,#30859,#30860);
#26820=AXIS2_PLACEMENT_3D('',#38254,#30862,#30863);
#26821=AXIS2_PLACEMENT_3D('',#38258,#30866,#30867);
#26822=AXIS2_PLACEMENT_3D('',#38262,#30870,#30871);
#26823=AXIS2_PLACEMENT_3D('',#38266,#30874,#30875);
#26824=AXIS2_PLACEMENT_3D('',#38270,#30878,#30879);
#26825=AXIS2_PLACEMENT_3D('',#38274,#30882,#30883);
#26826=AXIS2_PLACEMENT_3D('',#38278,#30886,#30887);
#26827=AXIS2_PLACEMENT_3D('',#38282,#30890,#30891);
#26828=AXIS2_PLACEMENT_3D('',#38286,#30894,#30895);
#26829=AXIS2_PLACEMENT_3D('',#38290,#30898,#30899);
#26830=AXIS2_PLACEMENT_3D('',#38292,#30901,#30902);
#26831=AXIS2_PLACEMENT_3D('',#38293,#30903,#30904);
#26832=AXIS2_PLACEMENT_3D('',#38297,#30906,#30907);
#26833=AXIS2_PLACEMENT_3D('',#38299,#30909,#30910);
#26834=AXIS2_PLACEMENT_3D('',#38306,#30913,#30914);
#26835=AXIS2_PLACEMENT_3D('',#38322,#30922,#30923);
#26836=AXIS2_PLACEMENT_3D('',#38326,#30925,#30926);
#26837=AXIS2_PLACEMENT_3D('',#38330,#30928,#30929);
#26838=AXIS2_PLACEMENT_3D('',#38332,#30930,#30931);
#26839=AXIS2_PLACEMENT_3D('',#38334,#30932,#30933);
#26840=AXIS2_PLACEMENT_3D('',#38338,#30935,#30936);
#26841=AXIS2_PLACEMENT_3D('',#38342,#30938,#30939);
#26842=AXIS2_PLACEMENT_3D('',#38346,#30941,#30942);
#26843=AXIS2_PLACEMENT_3D('',#38348,#30943,#30944);
#26844=AXIS2_PLACEMENT_3D('',#38350,#30945,#30946);
#26845=AXIS2_PLACEMENT_3D('',#38358,#30950,#30951);
#26846=AXIS2_PLACEMENT_3D('',#38360,#30952,#30953);
#26847=AXIS2_PLACEMENT_3D('',#38362,#30954,#30955);
#26848=AXIS2_PLACEMENT_3D('',#38366,#30957,#30958);
#26849=AXIS2_PLACEMENT_3D('',#38370,#30960,#30961);
#26850=AXIS2_PLACEMENT_3D('',#38374,#30963,#30964);
#26851=AXIS2_PLACEMENT_3D('',#38376,#30965,#30966);
#26852=AXIS2_PLACEMENT_3D('',#38378,#30967,#30968);
#26853=AXIS2_PLACEMENT_3D('',#38382,#30970,#30971);
#26854=AXIS2_PLACEMENT_3D('',#38386,#30973,#30974);
#26855=AXIS2_PLACEMENT_3D('',#38396,#30980,#30981);
#26856=AXIS2_PLACEMENT_3D('',#38400,#30984,#30985);
#26857=AXIS2_PLACEMENT_3D('',#38404,#30988,#30989);
#26858=AXIS2_PLACEMENT_3D('',#38405,#30990,#30991);
#26859=AXIS2_PLACEMENT_3D('',#38406,#30992,#30993);
#26860=AXIS2_PLACEMENT_3D('',#38407,#30994,#30995);
#26861=AXIS2_PLACEMENT_3D('',#38411,#30997,#30998);
#26862=AXIS2_PLACEMENT_3D('',#38413,#31000,#31001);
#26863=AXIS2_PLACEMENT_3D('',#38419,#31005,#31006);
#26864=AXIS2_PLACEMENT_3D('',#38423,#31009,#31010);
#26865=AXIS2_PLACEMENT_3D('',#38427,#31013,#31014);
#26866=AXIS2_PLACEMENT_3D('',#38431,#31017,#31018);
#26867=AXIS2_PLACEMENT_3D('',#38440,#31024,#31025);
#26868=AXIS2_PLACEMENT_3D('',#38444,#31028,#31029);
#26869=AXIS2_PLACEMENT_3D('',#38448,#31032,#31033);
#26870=AXIS2_PLACEMENT_3D('',#38452,#31036,#31037);
#26871=AXIS2_PLACEMENT_3D('',#38456,#31040,#31041);
#26872=AXIS2_PLACEMENT_3D('',#38460,#31044,#31045);
#26873=AXIS2_PLACEMENT_3D('',#38462,#31046,#31047);
#26874=AXIS2_PLACEMENT_3D('',#38464,#31049,#31050);
#26875=AXIS2_PLACEMENT_3D('',#38468,#31053,#31054);
#26876=AXIS2_PLACEMENT_3D('',#38470,#31055,#31056);
#26877=AXIS2_PLACEMENT_3D('',#38472,#31058,#31059);
#26878=AXIS2_PLACEMENT_3D('',#38476,#31062,#31063);
#26879=AXIS2_PLACEMENT_3D('',#38478,#31064,#31065);
#26880=AXIS2_PLACEMENT_3D('',#38480,#31067,#31068);
#26881=AXIS2_PLACEMENT_3D('',#38482,#31069,#31070);
#26882=AXIS2_PLACEMENT_3D('',#38484,#31072,#31073);
#26883=AXIS2_PLACEMENT_3D('',#38486,#31074,#31075);
#26884=AXIS2_PLACEMENT_3D('',#38488,#31077,#31078);
#26885=AXIS2_PLACEMENT_3D('',#38492,#31081,#31082);
#26886=AXIS2_PLACEMENT_3D('',#38494,#31083,#31084);
#26887=AXIS2_PLACEMENT_3D('',#38496,#31086,#31087);
#26888=AXIS2_PLACEMENT_3D('',#38500,#31090,#31091);
#26889=AXIS2_PLACEMENT_3D('',#38502,#31092,#31093);
#26890=AXIS2_PLACEMENT_3D('',#38504,#31095,#31096);
#26891=AXIS2_PLACEMENT_3D('',#38508,#31099,#31100);
#26892=AXIS2_PLACEMENT_3D('',#38510,#31101,#31102);
#26893=AXIS2_PLACEMENT_3D('',#38512,#31104,#31105);
#26894=AXIS2_PLACEMENT_3D('',#38514,#31106,#31107);
#26895=AXIS2_PLACEMENT_3D('',#38516,#31109,#31110);
#26896=AXIS2_PLACEMENT_3D('',#38518,#31111,#31112);
#26897=AXIS2_PLACEMENT_3D('',#38520,#31114,#31115);
#26898=AXIS2_PLACEMENT_3D('',#38524,#31118,#31119);
#26899=AXIS2_PLACEMENT_3D('',#38528,#31122,#31123);
#26900=AXIS2_PLACEMENT_3D('',#38532,#31126,#31127);
#26901=AXIS2_PLACEMENT_3D('',#38534,#31128,#31129);
#26902=AXIS2_PLACEMENT_3D('',#38536,#31131,#31132);
#26903=AXIS2_PLACEMENT_3D('',#38538,#31133,#31134);
#26904=AXIS2_PLACEMENT_3D('',#38540,#31136,#31137);
#26905=AXIS2_PLACEMENT_3D('',#38542,#31138,#31139);
#26906=AXIS2_PLACEMENT_3D('',#38544,#31141,#31142);
#26907=AXIS2_PLACEMENT_3D('',#38548,#31145,#31146);
#26908=AXIS2_PLACEMENT_3D('',#38550,#31147,#31148);
#26909=AXIS2_PLACEMENT_3D('',#38552,#31150,#31151);
#26910=AXIS2_PLACEMENT_3D('',#38556,#31154,#31155);
#26911=AXIS2_PLACEMENT_3D('',#38558,#31156,#31157);
#26912=AXIS2_PLACEMENT_3D('',#38560,#31159,#31160);
#26913=AXIS2_PLACEMENT_3D('',#38564,#31163,#31164);
#26914=AXIS2_PLACEMENT_3D('',#38566,#31165,#31166);
#26915=AXIS2_PLACEMENT_3D('',#38568,#31168,#31169);
#26916=AXIS2_PLACEMENT_3D('',#38570,#31170,#31171);
#26917=AXIS2_PLACEMENT_3D('',#38572,#31173,#31174);
#26918=AXIS2_PLACEMENT_3D('',#38574,#31175,#31176);
#26919=AXIS2_PLACEMENT_3D('',#38576,#31178,#31179);
#26920=AXIS2_PLACEMENT_3D('',#38580,#31182,#31183);
#26921=AXIS2_PLACEMENT_3D('',#38582,#31184,#31185);
#26922=AXIS2_PLACEMENT_3D('',#38584,#31187,#31188);
#26923=AXIS2_PLACEMENT_3D('',#38588,#31191,#31192);
#26924=AXIS2_PLACEMENT_3D('',#38590,#31193,#31194);
#26925=AXIS2_PLACEMENT_3D('',#38592,#31196,#31197);
#26926=AXIS2_PLACEMENT_3D('',#38594,#31199,#31200);
#26927=AXIS2_PLACEMENT_3D('',#38595,#31201,#31202);
#26928=AXIS2_PLACEMENT_3D('',#38604,#31207,#31208);
#26929=AXIS2_PLACEMENT_3D('',#38613,#31213,#31214);
#26930=AXIS2_PLACEMENT_3D('',#38617,#31217,#31218);
#26931=AXIS2_PLACEMENT_3D('',#38621,#31221,#31222);
#26932=AXIS2_PLACEMENT_3D('',#38622,#31223,#31224);
#26933=AXIS2_PLACEMENT_3D('',#38623,#31225,#31226);
#26934=AXIS2_PLACEMENT_3D('',#38625,#31227,#31228);
#26935=AXIS2_PLACEMENT_3D('',#38627,#31229,#31230);
#26936=AXIS2_PLACEMENT_3D('',#38629,#31232,#31233);
#26937=AXIS2_PLACEMENT_3D('',#38637,#31238,#31239);
#26938=AXIS2_PLACEMENT_3D('',#38643,#31243,#31244);
#26939=AXIS2_PLACEMENT_3D('',#38652,#31249,#31250);
#26940=AXIS2_PLACEMENT_3D('',#38655,#31252,#31253);
#26941=AXIS2_PLACEMENT_3D('',#38659,#31256,#31257);
#26942=AXIS2_PLACEMENT_3D('',#38662,#31259,#31260);
#26943=AXIS2_PLACEMENT_3D('',#38663,#31261,#31262);
#26944=AXIS2_PLACEMENT_3D('',#38686,#31273,#31274);
#26945=AXIS2_PLACEMENT_3D('',#38690,#31276,#31277);
#26946=AXIS2_PLACEMENT_3D('',#38694,#31279,#31280);
#26947=AXIS2_PLACEMENT_3D('',#38696,#31281,#31282);
#26948=AXIS2_PLACEMENT_3D('',#38698,#31283,#31284);
#26949=AXIS2_PLACEMENT_3D('',#38702,#31286,#31287);
#26950=AXIS2_PLACEMENT_3D('',#38706,#31289,#31290);
#26951=AXIS2_PLACEMENT_3D('',#38710,#31292,#31293);
#26952=AXIS2_PLACEMENT_3D('',#38712,#31294,#31295);
#26953=AXIS2_PLACEMENT_3D('',#38714,#31296,#31297);
#26954=AXIS2_PLACEMENT_3D('',#38722,#31301,#31302);
#26955=AXIS2_PLACEMENT_3D('',#38724,#31303,#31304);
#26956=AXIS2_PLACEMENT_3D('',#38726,#31305,#31306);
#26957=AXIS2_PLACEMENT_3D('',#38730,#31308,#31309);
#26958=AXIS2_PLACEMENT_3D('',#38734,#31311,#31312);
#26959=AXIS2_PLACEMENT_3D('',#38738,#31314,#31315);
#26960=AXIS2_PLACEMENT_3D('',#38740,#31316,#31317);
#26961=AXIS2_PLACEMENT_3D('',#38742,#31318,#31319);
#26962=AXIS2_PLACEMENT_3D('',#38746,#31321,#31322);
#26963=AXIS2_PLACEMENT_3D('',#38750,#31324,#31325);
#26964=AXIS2_PLACEMENT_3D('',#38752,#31327,#31328);
#26965=AXIS2_PLACEMENT_3D('',#38756,#31331,#31332);
#26966=AXIS2_PLACEMENT_3D('',#38760,#31335,#31336);
#26967=AXIS2_PLACEMENT_3D('',#38766,#31340,#31341);
#26968=AXIS2_PLACEMENT_3D('',#38772,#31345,#31346);
#26969=AXIS2_PLACEMENT_3D('',#38778,#31350,#31351);
#26970=AXIS2_PLACEMENT_3D('',#38784,#31355,#31356);
#26971=AXIS2_PLACEMENT_3D('',#38785,#31357,#31358);
#26972=AXIS2_PLACEMENT_3D('',#38786,#31359,#31360);
#26973=AXIS2_PLACEMENT_3D('',#38787,#31361,#31362);
#26974=AXIS2_PLACEMENT_3D('',#38788,#31363,#31364);
#26975=AXIS2_PLACEMENT_3D('',#38790,#31365,#31366);
#26976=AXIS2_PLACEMENT_3D('',#38796,#31370,#31371);
#26977=AXIS2_PLACEMENT_3D('',#38802,#31375,#31376);
#26978=AXIS2_PLACEMENT_3D('',#38804,#31377,#31378);
#26979=AXIS2_PLACEMENT_3D('',#38808,#31381,#31382);
#26980=AXIS2_PLACEMENT_3D('',#38814,#31386,#31387);
#26981=AXIS2_PLACEMENT_3D('',#38818,#31390,#31391);
#26982=AXIS2_PLACEMENT_3D('',#38819,#31392,#31393);
#26983=AXIS2_PLACEMENT_3D('',#38821,#31394,#31395);
#26984=AXIS2_PLACEMENT_3D('',#38825,#31398,#31399);
#26985=AXIS2_PLACEMENT_3D('',#38826,#31400,#31401);
#26986=AXIS2_PLACEMENT_3D('',#38827,#31402,#31403);
#26987=AXIS2_PLACEMENT_3D('',#38828,#31404,#31405);
#26988=AXIS2_PLACEMENT_3D('',#38834,#31409,#31410);
#26989=AXIS2_PLACEMENT_3D('',#38838,#31413,#31414);
#26990=AXIS2_PLACEMENT_3D('',#38842,#31417,#31418);
#26991=AXIS2_PLACEMENT_3D('',#38846,#31421,#31422);
#26992=AXIS2_PLACEMENT_3D('',#38850,#31425,#31426);
#26993=AXIS2_PLACEMENT_3D('',#38854,#31429,#31430);
#26994=AXIS2_PLACEMENT_3D('',#38858,#31433,#31434);
#26995=AXIS2_PLACEMENT_3D('',#38862,#31437,#31438);
#26996=AXIS2_PLACEMENT_3D('',#38866,#31441,#31442);
#26997=AXIS2_PLACEMENT_3D('',#38870,#31445,#31446);
#26998=AXIS2_PLACEMENT_3D('',#38872,#31447,#31448);
#26999=AXIS2_PLACEMENT_3D('',#38874,#31450,#31451);
#27000=AXIS2_PLACEMENT_3D('',#38878,#31454,#31455);
#27001=AXIS2_PLACEMENT_3D('',#38880,#31456,#31457);
#27002=AXIS2_PLACEMENT_3D('',#38882,#31459,#31460);
#27003=AXIS2_PLACEMENT_3D('',#38886,#31463,#31464);
#27004=AXIS2_PLACEMENT_3D('',#38888,#31465,#31466);
#27005=AXIS2_PLACEMENT_3D('',#38890,#31468,#31469);
#27006=AXIS2_PLACEMENT_3D('',#38892,#31470,#31471);
#27007=AXIS2_PLACEMENT_3D('',#38894,#31473,#31474);
#27008=AXIS2_PLACEMENT_3D('',#38896,#31475,#31476);
#27009=AXIS2_PLACEMENT_3D('',#38898,#31478,#31479);
#27010=AXIS2_PLACEMENT_3D('',#38902,#31482,#31483);
#27011=AXIS2_PLACEMENT_3D('',#38904,#31484,#31485);
#27012=AXIS2_PLACEMENT_3D('',#38906,#31487,#31488);
#27013=AXIS2_PLACEMENT_3D('',#38910,#31491,#31492);
#27014=AXIS2_PLACEMENT_3D('',#38912,#31493,#31494);
#27015=AXIS2_PLACEMENT_3D('',#38914,#31496,#31497);
#27016=AXIS2_PLACEMENT_3D('',#38918,#31500,#31501);
#27017=AXIS2_PLACEMENT_3D('',#38920,#31502,#31503);
#27018=AXIS2_PLACEMENT_3D('',#38922,#31505,#31506);
#27019=AXIS2_PLACEMENT_3D('',#38924,#31507,#31508);
#27020=AXIS2_PLACEMENT_3D('',#38926,#31510,#31511);
#27021=AXIS2_PLACEMENT_3D('',#38928,#31512,#31513);
#27022=AXIS2_PLACEMENT_3D('',#38930,#31515,#31516);
#27023=AXIS2_PLACEMENT_3D('',#38934,#31519,#31520);
#27024=AXIS2_PLACEMENT_3D('',#38938,#31523,#31524);
#27025=AXIS2_PLACEMENT_3D('',#38942,#31527,#31528);
#27026=AXIS2_PLACEMENT_3D('',#38944,#31529,#31530);
#27027=AXIS2_PLACEMENT_3D('',#38946,#31532,#31533);
#27028=AXIS2_PLACEMENT_3D('',#38948,#31534,#31535);
#27029=AXIS2_PLACEMENT_3D('',#38950,#31537,#31538);
#27030=AXIS2_PLACEMENT_3D('',#38952,#31539,#31540);
#27031=AXIS2_PLACEMENT_3D('',#38954,#31542,#31543);
#27032=AXIS2_PLACEMENT_3D('',#38958,#31546,#31547);
#27033=AXIS2_PLACEMENT_3D('',#38960,#31548,#31549);
#27034=AXIS2_PLACEMENT_3D('',#38962,#31551,#31552);
#27035=AXIS2_PLACEMENT_3D('',#38966,#31555,#31556);
#27036=AXIS2_PLACEMENT_3D('',#38968,#31557,#31558);
#27037=AXIS2_PLACEMENT_3D('',#38970,#31560,#31561);
#27038=AXIS2_PLACEMENT_3D('',#38974,#31564,#31565);
#27039=AXIS2_PLACEMENT_3D('',#38976,#31566,#31567);
#27040=AXIS2_PLACEMENT_3D('',#38978,#31569,#31570);
#27041=AXIS2_PLACEMENT_3D('',#38980,#31571,#31572);
#27042=AXIS2_PLACEMENT_3D('',#38982,#31574,#31575);
#27043=AXIS2_PLACEMENT_3D('',#38984,#31576,#31577);
#27044=AXIS2_PLACEMENT_3D('',#38986,#31579,#31580);
#27045=AXIS2_PLACEMENT_3D('',#38990,#31583,#31584);
#27046=AXIS2_PLACEMENT_3D('',#38992,#31585,#31586);
#27047=AXIS2_PLACEMENT_3D('',#38994,#31588,#31589);
#27048=AXIS2_PLACEMENT_3D('',#38998,#31592,#31593);
#27049=AXIS2_PLACEMENT_3D('',#39000,#31594,#31595);
#27050=AXIS2_PLACEMENT_3D('',#39002,#31597,#31598);
#27051=AXIS2_PLACEMENT_3D('',#39004,#31600,#31601);
#27052=AXIS2_PLACEMENT_3D('',#39013,#31606,#31607);
#27053=AXIS2_PLACEMENT_3D('',#39019,#31611,#31612);
#27054=AXIS2_PLACEMENT_3D('',#39025,#31616,#31617);
#27055=AXIS2_PLACEMENT_3D('',#39031,#31621,#31622);
#27056=AXIS2_PLACEMENT_3D('',#39037,#31626,#31627);
#27057=AXIS2_PLACEMENT_3D('',#39046,#31632,#31633);
#27058=AXIS2_PLACEMENT_3D('',#39052,#31637,#31638);
#27059=AXIS2_PLACEMENT_3D('',#39058,#31642,#31643);
#27060=AXIS2_PLACEMENT_3D('',#39061,#31646,#31647);
#27061=AXIS2_PLACEMENT_3D('',#39069,#31652,#31653);
#27062=AXIS2_PLACEMENT_3D('',#39075,#31657,#31658);
#27063=AXIS2_PLACEMENT_3D('',#39081,#31662,#31663);
#27064=AXIS2_PLACEMENT_3D('',#39087,#31667,#31668);
#27065=AXIS2_PLACEMENT_3D('',#39093,#31672,#31673);
#27066=AXIS2_PLACEMENT_3D('',#39099,#31677,#31678);
#27067=AXIS2_PLACEMENT_3D('',#39105,#31682,#31683);
#27068=AXIS2_PLACEMENT_3D('',#39111,#31687,#31688);
#27069=AXIS2_PLACEMENT_3D('',#39117,#31692,#31693);
#27070=AXIS2_PLACEMENT_3D('',#39123,#31697,#31698);
#27071=AXIS2_PLACEMENT_3D('',#39129,#31702,#31703);
#27072=AXIS2_PLACEMENT_3D('',#39135,#31707,#31708);
#27073=AXIS2_PLACEMENT_3D('',#39141,#31712,#31713);
#27074=AXIS2_PLACEMENT_3D('',#39147,#31717,#31718);
#27075=AXIS2_PLACEMENT_3D('',#39152,#31722,#31723);
#27076=AXIS2_PLACEMENT_3D('',#39154,#31724,#31725);
#27077=AXIS2_PLACEMENT_3D('',#39158,#31728,#31729);
#27078=AXIS2_PLACEMENT_3D('',#39164,#31733,#31734);
#27079=AXIS2_PLACEMENT_3D('',#39166,#31735,#31736);
#27080=AXIS2_PLACEMENT_3D('',#39170,#31739,#31740);
#27081=AXIS2_PLACEMENT_3D('',#39172,#31741,#31742);
#27082=AXIS2_PLACEMENT_3D('',#39176,#31745,#31746);
#27083=AXIS2_PLACEMENT_3D('',#39182,#31750,#31751);
#27084=AXIS2_PLACEMENT_3D('',#39184,#31753,#31754);
#27085=AXIS2_PLACEMENT_3D('',#39185,#31755,#31756);
#27086=AXIS2_PLACEMENT_3D('',#39186,#31757,#31758);
#27087=AXIS2_PLACEMENT_3D('',#39190,#31761,#31762);
#27088=AXIS2_PLACEMENT_3D('',#39196,#31766,#31767);
#27089=AXIS2_PLACEMENT_3D('',#39202,#31771,#31772);
#27090=AXIS2_PLACEMENT_3D('',#39207,#31776,#31777);
#27091=AXIS2_PLACEMENT_3D('',#39208,#31778,#31779);
#27092=AXIS2_PLACEMENT_3D('',#39210,#31781,#31782);
#27093=AXIS2_PLACEMENT_3D('',#39216,#31785,#31786);
#27094=AXIS2_PLACEMENT_3D('',#39220,#31788,#31789);
#27095=AXIS2_PLACEMENT_3D('',#39224,#31791,#31792);
#27096=AXIS2_PLACEMENT_3D('',#39226,#31793,#31794);
#27097=AXIS2_PLACEMENT_3D('',#39228,#31795,#31796);
#27098=AXIS2_PLACEMENT_3D('',#39232,#31798,#31799);
#27099=AXIS2_PLACEMENT_3D('',#39236,#31801,#31802);
#27100=AXIS2_PLACEMENT_3D('',#39240,#31804,#31805);
#27101=AXIS2_PLACEMENT_3D('',#39242,#31806,#31807);
#27102=AXIS2_PLACEMENT_3D('',#39244,#31808,#31809);
#27103=AXIS2_PLACEMENT_3D('',#39252,#31813,#31814);
#27104=AXIS2_PLACEMENT_3D('',#39254,#31815,#31816);
#27105=AXIS2_PLACEMENT_3D('',#39256,#31817,#31818);
#27106=AXIS2_PLACEMENT_3D('',#39260,#31820,#31821);
#27107=AXIS2_PLACEMENT_3D('',#39264,#31823,#31824);
#27108=AXIS2_PLACEMENT_3D('',#39268,#31826,#31827);
#27109=AXIS2_PLACEMENT_3D('',#39270,#31828,#31829);
#27110=AXIS2_PLACEMENT_3D('',#39272,#31830,#31831);
#27111=AXIS2_PLACEMENT_3D('',#39276,#31833,#31834);
#27112=AXIS2_PLACEMENT_3D('',#39280,#31836,#31837);
#27113=AXIS2_PLACEMENT_3D('',#39284,#31840,#31841);
#27114=AXIS2_PLACEMENT_3D('',#39310,#31855,#31856);
#27115=AXIS2_PLACEMENT_3D('',#39316,#31860,#31861);
#27116=AXIS2_PLACEMENT_3D('',#39322,#31865,#31866);
#27117=AXIS2_PLACEMENT_3D('',#39326,#31869,#31870);
#27118=AXIS2_PLACEMENT_3D('',#39330,#31873,#31874);
#27119=AXIS2_PLACEMENT_3D('',#39334,#31877,#31878);
#27120=AXIS2_PLACEMENT_3D('',#39338,#31880,#31881);
#27121=AXIS2_PLACEMENT_3D('',#39340,#31883,#31884);
#27122=AXIS2_PLACEMENT_3D('',#39344,#31886,#31887);
#27123=AXIS2_PLACEMENT_3D('',#39346,#31889,#31890);
#27124=AXIS2_PLACEMENT_3D('',#39348,#31892,#31893);
#27125=AXIS2_PLACEMENT_3D('',#39352,#31896,#31897);
#27126=AXIS2_PLACEMENT_3D('',#39354,#31899,#31900);
#27127=AXIS2_PLACEMENT_3D('',#39357,#31901,#31902);
#27128=AXIS2_PLACEMENT_3D('',#39360,#31905,#31906);
#27129=AXIS2_PLACEMENT_3D('',#39363,#31907,#31908);
#27130=AXIS2_PLACEMENT_3D('',#39366,#31911,#31912);
#27131=AXIS2_PLACEMENT_3D('',#39367,#31913,#31914);
#27132=AXIS2_PLACEMENT_3D('',#39368,#31915,#31916);
#27133=AXIS2_PLACEMENT_3D('',#39371,#31917,#31918);
#27134=AXIS2_PLACEMENT_3D('',#39374,#31921,#31922);
#27135=AXIS2_PLACEMENT_3D('',#39377,#31923,#31924);
#27136=AXIS2_PLACEMENT_3D('',#39380,#31927,#31928);
#27137=AXIS2_PLACEMENT_3D('',#39382,#31930,#31931);
#27138=AXIS2_PLACEMENT_3D('',#39384,#31933,#31934);
#27139=AXIS2_PLACEMENT_3D('',#39387,#31935,#31936);
#27140=AXIS2_PLACEMENT_3D('',#39390,#31939,#31940);
#27141=AXIS2_PLACEMENT_3D('',#39393,#31941,#31942);
#27142=AXIS2_PLACEMENT_3D('',#39396,#31945,#31946);
#27143=AXIS2_PLACEMENT_3D('',#39397,#31947,#31948);
#27144=AXIS2_PLACEMENT_3D('',#39398,#31949,#31950);
#27145=AXIS2_PLACEMENT_3D('',#39404,#31954,#31955);
#27146=AXIS2_PLACEMENT_3D('',#39406,#31957,#31958);
#27147=AXIS2_PLACEMENT_3D('',#39409,#31959,#31960);
#27148=AXIS2_PLACEMENT_3D('',#39412,#31963,#31964);
#27149=AXIS2_PLACEMENT_3D('',#39415,#31965,#31966);
#27150=AXIS2_PLACEMENT_3D('',#39418,#31969,#31970);
#27151=AXIS2_PLACEMENT_3D('',#39419,#31971,#31972);
#27152=AXIS2_PLACEMENT_3D('',#39420,#31973,#31974);
#27153=AXIS2_PLACEMENT_3D('',#39423,#31975,#31976);
#27154=AXIS2_PLACEMENT_3D('',#39426,#31979,#31980);
#27155=AXIS2_PLACEMENT_3D('',#39429,#31981,#31982);
#27156=AXIS2_PLACEMENT_3D('',#39432,#31985,#31986);
#27157=AXIS2_PLACEMENT_3D('',#39434,#31988,#31989);
#27158=AXIS2_PLACEMENT_3D('',#39436,#31991,#31992);
#27159=AXIS2_PLACEMENT_3D('',#39438,#31994,#31995);
#27160=AXIS2_PLACEMENT_3D('',#39441,#31996,#31997);
#27161=AXIS2_PLACEMENT_3D('',#39444,#32000,#32001);
#27162=AXIS2_PLACEMENT_3D('',#39447,#32002,#32003);
#27163=AXIS2_PLACEMENT_3D('',#39450,#32006,#32007);
#27164=AXIS2_PLACEMENT_3D('',#39451,#32008,#32009);
#27165=AXIS2_PLACEMENT_3D('',#39452,#32010,#32011);
#27166=AXIS2_PLACEMENT_3D('',#39456,#32013,#32014);
#27167=AXIS2_PLACEMENT_3D('',#39458,#32016,#32017);
#27168=AXIS2_PLACEMENT_3D('',#39462,#32019,#32020);
#27169=AXIS2_PLACEMENT_3D('',#39464,#32022,#32023);
#27170=AXIS2_PLACEMENT_3D('',#39470,#32027,#32028);
#27171=AXIS2_PLACEMENT_3D('',#39474,#32031,#32032);
#27172=AXIS2_PLACEMENT_3D('',#39478,#32035,#32036);
#27173=AXIS2_PLACEMENT_3D('',#39480,#32038,#32039);
#27174=AXIS2_PLACEMENT_3D('',#39484,#32042,#32043);
#27175=AXIS2_PLACEMENT_3D('',#39486,#32045,#32046);
#27176=AXIS2_PLACEMENT_3D('',#39488,#32048,#32049);
#27177=AXIS2_PLACEMENT_3D('',#39490,#32051,#32052);
#27178=AXIS2_PLACEMENT_3D('',#39492,#32054,#32055);
#27179=AXIS2_PLACEMENT_3D('',#39494,#32057,#32058);
#27180=AXIS2_PLACEMENT_3D('',#39496,#32060,#32061);
#27181=AXIS2_PLACEMENT_3D('',#39500,#32064,#32065);
#27182=AXIS2_PLACEMENT_3D('',#39502,#32067,#32068);
#27183=AXIS2_PLACEMENT_3D('',#39503,#32069,#32070);
#27184=AXIS2_PLACEMENT_3D('',#39507,#32073,#32074);
#27185=AXIS2_PLACEMENT_3D('',#39509,#32075,#32076);
#27186=AXIS2_PLACEMENT_3D('',#39511,#32078,#32079);
#27187=AXIS2_PLACEMENT_3D('',#39513,#32081,#32082);
#27188=AXIS2_PLACEMENT_3D('',#39514,#32083,#32084);
#27189=AXIS2_PLACEMENT_3D('',#39515,#32085,#32086);
#27190=AXIS2_PLACEMENT_3D('',#39516,#32087,#32088);
#27191=AXIS2_PLACEMENT_3D('',#39517,#32089,#32090);
#27192=AXIS2_PLACEMENT_3D('',#39518,#32091,#32092);
#27193=AXIS2_PLACEMENT_3D('',#39519,#32093,#32094);
#27194=AXIS2_PLACEMENT_3D('',#39521,#32095,#32096);
#27195=AXIS2_PLACEMENT_3D('',#39523,#32097,#32098);
#27196=AXIS2_PLACEMENT_3D('',#39524,#32099,#32100);
#27197=AXIS2_PLACEMENT_3D('',#39553,#32101,#32102);
#27198=AXIS2_PLACEMENT_3D('',#39554,#32103,#32104);
#27199=AXIS2_PLACEMENT_3D('',#39555,#32105,#32106);
#27200=AXIS2_PLACEMENT_3D('',#39558,#32108,#32109);
#27201=AXIS2_PLACEMENT_3D('',#39559,#32110,#32111);
#27202=AXIS2_PLACEMENT_3D('',#39561,#32112,#32113);
#27203=AXIS2_PLACEMENT_3D('',#39562,#32114,#32115);
#27204=AXIS2_PLACEMENT_3D('',#39565,#32116,#32117);
#27205=AXIS2_PLACEMENT_3D('',#39573,#32118,#32119);
#27206=AXIS2_PLACEMENT_3D('',#39576,#32120,#32121);
#27207=AXIS2_PLACEMENT_3D('',#39584,#32122,#32123);
#27208=AXIS2_PLACEMENT_3D('',#39587,#32124,#32125);
#27209=AXIS2_PLACEMENT_3D('',#39601,#32127,#32128);
#27210=AXIS2_PLACEMENT_3D('',#39612,#32129,#32130);
#27211=AXIS2_PLACEMENT_3D('',#39614,#32131,#32132);
#27212=AXIS2_PLACEMENT_3D('',#39616,#32133,#32134);
#27213=AXIS2_PLACEMENT_3D('',#39617,#32135,#32136);
#27214=AXIS2_PLACEMENT_3D('',#39621,#32138,#32139);
#27215=AXIS2_PLACEMENT_3D('',#39623,#32140,#32141);
#27216=AXIS2_PLACEMENT_3D('',#39625,#32142,#32143);
#27217=AXIS2_PLACEMENT_3D('',#39627,#32144,#32145);
#27218=AXIS2_PLACEMENT_3D('',#39629,#32146,#32147);
#27219=AXIS2_PLACEMENT_3D('',#39630,#32148,#32149);
#27220=AXIS2_PLACEMENT_3D('',#39631,#32150,#32151);
#27221=AXIS2_PLACEMENT_3D('',#39633,#32152,#32153);
#27222=AXIS2_PLACEMENT_3D('',#39634,#32154,#32155);
#27223=AXIS2_PLACEMENT_3D('',#39636,#32156,#32157);
#27224=AXIS2_PLACEMENT_3D('',#39638,#32158,#32159);
#27225=AXIS2_PLACEMENT_3D('',#39640,#32160,#32161);
#27226=AXIS2_PLACEMENT_3D('',#39642,#32162,#32163);
#27227=AXIS2_PLACEMENT_3D('',#39643,#32164,#32165);
#27228=AXIS2_PLACEMENT_3D('',#39644,#32166,#32167);
#27229=AXIS2_PLACEMENT_3D('',#39646,#32168,#32169);
#27230=AXIS2_PLACEMENT_3D('',#39648,#32170,#32171);
#27231=AXIS2_PLACEMENT_3D('',#39650,#32172,#32173);
#27232=AXIS2_PLACEMENT_3D('',#39652,#32174,#32175);
#27233=AXIS2_PLACEMENT_3D('',#39653,#32176,#32177);
#27234=AXIS2_PLACEMENT_3D('',#39654,#32178,#32179);
#27235=AXIS2_PLACEMENT_3D('',#39658,#32182,#32183);
#27236=AXIS2_PLACEMENT_3D('',#39662,#32186,#32187);
#27237=AXIS2_PLACEMENT_3D('',#39666,#32190,#32191);
#27238=AXIS2_PLACEMENT_3D('',#39670,#32194,#32195);
#27239=AXIS2_PLACEMENT_3D('',#39674,#32198,#32199);
#27240=AXIS2_PLACEMENT_3D('',#39678,#32202,#32203);
#27241=AXIS2_PLACEMENT_3D('',#39684,#32207,#32208);
#27242=AXIS2_PLACEMENT_3D('',#39688,#32211,#32212);
#27243=AXIS2_PLACEMENT_3D('',#39692,#32215,#32216);
#27244=AXIS2_PLACEMENT_3D('',#39696,#32219,#32220);
#27245=AXIS2_PLACEMENT_3D('',#39700,#32223,#32224);
#27246=AXIS2_PLACEMENT_3D('',#39702,#32226,#32227);
#27247=AXIS2_PLACEMENT_3D('',#39703,#32228,#32229);
#27248=AXIS2_PLACEMENT_3D('',#39711,#32230,#32231);
#27249=AXIS2_PLACEMENT_3D('',#39719,#32232,#32233);
#27250=AXIS2_PLACEMENT_3D('',#39727,#32234,#32235);
#27251=AXIS2_PLACEMENT_3D('',#39735,#32236,#32237);
#27252=AXIS2_PLACEMENT_3D('',#39743,#32238,#32239);
#27253=AXIS2_PLACEMENT_3D('',#39751,#32240,#32241);
#27254=AXIS2_PLACEMENT_3D('',#39759,#32242,#32243);
#27255=AXIS2_PLACEMENT_3D('',#39767,#32244,#32245);
#27256=AXIS2_PLACEMENT_3D('',#39775,#32246,#32247);
#27257=AXIS2_PLACEMENT_3D('',#39783,#32248,#32249);
#27258=AXIS2_PLACEMENT_3D('',#39786,#32252,#32253);
#27259=AXIS2_PLACEMENT_3D('',#39788,#32255,#32256);
#27260=AXIS2_PLACEMENT_3D('',#39790,#32258,#32259);
#27261=AXIS2_PLACEMENT_3D('',#39792,#32261,#32262);
#27262=AXIS2_PLACEMENT_3D('',#39794,#32264,#32265);
#27263=AXIS2_PLACEMENT_3D('',#39795,#32266,#32267);
#27264=AXIS2_PLACEMENT_3D('',#39796,#32268,#32269);
#27265=AXIS2_PLACEMENT_3D('',#39797,#32270,#32271);
#27266=AXIS2_PLACEMENT_3D('',#39798,#32272,#32273);
#27267=AXIS2_PLACEMENT_3D('',#39799,#32274,#32275);
#27268=AXIS2_PLACEMENT_3D('',#39800,#32276,#32277);
#27269=AXIS2_PLACEMENT_3D('',#39801,#32278,#32279);
#27270=AXIS2_PLACEMENT_3D('',#39802,#32280,#32281);
#27271=AXIS2_PLACEMENT_3D('',#39803,#32282,#32283);
#27272=AXIS2_PLACEMENT_3D('',#39804,#32284,#32285);
#27273=AXIS2_PLACEMENT_3D('',#39805,#32286,#32287);
#27274=AXIS2_PLACEMENT_3D('',#39806,#32288,#32289);
#27275=AXIS2_PLACEMENT_3D('',#39807,#32290,#32291);
#27276=AXIS2_PLACEMENT_3D('',#39808,#32292,#32293);
#27277=AXIS2_PLACEMENT_3D('',#39810,#32294,#32295);
#27278=AXIS2_PLACEMENT_3D('',#39814,#32297,#32298);
#27279=AXIS2_PLACEMENT_3D('',#39838,#32301,#32302);
#27280=AXIS2_PLACEMENT_3D('',#39839,#32303,#32304);
#27281=AXIS2_PLACEMENT_3D('',#39841,#32305,#32306);
#27282=AXIS2_PLACEMENT_3D('',#39842,#32307,#32308);
#27283=AXIS2_PLACEMENT_3D('',#39843,#32309,#32310);
#27284=AXIS2_PLACEMENT_3D('',#39845,#32311,#32312);
#27285=AXIS2_PLACEMENT_3D('',#39848,#32314,#32315);
#27286=AXIS2_PLACEMENT_3D('',#39849,#32316,#32317);
#27287=AXIS2_PLACEMENT_3D('',#39851,#32318,#32319);
#27288=AXIS2_PLACEMENT_3D('',#39853,#32321,#32322);
#27289=AXIS2_PLACEMENT_3D('',#39855,#32323,#32324);
#27290=AXIS2_PLACEMENT_3D('',#39856,#32325,#32326);
#27291=AXIS2_PLACEMENT_3D('',#39857,#32327,#32328);
#27292=AXIS2_PLACEMENT_3D('',#39859,#32329,#32330);
#27293=AXIS2_PLACEMENT_3D('',#39862,#32332,#32333);
#27294=AXIS2_PLACEMENT_3D('',#39863,#32334,#32335);
#27295=AXIS2_PLACEMENT_3D('',#39866,#32336,#32337);
#27296=AXIS2_PLACEMENT_3D('',#39867,#32338,#32339);
#27297=AXIS2_PLACEMENT_3D('',#39869,#32341,#32342);
#27298=AXIS2_PLACEMENT_3D('',#39872,#32344,#32345);
#27299=AXIS2_PLACEMENT_3D('',#39873,#32346,#32347);
#27300=AXIS2_PLACEMENT_3D('',#39875,#32348,#32349);
#27301=AXIS2_PLACEMENT_3D('',#39877,#32350,#32351);
#27302=AXIS2_PLACEMENT_3D('',#39878,#32352,#32353);
#27303=AXIS2_PLACEMENT_3D('',#39879,#32354,#32355);
#27304=AXIS2_PLACEMENT_3D('',#39881,#32356,#32357);
#27305=AXIS2_PLACEMENT_3D('',#39883,#32359,#32360);
#27306=AXIS2_PLACEMENT_3D('',#39885,#32361,#32362);
#27307=AXIS2_PLACEMENT_3D('',#39888,#32364,#32365);
#27308=AXIS2_PLACEMENT_3D('',#39889,#32366,#32367);
#27309=AXIS2_PLACEMENT_3D('',#39892,#32368,#32369);
#27310=AXIS2_PLACEMENT_3D('',#39893,#32370,#32371);
#27311=AXIS2_PLACEMENT_3D('',#39896,#32373,#32374);
#27312=AXIS2_PLACEMENT_3D('',#39897,#32375,#32376);
#27313=AXIS2_PLACEMENT_3D('',#39900,#32378,#32379);
#27314=AXIS2_PLACEMENT_3D('',#39901,#32380,#32381);
#27315=AXIS2_PLACEMENT_3D('',#39902,#32382,#32383);
#27316=AXIS2_PLACEMENT_3D('',#39903,#32384,#32385);
#27317=AXIS2_PLACEMENT_3D('',#39904,#32386,#32387);
#27318=AXIS2_PLACEMENT_3D('',#39905,#32388,#32389);
#27319=AXIS2_PLACEMENT_3D('',#39906,#32390,#32391);
#27320=AXIS2_PLACEMENT_3D('',#39912,#32392,#32393);
#27321=AXIS2_PLACEMENT_3D('',#39916,#32394,#32395);
#27322=AXIS2_PLACEMENT_3D('',#39922,#32399,#32400);
#27323=AXIS2_PLACEMENT_3D('',#39923,#32401,#32402);
#27324=AXIS2_PLACEMENT_3D('',#39927,#32405,#32406);
#27325=AXIS2_PLACEMENT_3D('',#39931,#32409,#32410);
#27326=AXIS2_PLACEMENT_3D('',#39932,#32411,#32412);
#27327=AXIS2_PLACEMENT_3D('',#39933,#32413,#32414);
#27328=AXIS2_PLACEMENT_3D('',#39934,#32415,#32416);
#27329=AXIS2_PLACEMENT_3D('',#39935,#32417,#32418);
#27330=AXIS2_PLACEMENT_3D('',#40007,#32420,#32421);
#27331=AXIS2_PLACEMENT_3D('',#40009,#32422,#32423);
#27332=AXIS2_PLACEMENT_3D('',#40012,#32425,#32426);
#27333=AXIS2_PLACEMENT_3D('',#40013,#32427,#32428);
#27334=AXIS2_PLACEMENT_3D('',#40015,#32429,#32430);
#27335=AXIS2_PLACEMENT_3D('',#40018,#32432,#32433);
#27336=AXIS2_PLACEMENT_3D('',#40019,#32434,#32435);
#27337=AXIS2_PLACEMENT_3D('',#40021,#32436,#32437);
#27338=AXIS2_PLACEMENT_3D('',#40024,#32439,#32440);
#27339=AXIS2_PLACEMENT_3D('',#40025,#32441,#32442);
#27340=AXIS2_PLACEMENT_3D('',#40027,#32443,#32444);
#27341=AXIS2_PLACEMENT_3D('',#40030,#32446,#32447);
#27342=AXIS2_PLACEMENT_3D('',#40031,#32448,#32449);
#27343=AXIS2_PLACEMENT_3D('',#40033,#32450,#32451);
#27344=AXIS2_PLACEMENT_3D('',#40036,#32453,#32454);
#27345=AXIS2_PLACEMENT_3D('',#40037,#32455,#32456);
#27346=AXIS2_PLACEMENT_3D('',#40039,#32457,#32458);
#27347=AXIS2_PLACEMENT_3D('',#40042,#32460,#32461);
#27348=AXIS2_PLACEMENT_3D('',#40043,#32462,#32463);
#27349=AXIS2_PLACEMENT_3D('',#40045,#32464,#32465);
#27350=AXIS2_PLACEMENT_3D('',#40048,#32467,#32468);
#27351=AXIS2_PLACEMENT_3D('',#40049,#32469,#32470);
#27352=AXIS2_PLACEMENT_3D('',#40051,#32471,#32472);
#27353=AXIS2_PLACEMENT_3D('',#40054,#32474,#32475);
#27354=AXIS2_PLACEMENT_3D('',#40055,#32476,#32477);
#27355=AXIS2_PLACEMENT_3D('',#40057,#32478,#32479);
#27356=AXIS2_PLACEMENT_3D('',#40060,#32481,#32482);
#27357=AXIS2_PLACEMENT_3D('',#40061,#32483,#32484);
#27358=AXIS2_PLACEMENT_3D('',#40063,#32485,#32486);
#27359=AXIS2_PLACEMENT_3D('',#40066,#32488,#32489);
#27360=AXIS2_PLACEMENT_3D('',#40067,#32490,#32491);
#27361=AXIS2_PLACEMENT_3D('',#40069,#32492,#32493);
#27362=AXIS2_PLACEMENT_3D('',#40072,#32495,#32496);
#27363=AXIS2_PLACEMENT_3D('',#40073,#32497,#32498);
#27364=AXIS2_PLACEMENT_3D('',#40075,#32499,#32500);
#27365=AXIS2_PLACEMENT_3D('',#40078,#32502,#32503);
#27366=AXIS2_PLACEMENT_3D('',#40079,#32504,#32505);
#27367=AXIS2_PLACEMENT_3D('',#40081,#32506,#32507);
#27368=AXIS2_PLACEMENT_3D('',#40082,#32508,#32509);
#27369=AXIS2_PLACEMENT_3D('',#40083,#32510,#32511);
#27370=AXIS2_PLACEMENT_3D('',#40088,#32513,#32514);
#27371=AXIS2_PLACEMENT_3D('',#40091,#32516,#32517);
#27372=AXIS2_PLACEMENT_3D('',#40092,#32518,#32519);
#27373=AXIS2_PLACEMENT_3D('',#40105,#32520,#32521);
#27374=AXIS2_PLACEMENT_3D('',#40116,#32522,#32523);
#27375=AXIS2_PLACEMENT_3D('',#40139,#32524,#32525);
#27376=AXIS2_PLACEMENT_3D('',#40140,#32526,#32527);
#27377=AXIS2_PLACEMENT_3D('',#40144,#32529,#32530);
#27378=AXIS2_PLACEMENT_3D('',#40146,#32532,#32533);
#27379=AXIS2_PLACEMENT_3D('',#40151,#32536,#32537);
#27380=AXIS2_PLACEMENT_3D('',#40152,#32538,#32539);
#27381=AXIS2_PLACEMENT_3D('',#40165,#32540,#32541);
#27382=AXIS2_PLACEMENT_3D('',#40176,#32542,#32543);
#27383=AXIS2_PLACEMENT_3D('',#40199,#32544,#32545);
#27384=AXIS2_PLACEMENT_3D('',#40200,#32546,#32547);
#27385=AXIS2_PLACEMENT_3D('',#40203,#32550,#32551);
#27386=AXIS2_PLACEMENT_3D('',#40204,#32552,#32553);
#27387=AXIS2_PLACEMENT_3D('',#40205,#32554,#32555);
#27388=AXIS2_PLACEMENT_3D('',#40206,#32556,#32557);
#27389=AXIS2_PLACEMENT_3D('',#40207,#32558,#32559);
#27390=AXIS2_PLACEMENT_3D('',#40208,#32560,#32561);
#27391=AXIS2_PLACEMENT_3D('',#40209,#32562,#32563);
#27392=AXIS2_PLACEMENT_3D('',#40210,#32564,#32565);
#27393=AXIS2_PLACEMENT_3D('',#40211,#32566,#32567);
#27394=AXIS2_PLACEMENT_3D('',#40212,#32568,#32569);
#27395=AXIS2_PLACEMENT_3D('',#40213,#32570,#32571);
#27396=AXIS2_PLACEMENT_3D('',#40214,#32572,#32573);
#27397=AXIS2_PLACEMENT_3D('',#40216,#32574,#32575);
#27398=AXIS2_PLACEMENT_3D('',#40219,#32577,#32578);
#27399=AXIS2_PLACEMENT_3D('',#40220,#32579,#32580);
#27400=AXIS2_PLACEMENT_3D('',#40222,#32581,#32582);
#27401=AXIS2_PLACEMENT_3D('',#40225,#32584,#32585);
#27402=AXIS2_PLACEMENT_3D('',#40226,#32586,#32587);
#27403=AXIS2_PLACEMENT_3D('',#40228,#32588,#32589);
#27404=AXIS2_PLACEMENT_3D('',#40231,#32591,#32592);
#27405=AXIS2_PLACEMENT_3D('',#40232,#32593,#32594);
#27406=AXIS2_PLACEMENT_3D('',#40234,#32595,#32596);
#27407=AXIS2_PLACEMENT_3D('',#40237,#32598,#32599);
#27408=AXIS2_PLACEMENT_3D('',#40238,#32600,#32601);
#27409=AXIS2_PLACEMENT_3D('',#40240,#32602,#32603);
#27410=AXIS2_PLACEMENT_3D('',#40243,#32605,#32606);
#27411=AXIS2_PLACEMENT_3D('',#40244,#32607,#32608);
#27412=AXIS2_PLACEMENT_3D('',#40246,#32609,#32610);
#27413=AXIS2_PLACEMENT_3D('',#40249,#32612,#32613);
#27414=AXIS2_PLACEMENT_3D('',#40250,#32614,#32615);
#27415=AXIS2_PLACEMENT_3D('',#40252,#32616,#32617);
#27416=AXIS2_PLACEMENT_3D('',#40255,#32619,#32620);
#27417=AXIS2_PLACEMENT_3D('',#40256,#32621,#32622);
#27418=AXIS2_PLACEMENT_3D('',#40265,#32627,#32628);
#27419=AXIS2_PLACEMENT_3D('',#40271,#32632,#32633);
#27420=AXIS2_PLACEMENT_3D('',#40277,#32637,#32638);
#27421=AXIS2_PLACEMENT_3D('',#40283,#32642,#32643);
#27422=AXIS2_PLACEMENT_3D('',#40289,#32647,#32648);
#27423=AXIS2_PLACEMENT_3D('',#40295,#32652,#32653);
#27424=AXIS2_PLACEMENT_3D('',#40301,#32657,#32658);
#27425=AXIS2_PLACEMENT_3D('',#40307,#32662,#32663);
#27426=AXIS2_PLACEMENT_3D('',#40313,#32667,#32668);
#27427=AXIS2_PLACEMENT_3D('',#40319,#32672,#32673);
#27428=AXIS2_PLACEMENT_3D('',#40325,#32677,#32678);
#27429=AXIS2_PLACEMENT_3D('',#40328,#32681,#32682);
#27430=AXIS2_PLACEMENT_3D('',#40329,#32683,#32684);
#27431=AXIS2_PLACEMENT_3D('',#40330,#32685,#32686);
#27432=AXIS2_PLACEMENT_3D('',#40331,#32687,#32688);
#27433=AXIS2_PLACEMENT_3D('',#40332,#32689,#32690);
#27434=AXIS2_PLACEMENT_3D('',#40333,#32691,#32692);
#27435=AXIS2_PLACEMENT_3D('',#40334,#32693,#32694);
#27436=AXIS2_PLACEMENT_3D('',#40335,#32695,#32696);
#27437=AXIS2_PLACEMENT_3D('',#40337,#32697,#32698);
#27438=AXIS2_PLACEMENT_3D('',#40340,#32700,#32701);
#27439=AXIS2_PLACEMENT_3D('',#40341,#32702,#32703);
#27440=AXIS2_PLACEMENT_3D('',#40343,#32704,#32705);
#27441=AXIS2_PLACEMENT_3D('',#40346,#32707,#32708);
#27442=AXIS2_PLACEMENT_3D('',#40347,#32709,#32710);
#27443=AXIS2_PLACEMENT_3D('',#40350,#32711,#32712);
#27444=AXIS2_PLACEMENT_3D('',#40354,#32714,#32715);
#27445=AXIS2_PLACEMENT_3D('',#40356,#32717,#32718);
#27446=AXIS2_PLACEMENT_3D('',#40359,#32719,#32720);
#27447=AXIS2_PLACEMENT_3D('',#40363,#32722,#32723);
#27448=AXIS2_PLACEMENT_3D('',#40365,#32725,#32726);
#27449=AXIS2_PLACEMENT_3D('',#40370,#32728,#32729);
#27450=AXIS2_PLACEMENT_3D('',#40373,#32731,#32732);
#27451=AXIS2_PLACEMENT_3D('',#40375,#32733,#32734);
#27452=AXIS2_PLACEMENT_3D('',#40379,#32736,#32737);
#27453=AXIS2_PLACEMENT_3D('',#40384,#32741,#32742);
#27454=AXIS2_PLACEMENT_3D('',#40394,#32747,#32748);
#27455=AXIS2_PLACEMENT_3D('',#40397,#32750,#32751);
#27456=AXIS2_PLACEMENT_3D('',#40399,#32752,#32753);
#27457=AXIS2_PLACEMENT_3D('',#40402,#32755,#32756);
#27458=AXIS2_PLACEMENT_3D('',#40403,#32757,#32758);
#27459=AXIS2_PLACEMENT_3D('',#40406,#32761,#32762);
#27460=AXIS2_PLACEMENT_3D('',#40408,#32764,#32765);
#27461=AXIS2_PLACEMENT_3D('',#40410,#32767,#32768);
#27462=AXIS2_PLACEMENT_3D('',#40411,#32769,#32770);
#27463=AXIS2_PLACEMENT_3D('',#40413,#32772,#32773);
#27464=AXIS2_PLACEMENT_3D('',#40415,#32775,#32776);
#27465=AXIS2_PLACEMENT_3D('',#40417,#32778,#32779);
#27466=AXIS2_PLACEMENT_3D('',#40419,#32781,#32782);
#27467=AXIS2_PLACEMENT_3D('',#40420,#32783,#32784);
#27468=AXIS2_PLACEMENT_3D('',#40421,#32785,#32786);
#27469=AXIS2_PLACEMENT_3D('',#40422,#32787,#32788);
#27470=AXIS2_PLACEMENT_3D('',#40423,#32789,#32790);
#27471=AXIS2_PLACEMENT_3D('',#40424,#32791,#32792);
#27472=AXIS2_PLACEMENT_3D('',#40425,#32793,#32794);
#27473=AXIS2_PLACEMENT_3D('',#40427,#32795,#32796);
#27474=AXIS2_PLACEMENT_3D('',#40430,#32798,#32799);
#27475=AXIS2_PLACEMENT_3D('',#40431,#32800,#32801);
#27476=AXIS2_PLACEMENT_3D('',#40433,#32802,#32803);
#27477=AXIS2_PLACEMENT_3D('',#40436,#32805,#32806);
#27478=AXIS2_PLACEMENT_3D('',#40437,#32807,#32808);
#27479=AXIS2_PLACEMENT_3D('',#40439,#32809,#32810);
#27480=AXIS2_PLACEMENT_3D('',#40442,#32812,#32813);
#27481=AXIS2_PLACEMENT_3D('',#40443,#32814,#32815);
#27482=AXIS2_PLACEMENT_3D('',#40445,#32816,#32817);
#27483=AXIS2_PLACEMENT_3D('',#40448,#32819,#32820);
#27484=AXIS2_PLACEMENT_3D('',#40449,#32821,#32822);
#27485=AXIS2_PLACEMENT_3D('',#40451,#32823,#32824);
#27486=AXIS2_PLACEMENT_3D('',#40454,#32826,#32827);
#27487=AXIS2_PLACEMENT_3D('',#40455,#32828,#32829);
#27488=AXIS2_PLACEMENT_3D('',#40457,#32830,#32831);
#27489=AXIS2_PLACEMENT_3D('',#40460,#32833,#32834);
#27490=AXIS2_PLACEMENT_3D('',#40461,#32835,#32836);
#27491=AXIS2_PLACEMENT_3D('',#40463,#32837,#32838);
#27492=AXIS2_PLACEMENT_3D('',#40466,#32840,#32841);
#27493=AXIS2_PLACEMENT_3D('',#40467,#32842,#32843);
#27494=AXIS2_PLACEMENT_3D('',#40469,#32844,#32845);
#27495=AXIS2_PLACEMENT_3D('',#40472,#32847,#32848);
#27496=AXIS2_PLACEMENT_3D('',#40473,#32849,#32850);
#27497=AXIS2_PLACEMENT_3D('',#40475,#32851,#32852);
#27498=AXIS2_PLACEMENT_3D('',#40478,#32854,#32855);
#27499=AXIS2_PLACEMENT_3D('',#40479,#32856,#32857);
#27500=AXIS2_PLACEMENT_3D('',#40481,#32858,#32859);
#27501=AXIS2_PLACEMENT_3D('',#40484,#32861,#32862);
#27502=AXIS2_PLACEMENT_3D('',#40485,#32863,#32864);
#27503=AXIS2_PLACEMENT_3D('',#40487,#32865,#32866);
#27504=AXIS2_PLACEMENT_3D('',#40490,#32868,#32869);
#27505=AXIS2_PLACEMENT_3D('',#40491,#32870,#32871);
#27506=AXIS2_PLACEMENT_3D('',#40493,#32872,#32873);
#27507=AXIS2_PLACEMENT_3D('',#40496,#32875,#32876);
#27508=AXIS2_PLACEMENT_3D('',#40497,#32877,#32878);
#27509=AXIS2_PLACEMENT_3D('',#40499,#32879,#32880);
#27510=AXIS2_PLACEMENT_3D('',#40502,#32882,#32883);
#27511=AXIS2_PLACEMENT_3D('',#40503,#32884,#32885);
#27512=AXIS2_PLACEMENT_3D('',#40505,#32886,#32887);
#27513=AXIS2_PLACEMENT_3D('',#40508,#32889,#32890);
#27514=AXIS2_PLACEMENT_3D('',#40509,#32891,#32892);
#27515=AXIS2_PLACEMENT_3D('',#40511,#32893,#32894);
#27516=AXIS2_PLACEMENT_3D('',#40514,#32896,#32897);
#27517=AXIS2_PLACEMENT_3D('',#40515,#32898,#32899);
#27518=AXIS2_PLACEMENT_3D('',#40517,#32900,#32901);
#27519=AXIS2_PLACEMENT_3D('',#40520,#32903,#32904);
#27520=AXIS2_PLACEMENT_3D('',#40521,#32905,#32906);
#27521=AXIS2_PLACEMENT_3D('',#40523,#32907,#32908);
#27522=AXIS2_PLACEMENT_3D('',#40526,#32910,#32911);
#27523=AXIS2_PLACEMENT_3D('',#40527,#32912,#32913);
#27524=AXIS2_PLACEMENT_3D('',#40529,#32914,#32915);
#27525=AXIS2_PLACEMENT_3D('',#40532,#32917,#32918);
#27526=AXIS2_PLACEMENT_3D('',#40533,#32919,#32920);
#27527=AXIS2_PLACEMENT_3D('',#40535,#32921,#32922);
#27528=AXIS2_PLACEMENT_3D('',#40538,#32924,#32925);
#27529=AXIS2_PLACEMENT_3D('',#40539,#32926,#32927);
#27530=AXIS2_PLACEMENT_3D('',#40541,#32928,#32929);
#27531=AXIS2_PLACEMENT_3D('',#40544,#32931,#32932);
#27532=AXIS2_PLACEMENT_3D('',#40545,#32933,#32934);
#27533=AXIS2_PLACEMENT_3D('',#40547,#32935,#32936);
#27534=AXIS2_PLACEMENT_3D('',#40550,#32938,#32939);
#27535=AXIS2_PLACEMENT_3D('',#40551,#32940,#32941);
#27536=AXIS2_PLACEMENT_3D('',#40552,#32942,#32943);
#27537=AXIS2_PLACEMENT_3D('',#40553,#32944,#32945);
#27538=AXIS2_PLACEMENT_3D('',#40554,#32946,#32947);
#27539=AXIS2_PLACEMENT_3D('',#40555,#32948,#32949);
#27540=AXIS2_PLACEMENT_3D('',#40596,#32970,#32971);
#27541=AXIS2_PLACEMENT_3D('',#40602,#32975,#32976);
#27542=AXIS2_PLACEMENT_3D('',#40606,#32979,#32980);
#27543=AXIS2_PLACEMENT_3D('',#40610,#32983,#32984);
#27544=AXIS2_PLACEMENT_3D('',#40614,#32987,#32988);
#27545=AXIS2_PLACEMENT_3D('',#40618,#32991,#32992);
#27546=AXIS2_PLACEMENT_3D('',#40622,#32995,#32996);
#27547=AXIS2_PLACEMENT_3D('',#40626,#32999,#33000);
#27548=AXIS2_PLACEMENT_3D('',#40630,#33003,#33004);
#27549=AXIS2_PLACEMENT_3D('',#40634,#33007,#33008);
#27550=AXIS2_PLACEMENT_3D('',#40638,#33011,#33012);
#27551=AXIS2_PLACEMENT_3D('',#40642,#33015,#33016);
#27552=AXIS2_PLACEMENT_3D('',#40644,#33018,#33019);
#27553=AXIS2_PLACEMENT_3D('',#40645,#33020,#33021);
#27554=AXIS2_PLACEMENT_3D('',#40646,#33022,#33023);
#27555=AXIS2_PLACEMENT_3D('',#40647,#33024,#33025);
#27556=AXIS2_PLACEMENT_3D('',#40648,#33026,#33027);
#27557=AXIS2_PLACEMENT_3D('',#40649,#33028,#33029);
#27558=AXIS2_PLACEMENT_3D('',#40666,#33038,#33039);
#27559=AXIS2_PLACEMENT_3D('',#40669,#33042,#33043);
#27560=AXIS2_PLACEMENT_3D('',#40671,#33045,#33046);
#27561=AXIS2_PLACEMENT_3D('',#40673,#33048,#33049);
#27562=AXIS2_PLACEMENT_3D('',#40675,#33051,#33052);
#27563=AXIS2_PLACEMENT_3D('',#40677,#33054,#33055);
#27564=AXIS2_PLACEMENT_3D('',#40679,#33057,#33058);
#27565=AXIS2_PLACEMENT_3D('',#40681,#33060,#33061);
#27566=AXIS2_PLACEMENT_3D('',#40682,#33062,#33063);
#27567=AXIS2_PLACEMENT_3D('',#40695,#33070,#33071);
#27568=AXIS2_PLACEMENT_3D('',#40708,#33078,#33079);
#27569=AXIS2_PLACEMENT_3D('',#40721,#33086,#33087);
#27570=AXIS2_PLACEMENT_3D('',#40734,#33094,#33095);
#27571=AXIS2_PLACEMENT_3D('',#40740,#33099,#33100);
#27572=AXIS2_PLACEMENT_3D('',#40744,#33103,#33104);
#27573=AXIS2_PLACEMENT_3D('',#40748,#33107,#33108);
#27574=AXIS2_PLACEMENT_3D('',#40752,#33111,#33112);
#27575=AXIS2_PLACEMENT_3D('',#40756,#33115,#33116);
#27576=AXIS2_PLACEMENT_3D('',#40758,#33118,#33119);
#27577=AXIS2_PLACEMENT_3D('',#40759,#33120,#33121);
#27578=AXIS2_PLACEMENT_3D('',#40765,#33125,#33126);
#27579=AXIS2_PLACEMENT_3D('',#40769,#33129,#33130);
#27580=AXIS2_PLACEMENT_3D('',#40773,#33133,#33134);
#27581=AXIS2_PLACEMENT_3D('',#40777,#33137,#33138);
#27582=AXIS2_PLACEMENT_3D('',#40781,#33141,#33142);
#27583=AXIS2_PLACEMENT_3D('',#40783,#33144,#33145);
#27584=AXIS2_PLACEMENT_3D('',#40784,#33146,#33147);
#27585=AXIS2_PLACEMENT_3D('',#40790,#33151,#33152);
#27586=AXIS2_PLACEMENT_3D('',#40794,#33155,#33156);
#27587=AXIS2_PLACEMENT_3D('',#40798,#33159,#33160);
#27588=AXIS2_PLACEMENT_3D('',#40802,#33163,#33164);
#27589=AXIS2_PLACEMENT_3D('',#40806,#33167,#33168);
#27590=AXIS2_PLACEMENT_3D('',#40808,#33170,#33171);
#27591=AXIS2_PLACEMENT_3D('',#40809,#33172,#33173);
#27592=AXIS2_PLACEMENT_3D('',#40815,#33177,#33178);
#27593=AXIS2_PLACEMENT_3D('',#40819,#33181,#33182);
#27594=AXIS2_PLACEMENT_3D('',#40823,#33185,#33186);
#27595=AXIS2_PLACEMENT_3D('',#40827,#33189,#33190);
#27596=AXIS2_PLACEMENT_3D('',#40831,#33193,#33194);
#27597=AXIS2_PLACEMENT_3D('',#40833,#33196,#33197);
#27598=AXIS2_PLACEMENT_3D('',#40834,#33198,#33199);
#27599=AXIS2_PLACEMENT_3D('',#40835,#33200,#33201);
#27600=AXIS2_PLACEMENT_3D('',#40836,#33202,#33203);
#27601=AXIS2_PLACEMENT_3D('',#40837,#33204,#33205);
#27602=AXIS2_PLACEMENT_3D('',#40838,#33206,#33207);
#27603=AXIS2_PLACEMENT_3D('',#40839,#33208,#33209);
#27604=AXIS2_PLACEMENT_3D('',#40844,#33211,#33212);
#27605=AXIS2_PLACEMENT_3D('',#40846,#33213,#33214);
#27606=AXIS2_PLACEMENT_3D('',#40848,#33215,#33216);
#27607=AXIS2_PLACEMENT_3D('',#40850,#33217,#33218);
#27608=AXIS2_PLACEMENT_3D('',#40852,#33219,#33220);
#27609=AXIS2_PLACEMENT_3D('',#40853,#33221,#33222);
#27610=AXIS2_PLACEMENT_3D('',#40854,#33223,#33224);
#27611=AXIS2_PLACEMENT_3D('',#40877,#33226,#33227);
#27612=AXIS2_PLACEMENT_3D('',#40897,#33228,#33229);
#27613=AXIS2_PLACEMENT_3D('',#40938,#33231,#33232);
#27614=AXIS2_PLACEMENT_3D('',#40941,#33233,#33234);
#27615=AXIS2_PLACEMENT_3D('',#40944,#33236,#33237);
#27616=AXIS2_PLACEMENT_3D('',#40945,#33238,#33239);
#27617=AXIS2_PLACEMENT_3D('',#40946,#33240,#33241);
#27618=AXIS2_PLACEMENT_3D('',#40987,#33243,#33244);
#27619=AXIS2_PLACEMENT_3D('',#40990,#33245,#33246);
#27620=AXIS2_PLACEMENT_3D('',#40993,#33248,#33249);
#27621=AXIS2_PLACEMENT_3D('',#40994,#33250,#33251);
#27622=AXIS2_PLACEMENT_3D('',#40995,#33252,#33253);
#27623=AXIS2_PLACEMENT_3D('',#40997,#33254,#33255);
#27624=AXIS2_PLACEMENT_3D('',#41000,#33257,#33258);
#27625=AXIS2_PLACEMENT_3D('',#41001,#33259,#33260);
#27626=AXIS2_PLACEMENT_3D('',#41004,#33261,#33262);
#27627=AXIS2_PLACEMENT_3D('',#41008,#33264,#33265);
#27628=AXIS2_PLACEMENT_3D('',#41010,#33267,#33268);
#27629=AXIS2_PLACEMENT_3D('',#41012,#33269,#33270);
#27630=AXIS2_PLACEMENT_3D('',#41015,#33272,#33273);
#27631=AXIS2_PLACEMENT_3D('',#41016,#33274,#33275);
#27632=AXIS2_PLACEMENT_3D('',#41018,#33277,#33278);
#27633=AXIS2_PLACEMENT_3D('',#41021,#33279,#33280);
#27634=AXIS2_PLACEMENT_3D('',#41023,#33281,#33282);
#27635=AXIS2_PLACEMENT_3D('',#41025,#33283,#33284);
#27636=AXIS2_PLACEMENT_3D('',#41027,#33285,#33286);
#27637=AXIS2_PLACEMENT_3D('',#41029,#33287,#33288);
#27638=AXIS2_PLACEMENT_3D('',#41030,#33289,#33290);
#27639=AXIS2_PLACEMENT_3D('',#41031,#33291,#33292);
#27640=AXIS2_PLACEMENT_3D('',#41034,#33293,#33294);
#27641=AXIS2_PLACEMENT_3D('',#41038,#33296,#33297);
#27642=AXIS2_PLACEMENT_3D('',#41040,#33299,#33300);
#27643=AXIS2_PLACEMENT_3D('',#41043,#33301,#33302);
#27644=AXIS2_PLACEMENT_3D('',#41047,#33304,#33305);
#27645=AXIS2_PLACEMENT_3D('',#41049,#33307,#33308);
#27646=AXIS2_PLACEMENT_3D('',#41052,#33309,#33310);
#27647=AXIS2_PLACEMENT_3D('',#41056,#33312,#33313);
#27648=AXIS2_PLACEMENT_3D('',#41058,#33315,#33316);
#27649=AXIS2_PLACEMENT_3D('',#41059,#33317,#33318);
#27650=AXIS2_PLACEMENT_3D('',#41064,#33323,#33324);
#27651=AXIS2_PLACEMENT_3D('',#41069,#33329,#33330);
#27652=AXIS2_PLACEMENT_3D('',#41070,#33331,#33332);
#27653=AXIS2_PLACEMENT_3D('',#41071,#33333,#33334);
#27654=AXIS2_PLACEMENT_3D('',#41072,#33335,#33336);
#27655=AXIS2_PLACEMENT_3D('',#41073,#33337,#33338);
#27656=AXIS2_PLACEMENT_3D('',#41074,#33339,#33340);
#27657=AXIS2_PLACEMENT_3D('',#41081,#33345,#33346);
#27658=AXIS2_PLACEMENT_3D('',#41086,#33350,#33351);
#27659=AXIS2_PLACEMENT_3D('',#41091,#33355,#33356);
#27660=AXIS2_PLACEMENT_3D('',#41096,#33360,#33361);
#27661=AXIS2_PLACEMENT_3D('',#41101,#33365,#33366);
#27662=AXIS2_PLACEMENT_3D('',#41104,#33369,#33370);
#27663=AXIS2_PLACEMENT_3D('',#41105,#33371,#33372);
#27664=AXIS2_PLACEMENT_3D('',#41106,#33373,#33374);
#27665=AXIS2_PLACEMENT_3D('',#41107,#33375,#33376);
#27666=AXIS2_PLACEMENT_3D('',#41108,#33377,#33378);
#27667=AXIS2_PLACEMENT_3D('',#41109,#33379,#33380);
#27668=AXIS2_PLACEMENT_3D('',#41110,#33381,#33382);
#27669=AXIS2_PLACEMENT_3D('',#41111,#33383,#33384);
#27670=AXIS2_PLACEMENT_3D('',#41113,#33385,#33386);
#27671=AXIS2_PLACEMENT_3D('',#41116,#33388,#33389);
#27672=AXIS2_PLACEMENT_3D('',#41117,#33390,#33391);
#27673=AXIS2_PLACEMENT_3D('',#41119,#33392,#33393);
#27674=AXIS2_PLACEMENT_3D('',#41122,#33395,#33396);
#27675=AXIS2_PLACEMENT_3D('',#41123,#33397,#33398);
#27676=AXIS2_PLACEMENT_3D('',#41124,#33399,#33400);
#27677=AXIS2_PLACEMENT_3D('',#41125,#33401,#33402);
#27678=AXIS2_PLACEMENT_3D('',#41126,#33403,#33404);
#27679=AXIS2_PLACEMENT_3D('',#41127,#33405,#33406);
#27680=AXIS2_PLACEMENT_3D('',#41128,#33407,#33408);
#27681=AXIS2_PLACEMENT_3D('',#41129,#33409,#33410);
#27682=AXIS2_PLACEMENT_3D('',#41130,#33411,#33412);
#27683=AXIS2_PLACEMENT_3D('',#41132,#33413,#33414);
#27684=AXIS2_PLACEMENT_3D('',#41135,#33416,#33417);
#27685=AXIS2_PLACEMENT_3D('',#41136,#33418,#33419);
#27686=AXIS2_PLACEMENT_3D('',#41138,#33420,#33421);
#27687=AXIS2_PLACEMENT_3D('',#41141,#33423,#33424);
#27688=AXIS2_PLACEMENT_3D('',#41142,#33425,#33426);
#27689=AXIS2_PLACEMENT_3D('',#41144,#33427,#33428);
#27690=AXIS2_PLACEMENT_3D('',#41147,#33430,#33431);
#27691=AXIS2_PLACEMENT_3D('',#41148,#33432,#33433);
#27692=AXIS2_PLACEMENT_3D('',#41150,#33434,#33435);
#27693=AXIS2_PLACEMENT_3D('',#41153,#33437,#33438);
#27694=AXIS2_PLACEMENT_3D('',#41154,#33439,#33440);
#27695=AXIS2_PLACEMENT_3D('',#41156,#33441,#33442);
#27696=AXIS2_PLACEMENT_3D('',#41159,#33444,#33445);
#27697=AXIS2_PLACEMENT_3D('',#41160,#33446,#33447);
#27698=AXIS2_PLACEMENT_3D('',#41162,#33448,#33449);
#27699=AXIS2_PLACEMENT_3D('',#41165,#33451,#33452);
#27700=AXIS2_PLACEMENT_3D('',#41166,#33453,#33454);
#27701=AXIS2_PLACEMENT_3D('',#41175,#33459,#33460);
#27702=AXIS2_PLACEMENT_3D('',#41185,#33466,#33467);
#27703=AXIS2_PLACEMENT_3D('',#41193,#33472,#33473);
#27704=AXIS2_PLACEMENT_3D('',#41203,#33479,#33480);
#27705=AXIS2_PLACEMENT_3D('',#41210,#33485,#33486);
#27706=AXIS2_PLACEMENT_3D('',#41214,#33489,#33490);
#27707=AXIS2_PLACEMENT_3D('',#41215,#33491,#33492);
#27708=AXIS2_PLACEMENT_3D('',#41219,#33495,#33496);
#27709=AXIS2_PLACEMENT_3D('',#41221,#33498,#33499);
#27710=AXIS2_PLACEMENT_3D('',#41225,#33502,#33503);
#27711=AXIS2_PLACEMENT_3D('',#41227,#33505,#33506);
#27712=AXIS2_PLACEMENT_3D('',#41228,#33507,#33508);
#27713=AXIS2_PLACEMENT_3D('',#41229,#33509,#33510);
#27714=AXIS2_PLACEMENT_3D('',#41230,#33511,#33512);
#27715=AXIS2_PLACEMENT_3D('',#41231,#33513,#33514);
#27716=AXIS2_PLACEMENT_3D('',#41233,#33515,#33516);
#27717=AXIS2_PLACEMENT_3D('',#41234,#33517,#33518);
#27718=AXIS2_PLACEMENT_3D('',#41237,#33520,#33521);
#27719=AXIS2_PLACEMENT_3D('',#41238,#33522,#33523);
#27720=AXIS2_PLACEMENT_3D('',#41240,#33524,#33525);
#27721=AXIS2_PLACEMENT_3D('',#41241,#33526,#33527);
#27722=AXIS2_PLACEMENT_3D('',#41243,#33528,#33529);
#27723=AXIS2_PLACEMENT_3D('',#41287,#33531,#33532);
#27724=AXIS2_PLACEMENT_3D('',#41500,#33533,#33534);
#27725=AXIS2_PLACEMENT_3D('',#41600,#33535,#33536);
#27726=AXIS2_PLACEMENT_3D('',#41602,#33537,#33538);
#27727=AXIS2_PLACEMENT_3D('',#41603,#33539,#33540);
#27728=AXIS2_PLACEMENT_3D('',#41604,#33541,#33542);
#27729=AXIS2_PLACEMENT_3D('',#41605,#33543,#33544);
#27730=AXIS2_PLACEMENT_3D('',#41606,#33545,#33546);
#27731=AXIS2_PLACEMENT_3D('',#41839,#33547,#33548);
#27732=AXIS2_PLACEMENT_3D('',#42537,#33549,#33550);
#27733=AXIS2_PLACEMENT_3D('',#42629,#33551,#33552);
#27734=AXIS2_PLACEMENT_3D('',#42630,#33553,#33554);
#27735=AXIS2_PLACEMENT_3D('',#42947,#33555,#33556);
#27736=AXIS2_PLACEMENT_3D('',#43006,#33557,#33558);
#27737=AXIS2_PLACEMENT_3D('',#43008,#33559,#33560);
#27738=AXIS2_PLACEMENT_3D('',#43009,#33561,#33562);
#27739=AXIS2_PLACEMENT_3D('',#43034,#33563,#33564);
#27740=AXIS2_PLACEMENT_3D('',#43035,#33565,#33566);
#27741=AXIS2_PLACEMENT_3D('',#43351,#33567,#33568);
#27742=AXIS2_PLACEMENT_3D('',#43509,#33569,#33570);
#27743=AXIS2_PLACEMENT_3D('',#43510,#33571,#33572);
#27744=AXIS2_PLACEMENT_3D('',#43608,#33573,#33574);
#27745=AXIS2_PLACEMENT_3D('',#44397,#33575,#33576);
#27746=AXIS2_PLACEMENT_3D('',#44497,#33577,#33578);
#27747=AXIS2_PLACEMENT_3D('',#44499,#33579,#33580);
#27748=AXIS2_PLACEMENT_3D('',#44500,#33581,#33582);
#27749=AXIS2_PLACEMENT_3D('',#44501,#33583,#33584);
#27750=AXIS2_PLACEMENT_3D('',#44502,#33585,#33586);
#27751=AXIS2_PLACEMENT_3D('',#44503,#33587,#33588);
#27752=AXIS2_PLACEMENT_3D('',#44736,#33589,#33590);
#27753=AXIS2_PLACEMENT_3D('',#45071,#33591,#33592);
#27754=AXIS2_PLACEMENT_3D('',#45347,#33593,#33594);
#27755=AXIS2_PLACEMENT_3D('',#45439,#33595,#33596);
#27756=AXIS2_PLACEMENT_3D('',#45440,#33597,#33598);
#27757=AXIS2_PLACEMENT_3D('',#45763,#33599,#33600);
#27758=AXIS2_PLACEMENT_3D('',#45822,#33601,#33602);
#27759=AXIS2_PLACEMENT_3D('',#45824,#33603,#33604);
#27760=AXIS2_PLACEMENT_3D('',#45825,#33605,#33606);
#27761=AXIS2_PLACEMENT_3D('',#45850,#33607,#33608);
#27762=AXIS2_PLACEMENT_3D('',#45851,#33609,#33610);
#27763=AXIS2_PLACEMENT_3D('',#46167,#33611,#33612);
#27764=AXIS2_PLACEMENT_3D('',#46325,#33613,#33614);
#27765=AXIS2_PLACEMENT_3D('',#46326,#33615,#33616);
#27766=AXIS2_PLACEMENT_3D('',#46423,#33617,#33618);
#27767=AXIS2_PLACEMENT_3D('',#47181,#33619,#33620);
#27768=AXIS2_PLACEMENT_3D('',#47281,#33621,#33622);
#27769=AXIS2_PLACEMENT_3D('',#47283,#33623,#33624);
#27770=AXIS2_PLACEMENT_3D('',#47284,#33625,#33626);
#27771=AXIS2_PLACEMENT_3D('',#47285,#33627,#33628);
#27772=AXIS2_PLACEMENT_3D('',#47286,#33629,#33630);
#27773=AXIS2_PLACEMENT_3D('',#47287,#33631,#33632);
#27774=AXIS2_PLACEMENT_3D('',#47520,#33633,#33634);
#27775=AXIS2_PLACEMENT_3D('',#48198,#33635,#33636);
#27776=AXIS2_PLACEMENT_3D('',#48290,#33637,#33638);
#27777=AXIS2_PLACEMENT_3D('',#48291,#33639,#33640);
#27778=AXIS2_PLACEMENT_3D('',#48616,#33641,#33642);
#27779=AXIS2_PLACEMENT_3D('',#48675,#33643,#33644);
#27780=AXIS2_PLACEMENT_3D('',#48677,#33645,#33646);
#27781=AXIS2_PLACEMENT_3D('',#48678,#33647,#33648);
#27782=AXIS2_PLACEMENT_3D('',#48703,#33649,#33650);
#27783=AXIS2_PLACEMENT_3D('',#48704,#33651,#33652);
#27784=AXIS2_PLACEMENT_3D('',#49053,#33653,#33654);
#27785=AXIS2_PLACEMENT_3D('',#49211,#33655,#33656);
#27786=AXIS2_PLACEMENT_3D('',#49212,#33657,#33658);
#27787=AXIS2_PLACEMENT_3D('',#49309,#33659,#33660);
#27788=AXIS2_PLACEMENT_3D('',#49808,#33661,#33662);
#27789=AXIS2_PLACEMENT_3D('',#50021,#33663,#33664);
#27790=AXIS2_PLACEMENT_3D('',#50121,#33665,#33666);
#27791=AXIS2_PLACEMENT_3D('',#50123,#33667,#33668);
#27792=AXIS2_PLACEMENT_3D('',#50124,#33669,#33670);
#27793=AXIS2_PLACEMENT_3D('',#50125,#33671,#33672);
#27794=AXIS2_PLACEMENT_3D('',#50126,#33673,#33674);
#27795=AXIS2_PLACEMENT_3D('',#50127,#33675,#33676);
#27796=AXIS2_PLACEMENT_3D('',#50360,#33677,#33678);
#27797=AXIS2_PLACEMENT_3D('',#51055,#33679,#33680);
#27798=AXIS2_PLACEMENT_3D('',#51147,#33681,#33682);
#27799=AXIS2_PLACEMENT_3D('',#51148,#33683,#33684);
#27800=AXIS2_PLACEMENT_3D('',#51195,#33685,#33686);
#27801=AXIS2_PLACEMENT_3D('',#51419,#33687,#33688);
#27802=AXIS2_PLACEMENT_3D('',#51478,#33689,#33690);
#27803=AXIS2_PLACEMENT_3D('',#51480,#33691,#33692);
#27804=AXIS2_PLACEMENT_3D('',#51481,#33693,#33694);
#27805=AXIS2_PLACEMENT_3D('',#51506,#33695,#33696);
#27806=AXIS2_PLACEMENT_3D('',#51507,#33697,#33698);
#27807=AXIS2_PLACEMENT_3D('',#51853,#33699,#33700);
#27808=AXIS2_PLACEMENT_3D('',#52011,#33701,#33702);
#27809=AXIS2_PLACEMENT_3D('',#52012,#33703,#33704);
#27810=AXIS2_PLACEMENT_3D('',#52113,#33705,#33706);
#27811=AXIS2_PLACEMENT_3D('',#52887,#33707,#33708);
#27812=AXIS2_PLACEMENT_3D('',#52987,#33709,#33710);
#27813=AXIS2_PLACEMENT_3D('',#52989,#33711,#33712);
#27814=AXIS2_PLACEMENT_3D('',#52990,#33713,#33714);
#27815=AXIS2_PLACEMENT_3D('',#52991,#33715,#33716);
#27816=AXIS2_PLACEMENT_3D('',#52992,#33717,#33718);
#27817=AXIS2_PLACEMENT_3D('',#52993,#33719,#33720);
#27818=AXIS2_PLACEMENT_3D('',#53226,#33721,#33722);
#27819=AXIS2_PLACEMENT_3D('',#53561,#33723,#33724);
#27820=AXIS2_PLACEMENT_3D('',#53837,#33725,#33726);
#27821=AXIS2_PLACEMENT_3D('',#53929,#33727,#33728);
#27822=AXIS2_PLACEMENT_3D('',#53930,#33729,#33730);
#27823=AXIS2_PLACEMENT_3D('',#54280,#33731,#33732);
#27824=AXIS2_PLACEMENT_3D('',#54339,#33733,#33734);
#27825=AXIS2_PLACEMENT_3D('',#54341,#33735,#33736);
#27826=AXIS2_PLACEMENT_3D('',#54342,#33737,#33738);
#27827=AXIS2_PLACEMENT_3D('',#54367,#33739,#33740);
#27828=AXIS2_PLACEMENT_3D('',#54368,#33741,#33742);
#27829=AXIS2_PLACEMENT_3D('',#54714,#33743,#33744);
#27830=AXIS2_PLACEMENT_3D('',#54872,#33745,#33746);
#27831=AXIS2_PLACEMENT_3D('',#54873,#33747,#33748);
#27832=AXIS2_PLACEMENT_3D('',#55808,#33749,#33750);
#27833=AXIS2_PLACEMENT_3D('',#55908,#33751,#33752);
#27834=AXIS2_PLACEMENT_3D('',#55910,#33753,#33754);
#27835=AXIS2_PLACEMENT_3D('',#55911,#33755,#33756);
#27836=AXIS2_PLACEMENT_3D('',#55912,#33757,#33758);
#27837=AXIS2_PLACEMENT_3D('',#55913,#33759,#33760);
#27838=AXIS2_PLACEMENT_3D('',#55914,#33761,#33762);
#27839=AXIS2_PLACEMENT_3D('',#56147,#33763,#33764);
#27840=AXIS2_PLACEMENT_3D('',#56822,#33765,#33766);
#27841=AXIS2_PLACEMENT_3D('',#56914,#33767,#33768);
#27842=AXIS2_PLACEMENT_3D('',#56915,#33769,#33770);
#27843=AXIS2_PLACEMENT_3D('',#56954,#33771,#33772);
#27844=AXIS2_PLACEMENT_3D('',#57175,#33773,#33774);
#27845=AXIS2_PLACEMENT_3D('',#57234,#33775,#33776);
#27846=AXIS2_PLACEMENT_3D('',#57236,#33777,#33778);
#27847=AXIS2_PLACEMENT_3D('',#57237,#33779,#33780);
#27848=AXIS2_PLACEMENT_3D('',#57262,#33781,#33782);
#27849=AXIS2_PLACEMENT_3D('',#57263,#33783,#33784);
#27850=AXIS2_PLACEMENT_3D('',#57606,#33785,#33786);
#27851=AXIS2_PLACEMENT_3D('',#57764,#33787,#33788);
#27852=AXIS2_PLACEMENT_3D('',#57765,#33789,#33790);
#27853=AXIS2_PLACEMENT_3D('',#57863,#33791,#33792);
#27854=AXIS2_PLACEMENT_3D('',#58434,#33793,#33794);
#27855=AXIS2_PLACEMENT_3D('',#59243,#33795,#33796);
#27856=AXIS2_PLACEMENT_3D('',#59411,#33797,#33798);
#27857=AXIS2_PLACEMENT_3D('',#59412,#33799,#33800);
#27858=AXIS2_PLACEMENT_3D('',#59413,#33801,#33802);
#27859=AXIS2_PLACEMENT_3D('',#59440,#33803,#33804);
#27860=AXIS2_PLACEMENT_3D('',#59441,#33805,#33806);
#27861=AXIS2_PLACEMENT_3D('',#59442,#33807,#33808);
#27862=AXIS2_PLACEMENT_3D('',#59678,#33809,#33810);
#27863=AXIS2_PLACEMENT_3D('',#59760,#33811,#33812);
#27864=AXIS2_PLACEMENT_3D('',#59919,#33813,#33814);
#27865=AXIS2_PLACEMENT_3D('',#59920,#33815,#33816);
#27866=AXIS2_PLACEMENT_3D('',#59921,#33817,#33818);
#27867=AXIS2_PLACEMENT_3D('',#60015,#33819,#33820);
#27868=AXIS2_PLACEMENT_3D('',#60532,#33821,#33822);
#27869=AXIS2_PLACEMENT_3D('',#60792,#33823,#33824);
#27870=AXIS2_PLACEMENT_3D('',#60793,#33825,#33826);
#27871=AXIS2_PLACEMENT_3D('',#60794,#33827,#33828);
#27872=AXIS2_PLACEMENT_3D('',#60820,#33829,#33830);
#27873=AXIS2_PLACEMENT_3D('',#60821,#33831,#33832);
#27874=AXIS2_PLACEMENT_3D('',#60822,#33833,#33834);
#27875=AXIS2_PLACEMENT_3D('',#60823,#33835,#33836);
#27876=AXIS2_PLACEMENT_3D('',#61155,#33837,#33838);
#27877=AXIS2_PLACEMENT_3D('',#61359,#33839,#33840);
#27878=AXIS2_PLACEMENT_3D('',#61459,#33841,#33842);
#27879=AXIS2_PLACEMENT_3D('',#61461,#33843,#33844);
#27880=AXIS2_PLACEMENT_3D('',#61462,#33845,#33846);
#27881=AXIS2_PLACEMENT_3D('',#61463,#33847,#33848);
#27882=AXIS2_PLACEMENT_3D('',#61464,#33849,#33850);
#27883=AXIS2_PLACEMENT_3D('',#61465,#33851,#33852);
#27884=AXIS2_PLACEMENT_3D('',#61698,#33853,#33854);
#27885=AXIS2_PLACEMENT_3D('',#62037,#33855,#33856);
#27886=AXIS2_PLACEMENT_3D('',#62317,#33857,#33858);
#27887=AXIS2_PLACEMENT_3D('',#62409,#33859,#33860);
#27888=AXIS2_PLACEMENT_3D('',#62410,#33861,#33862);
#27889=AXIS2_PLACEMENT_3D('',#62728,#33863,#33864);
#27890=AXIS2_PLACEMENT_3D('',#62787,#33865,#33866);
#27891=AXIS2_PLACEMENT_3D('',#62789,#33867,#33868);
#27892=AXIS2_PLACEMENT_3D('',#62790,#33869,#33870);
#27893=AXIS2_PLACEMENT_3D('',#62815,#33871,#33872);
#27894=AXIS2_PLACEMENT_3D('',#62816,#33873,#33874);
#27895=AXIS2_PLACEMENT_3D('',#63162,#33875,#33876);
#27896=AXIS2_PLACEMENT_3D('',#63320,#33877,#33878);
#27897=AXIS2_PLACEMENT_3D('',#63321,#33879,#33880);
#27898=AXIS2_PLACEMENT_3D('',#63413,#33881,#33882);
#27899=AXIS2_PLACEMENT_3D('',#63886,#33883,#33884);
#27900=AXIS2_PLACEMENT_3D('',#63887,#33885,#33886);
#27901=AXIS2_PLACEMENT_3D('',#63897,#33887,#33888);
#27902=AXIS2_PLACEMENT_3D('',#63898,#33889,#33890);
#27903=AXIS2_PLACEMENT_3D('',#63908,#33891,#33892);
#27904=AXIS2_PLACEMENT_3D('',#63909,#33893,#33894);
#27905=AXIS2_PLACEMENT_3D('',#63919,#33895,#33896);
#27906=AXIS2_PLACEMENT_3D('',#63920,#33897,#33898);
#27907=AXIS2_PLACEMENT_3D('',#63930,#33899,#33900);
#27908=AXIS2_PLACEMENT_3D('',#63931,#33901,#33902);
#27909=AXIS2_PLACEMENT_3D('',#63941,#33903,#33904);
#27910=AXIS2_PLACEMENT_3D('',#63942,#33905,#33906);
#27911=AXIS2_PLACEMENT_3D('',#63952,#33907,#33908);
#27912=AXIS2_PLACEMENT_3D('',#63953,#33909,#33910);
#27913=AXIS2_PLACEMENT_3D('',#63963,#33911,#33912);
#27914=AXIS2_PLACEMENT_3D('',#63964,#33913,#33914);
#27915=AXIS2_PLACEMENT_3D('',#63965,#33915,#33916);
#27916=AXIS2_PLACEMENT_3D('',#63967,#33917,#33918);
#27917=AXIS2_PLACEMENT_3D('',#63968,#33919,#33920);
#27918=AXIS2_PLACEMENT_3D('',#63970,#33921,#33922);
#27919=AXIS2_PLACEMENT_3D('',#63972,#33924,#33925);
#27920=AXIS2_PLACEMENT_3D('',#63974,#33926,#33927);
#27921=AXIS2_PLACEMENT_3D('',#63975,#33928,#33929);
#27922=AXIS2_PLACEMENT_3D('',#63977,#33930,#33931);
#27923=AXIS2_PLACEMENT_3D('',#63979,#33933,#33934);
#27924=AXIS2_PLACEMENT_3D('',#63981,#33935,#33936);
#27925=AXIS2_PLACEMENT_3D('',#63982,#33937,#33938);
#27926=AXIS2_PLACEMENT_3D('',#63984,#33939,#33940);
#27927=AXIS2_PLACEMENT_3D('',#63986,#33942,#33943);
#27928=AXIS2_PLACEMENT_3D('',#63988,#33944,#33945);
#27929=AXIS2_PLACEMENT_3D('',#63989,#33946,#33947);
#27930=AXIS2_PLACEMENT_3D('',#63991,#33948,#33949);
#27931=AXIS2_PLACEMENT_3D('',#63993,#33951,#33952);
#27932=AXIS2_PLACEMENT_3D('',#63995,#33953,#33954);
#27933=AXIS2_PLACEMENT_3D('',#63996,#33955,#33956);
#27934=AXIS2_PLACEMENT_3D('',#63999,#33958,#33959);
#27935=AXIS2_PLACEMENT_3D('',#64000,#33960,#33961);
#27936=AXIS2_PLACEMENT_3D('',#64002,#33962,#33963);
#27937=AXIS2_PLACEMENT_3D('',#64003,#33964,#33965);
#27938=AXIS2_PLACEMENT_3D('',#64006,#33967,#33968);
#27939=AXIS2_PLACEMENT_3D('',#64007,#33969,#33970);
#27940=AXIS2_PLACEMENT_3D('',#64009,#33971,#33972);
#27941=AXIS2_PLACEMENT_3D('',#64010,#33973,#33974);
#27942=AXIS2_PLACEMENT_3D('',#64013,#33976,#33977);
#27943=AXIS2_PLACEMENT_3D('',#64014,#33978,#33979);
#27944=AXIS2_PLACEMENT_3D('',#64015,#33980,#33981);
#27945=AXIS2_PLACEMENT_3D('',#64016,#33982,#33983);
#27946=AXIS2_PLACEMENT_3D('',#64018,#33984,#33985);
#27947=AXIS2_PLACEMENT_3D('',#64031,#33992,#33993);
#27948=AXIS2_PLACEMENT_3D('',#64033,#33994,#33995);
#27949=AXIS2_PLACEMENT_3D('',#64034,#33996,#33997);
#27950=AXIS2_PLACEMENT_3D('',#64036,#33999,#34000);
#27951=AXIS2_PLACEMENT_3D('',#64049,#34007,#34008);
#27952=AXIS2_PLACEMENT_3D('',#64052,#34011,#34012);
#27953=AXIS2_PLACEMENT_3D('',#64054,#34014,#34015);
#27954=AXIS2_PLACEMENT_3D('',#64056,#34017,#34018);
#27955=AXIS2_PLACEMENT_3D('',#64058,#34020,#34021);
#27956=AXIS2_PLACEMENT_3D('',#64060,#34023,#34024);
#27957=AXIS2_PLACEMENT_3D('',#64061,#34025,#34026);
#27958=AXIS2_PLACEMENT_3D('',#64062,#34027,#34028);
#27959=AXIS2_PLACEMENT_3D('',#64064,#34029,#34030);
#27960=AXIS2_PLACEMENT_3D('',#64066,#34031,#34032);
#27961=AXIS2_PLACEMENT_3D('',#64067,#34033,#34034);
#27962=AXIS2_PLACEMENT_3D('',#64070,#34036,#34037);
#27963=AXIS2_PLACEMENT_3D('',#64071,#34038,#34039);
#27964=AXIS2_PLACEMENT_3D('',#64073,#34040,#34041);
#27965=AXIS2_PLACEMENT_3D('',#64074,#34042,#34043);
#27966=AXIS2_PLACEMENT_3D('',#64075,#34044,#34045);
#27967=AXIS2_PLACEMENT_3D('',#64088,#34052,#34053);
#27968=AXIS2_PLACEMENT_3D('',#64101,#34060,#34061);
#27969=AXIS2_PLACEMENT_3D('',#64104,#34064,#34065);
#27970=AXIS2_PLACEMENT_3D('',#64106,#34067,#34068);
#27971=AXIS2_PLACEMENT_3D('',#64108,#34070,#34071);
#27972=AXIS2_PLACEMENT_3D('',#64110,#34073,#34074);
#27973=AXIS2_PLACEMENT_3D('',#64112,#34076,#34077);
#27974=AXIS2_PLACEMENT_3D('',#64113,#34078,#34079);
#27975=AXIS2_PLACEMENT_3D('',#64115,#34080,#34081);
#27976=AXIS2_PLACEMENT_3D('',#64116,#34082,#34083);
#27977=AXIS2_PLACEMENT_3D('',#64118,#34084,#34085);
#27978=AXIS2_PLACEMENT_3D('',#64120,#34087,#34088);
#27979=AXIS2_PLACEMENT_3D('',#64122,#34090,#34091);
#27980=AXIS2_PLACEMENT_3D('',#64123,#34092,#34093);
#27981=AXIS2_PLACEMENT_3D('',#64125,#34094,#34095);
#27982=AXIS2_PLACEMENT_3D('',#64127,#34096,#34097);
#27983=AXIS2_PLACEMENT_3D('',#64128,#34098,#34099);
#27984=AXIS2_PLACEMENT_3D('',#64131,#34101,#34102);
#27985=AXIS2_PLACEMENT_3D('',#64132,#34103,#34104);
#27986=AXIS2_PLACEMENT_3D('',#64134,#34105,#34106);
#27987=AXIS2_PLACEMENT_3D('',#64135,#34107,#34108);
#27988=AXIS2_PLACEMENT_3D('',#64136,#34109,#34110);
#27989=AXIS2_PLACEMENT_3D('',#64149,#34117,#34118);
#27990=AXIS2_PLACEMENT_3D('',#64162,#34125,#34126);
#27991=AXIS2_PLACEMENT_3D('',#64165,#34129,#34130);
#27992=AXIS2_PLACEMENT_3D('',#64167,#34132,#34133);
#27993=AXIS2_PLACEMENT_3D('',#64169,#34135,#34136);
#27994=AXIS2_PLACEMENT_3D('',#64171,#34138,#34139);
#27995=AXIS2_PLACEMENT_3D('',#64173,#34141,#34142);
#27996=AXIS2_PLACEMENT_3D('',#64174,#34143,#34144);
#27997=AXIS2_PLACEMENT_3D('',#64176,#34145,#34146);
#27998=AXIS2_PLACEMENT_3D('',#64177,#34147,#34148);
#27999=AXIS2_PLACEMENT_3D('',#64179,#34149,#34150);
#28000=AXIS2_PLACEMENT_3D('',#64181,#34152,#34153);
#28001=AXIS2_PLACEMENT_3D('',#64183,#34155,#34156);
#28002=AXIS2_PLACEMENT_3D('',#64184,#34157,#34158);
#28003=AXIS2_PLACEMENT_3D('',#64189,#34160,#34161);
#28004=AXIS2_PLACEMENT_3D('',#64192,#34163,#34164);
#28005=AXIS2_PLACEMENT_3D('',#64193,#34165,#34166);
#28006=AXIS2_PLACEMENT_3D('',#64196,#34167,#34168);
#28007=AXIS2_PLACEMENT_3D('',#64199,#34171,#34172);
#28008=AXIS2_PLACEMENT_3D('',#64202,#34173,#34174);
#28009=AXIS2_PLACEMENT_3D('',#64204,#34175,#34176);
#28010=AXIS2_PLACEMENT_3D('',#64206,#34177,#34178);
#28011=AXIS2_PLACEMENT_3D('',#64207,#34179,#34180);
#28012=AXIS2_PLACEMENT_3D('',#64208,#34181,#34182);
#28013=AXIS2_PLACEMENT_3D('',#64211,#34183,#34184);
#28014=AXIS2_PLACEMENT_3D('',#64213,#34185,#34186);
#28015=AXIS2_PLACEMENT_3D('',#64215,#34187,#34188);
#28016=AXIS2_PLACEMENT_3D('',#64216,#34189,#34190);
#28017=AXIS2_PLACEMENT_3D('',#64217,#34191,#34192);
#28018=AXIS2_PLACEMENT_3D('',#64220,#34193,#34194);
#28019=AXIS2_PLACEMENT_3D('',#64223,#34197,#34198);
#28020=AXIS2_PLACEMENT_3D('',#64228,#34201,#34202);
#28021=AXIS2_PLACEMENT_3D('',#64229,#34203,#34204);
#28022=AXIS2_PLACEMENT_3D('',#64232,#34206,#34207);
#28023=AXIS2_PLACEMENT_3D('',#64233,#34208,#34209);
#28024=AXIS2_PLACEMENT_3D('',#64236,#34211,#34212);
#28025=AXIS2_PLACEMENT_3D('',#64237,#34213,#34214);
#28026=AXIS2_PLACEMENT_3D('',#64239,#34215,#34216);
#28027=AXIS2_PLACEMENT_3D('',#64241,#34218,#34219);
#28028=AXIS2_PLACEMENT_3D('',#64243,#34220,#34221);
#28029=AXIS2_PLACEMENT_3D('',#64245,#34223,#34224);
#28030=AXIS2_PLACEMENT_3D('',#64246,#34225,#34226);
#28031=AXIS2_PLACEMENT_3D('',#64248,#34227,#34228);
#28032=AXIS2_PLACEMENT_3D('',#64252,#34231,#34232);
#28033=AXIS2_PLACEMENT_3D('',#64331,#34234,#34235);
#28034=AXIS2_PLACEMENT_3D('',#64335,#34237,#34238);
#28035=AXIS2_PLACEMENT_3D('',#64337,#34240,#34241);
#28036=AXIS2_PLACEMENT_3D('',#64340,#34244,#34245);
#28037=AXIS2_PLACEMENT_3D('',#64343,#34247,#34248);
#28038=AXIS2_PLACEMENT_3D('',#64344,#34249,#34250);
#28039=AXIS2_PLACEMENT_3D('',#64345,#34251,#34252);
#28040=AXIS2_PLACEMENT_3D('',#64347,#34253,#34254);
#28041=AXIS2_PLACEMENT_3D('',#64348,#34255,#34256);
#28042=AXIS2_PLACEMENT_3D('',#64350,#34257,#34258);
#28043=AXIS2_PLACEMENT_3D('',#64352,#34260,#34261);
#28044=AXIS2_PLACEMENT_3D('',#64354,#34262,#34263);
#28045=AXIS2_PLACEMENT_3D('',#64355,#34264,#34265);
#28046=AXIS2_PLACEMENT_3D('',#64357,#34266,#34267);
#28047=AXIS2_PLACEMENT_3D('',#64359,#34269,#34270);
#28048=AXIS2_PLACEMENT_3D('',#64360,#34271,#34272);
#28049=AXIS2_PLACEMENT_3D('',#64361,#34273,#34274);
#28050=AXIS2_PLACEMENT_3D('',#64362,#34275,#34276);
#28051=AXIS2_PLACEMENT_3D('',#64365,#34277,#34278);
#28052=AXIS2_PLACEMENT_3D('',#64396,#34279,#34280);
#28053=AXIS2_PLACEMENT_3D('',#64408,#34286,#34287);
#28054=AXIS2_PLACEMENT_3D('',#64409,#34288,#34289);
#28055=AXIS2_PLACEMENT_3D('',#64453,#34291,#34292);
#28056=AXIS2_PLACEMENT_3D('',#64455,#34293,#34294);
#28057=AXIS2_PLACEMENT_3D('',#64458,#34296,#34297);
#28058=AXIS2_PLACEMENT_3D('',#64459,#34298,#34299);
#28059=AXIS2_PLACEMENT_3D('',#64461,#34300,#34301);
#28060=AXIS2_PLACEMENT_3D('',#64462,#34302,#34303);
#28061=AXIS2_PLACEMENT_3D('',#64465,#34305,#34306);
#28062=AXIS2_PLACEMENT_3D('',#64466,#34307,#34308);
#28063=AXIS2_PLACEMENT_3D('',#64468,#34310,#34311);
#28064=AXIS2_PLACEMENT_3D('',#64479,#34317,#34318);
#28065=AXIS2_PLACEMENT_3D('',#64481,#34319,#34320);
#28066=AXIS2_PLACEMENT_3D('',#64488,#34324,#34325);
#28067=AXIS2_PLACEMENT_3D('',#64489,#34326,#34327);
#28068=AXIS2_PLACEMENT_3D('',#64490,#34328,#34329);
#28069=AXIS2_PLACEMENT_3D('',#64491,#34330,#34331);
#28070=AXIS2_PLACEMENT_3D('',#64492,#34332,#34333);
#28071=AXIS2_PLACEMENT_3D('',#64494,#34334,#34335);
#28072=AXIS2_PLACEMENT_3D('',#64496,#34336,#34337);
#28073=AXIS2_PLACEMENT_3D('',#64498,#34338,#34339);
#28074=AXIS2_PLACEMENT_3D('',#64500,#34340,#34341);
#28075=AXIS2_PLACEMENT_3D('',#64502,#34342,#34343);
#28076=AXIS2_PLACEMENT_3D('',#64504,#34344,#34345);
#28077=AXIS2_PLACEMENT_3D('',#64506,#34346,#34347);
#28078=AXIS2_PLACEMENT_3D('',#64508,#34348,#34349);
#28079=AXIS2_PLACEMENT_3D('',#64509,#34350,#34351);
#28080=AXIS2_PLACEMENT_3D('',#64511,#34352,#34353);
#28081=AXIS2_PLACEMENT_3D('',#64518,#34357,#34358);
#28082=AXIS2_PLACEMENT_3D('',#64519,#34359,#34360);
#28083=AXIS2_PLACEMENT_3D('',#64530,#34363,#34364);
#28084=AXIS2_PLACEMENT_3D('',#64542,#34367,#34368);
#28085=AXIS2_PLACEMENT_3D('',#64567,#34371,#34372);
#28086=AXIS2_PLACEMENT_3D('',#64568,#34373,#34374);
#28087=AXIS2_PLACEMENT_3D('',#64571,#34375,#34376);
#28088=AXIS2_PLACEMENT_3D('',#64666,#34378,#34379);
#28089=AXIS2_PLACEMENT_3D('',#64671,#34382,#34383);
#28090=AXIS2_PLACEMENT_3D('',#64674,#34386,#34387);
#28091=AXIS2_PLACEMENT_3D('',#64676,#34389,#34390);
#28092=AXIS2_PLACEMENT_3D('',#64678,#34392,#34393);
#28093=AXIS2_PLACEMENT_3D('',#64680,#34395,#34396);
#28094=AXIS2_PLACEMENT_3D('',#64682,#34398,#34399);
#28095=AXIS2_PLACEMENT_3D('',#64683,#34400,#34401);
#28096=AXIS2_PLACEMENT_3D('',#64684,#34402,#34403);
#28097=AXIS2_PLACEMENT_3D('',#64687,#34404,#34405);
#28098=AXIS2_PLACEMENT_3D('',#64690,#34408,#34409);
#28099=AXIS2_PLACEMENT_3D('',#64693,#34410,#34411);
#28100=AXIS2_PLACEMENT_3D('',#64696,#34414,#34415);
#28101=AXIS2_PLACEMENT_3D('',#64700,#34417,#34418);
#28102=AXIS2_PLACEMENT_3D('',#64702,#34420,#34421);
#28103=AXIS2_PLACEMENT_3D('',#64704,#34422,#34423);
#28104=AXIS2_PLACEMENT_3D('',#64706,#34425,#34426);
#28105=AXIS2_PLACEMENT_3D('',#64707,#34427,#34428);
#28106=AXIS2_PLACEMENT_3D('',#64708,#34429,#34430);
#28107=AXIS2_PLACEMENT_3D('',#64711,#34432,#34433);
#28108=AXIS2_PLACEMENT_3D('',#64712,#34434,#34435);
#28109=AXIS2_PLACEMENT_3D('',#64713,#34436,#34437);
#28110=AXIS2_PLACEMENT_3D('',#64714,#34438,#34439);
#28111=AXIS2_PLACEMENT_3D('',#64715,#34440,#34441);
#28112=AXIS2_PLACEMENT_3D('',#64716,#34442,#34443);
#28113=AXIS2_PLACEMENT_3D('',#64736,#34444,#34445);
#28114=AXIS2_PLACEMENT_3D('',#64740,#34447,#34448);
#28115=AXIS2_PLACEMENT_3D('',#64744,#34450,#34451);
#28116=AXIS2_PLACEMENT_3D('',#64748,#34453,#34454);
#28117=AXIS2_PLACEMENT_3D('',#64752,#34456,#34457);
#28118=AXIS2_PLACEMENT_3D('',#64756,#34459,#34460);
#28119=AXIS2_PLACEMENT_3D('',#64760,#34462,#34463);
#28120=AXIS2_PLACEMENT_3D('',#64764,#34465,#34466);
#28121=AXIS2_PLACEMENT_3D('',#64770,#34469,#34470);
#28122=AXIS2_PLACEMENT_3D('',#64772,#34471,#34472);
#28123=AXIS2_PLACEMENT_3D('',#64776,#34474,#34475);
#28124=AXIS2_PLACEMENT_3D('',#64777,#34476,#34477);
#28125=AXIS2_PLACEMENT_3D('',#64780,#34478,#34479);
#28126=AXIS2_PLACEMENT_3D('',#64784,#34481,#34482);
#28127=AXIS2_PLACEMENT_3D('',#64786,#34483,#34484);
#28128=AXIS2_PLACEMENT_3D('',#64790,#34486,#34487);
#28129=AXIS2_PLACEMENT_3D('',#64794,#34489,#34490);
#28130=AXIS2_PLACEMENT_3D('',#64796,#34491,#34492);
#28131=AXIS2_PLACEMENT_3D('',#64799,#34494,#34495);
#28132=AXIS2_PLACEMENT_3D('',#64802,#34496,#34497);
#28133=AXIS2_PLACEMENT_3D('',#64806,#34499,#34500);
#28134=AXIS2_PLACEMENT_3D('',#64808,#34501,#34502);
#28135=AXIS2_PLACEMENT_3D('',#64811,#34504,#34505);
#28136=AXIS2_PLACEMENT_3D('',#64812,#34506,#34507);
#28137=AXIS2_PLACEMENT_3D('',#64815,#34508,#34509);
#28138=AXIS2_PLACEMENT_3D('',#64819,#34511,#34512);
#28139=AXIS2_PLACEMENT_3D('',#64823,#34514,#34515);
#28140=AXIS2_PLACEMENT_3D('',#64827,#34517,#34518);
#28141=AXIS2_PLACEMENT_3D('',#64829,#34520,#34521);
#28142=AXIS2_PLACEMENT_3D('',#64832,#34524,#34525);
#28143=AXIS2_PLACEMENT_3D('',#64834,#34527,#34528);
#28144=AXIS2_PLACEMENT_3D('',#64836,#34530,#34531);
#28145=AXIS2_PLACEMENT_3D('',#64838,#34533,#34534);
#28146=AXIS2_PLACEMENT_3D('',#64840,#34536,#34537);
#28147=AXIS2_PLACEMENT_3D('',#64842,#34539,#34540);
#28148=AXIS2_PLACEMENT_3D('',#64844,#34542,#34543);
#28149=AXIS2_PLACEMENT_3D('',#64845,#34544,#34545);
#28150=AXIS2_PLACEMENT_3D('',#64849,#34547,#34548);
#28151=AXIS2_PLACEMENT_3D('',#64851,#34550,#34551);
#28152=AXIS2_PLACEMENT_3D('',#64855,#34554,#34555);
#28153=AXIS2_PLACEMENT_3D('',#64858,#34557,#34558);
#28154=AXIS2_PLACEMENT_3D('',#64859,#34559,#34560);
#28155=AXIS2_PLACEMENT_3D('',#64865,#34564,#34565);
#28156=AXIS2_PLACEMENT_3D('',#64868,#34567,#34568);
#28157=AXIS2_PLACEMENT_3D('',#64869,#34569,#34570);
#28158=AXIS2_PLACEMENT_3D('',#64872,#34572,#34573);
#28159=AXIS2_PLACEMENT_3D('',#64873,#34574,#34575);
#28160=AXIS2_PLACEMENT_3D('',#64877,#34578,#34579);
#28161=AXIS2_PLACEMENT_3D('',#64880,#34581,#34582);
#28162=AXIS2_PLACEMENT_3D('',#64881,#34583,#34584);
#28163=AXIS2_PLACEMENT_3D('',#64885,#34587,#34588);
#28164=AXIS2_PLACEMENT_3D('',#64886,#34589,#34590);
#28165=AXIS2_PLACEMENT_3D('',#64887,#34591,#34592);
#28166=AXIS2_PLACEMENT_3D('',#64888,#34593,#34594);
#28167=AXIS2_PLACEMENT_3D('',#64889,#34595,#34596);
#28168=AXIS2_PLACEMENT_3D('',#64890,#34597,#34598);
#28169=AXIS2_PLACEMENT_3D('',#64893,#34599,#34600);
#28170=AXIS2_PLACEMENT_3D('',#64897,#34602,#34603);
#28171=AXIS2_PLACEMENT_3D('',#64899,#34604,#34605);
#28172=AXIS2_PLACEMENT_3D('',#64902,#34607,#34608);
#28173=AXIS2_PLACEMENT_3D('',#64903,#34609,#34610);
#28174=AXIS2_PLACEMENT_3D('',#64906,#34613,#34614);
#28175=AXIS2_PLACEMENT_3D('',#64908,#34616,#34617);
#28176=AXIS2_PLACEMENT_3D('',#64910,#34619,#34620);
#28177=AXIS2_PLACEMENT_3D('',#64912,#34622,#34623);
#28178=AXIS2_PLACEMENT_3D('',#64914,#34625,#34626);
#28179=AXIS2_PLACEMENT_3D('',#64915,#34627,#34628);
#28180=AXIS2_PLACEMENT_3D('',#64921,#34632,#34633);
#28181=AXIS2_PLACEMENT_3D('',#64924,#34635,#34636);
#28182=AXIS2_PLACEMENT_3D('',#64925,#34637,#34638);
#28183=AXIS2_PLACEMENT_3D('',#64928,#34640,#34641);
#28184=AXIS2_PLACEMENT_3D('',#64929,#34642,#34643);
#28185=AXIS2_PLACEMENT_3D('',#64933,#34646,#34647);
#28186=AXIS2_PLACEMENT_3D('',#64935,#34648,#34649);
#28187=AXIS2_PLACEMENT_3D('',#64937,#34651,#34652);
#28188=AXIS2_PLACEMENT_3D('',#64938,#34653,#34654);
#28189=AXIS2_PLACEMENT_3D('',#64939,#34655,#34656);
#28190=AXIS2_PLACEMENT_3D('',#64940,#34657,#34658);
#28191=AXIS2_PLACEMENT_3D('',#64944,#34660,#34661);
#28192=AXIS2_PLACEMENT_3D('',#64946,#34663,#34664);
#28193=AXIS2_PLACEMENT_3D('',#64950,#34667,#34668);
#28194=AXIS2_PLACEMENT_3D('',#64953,#34670,#34671);
#28195=AXIS2_PLACEMENT_3D('',#64954,#34672,#34673);
#28196=AXIS2_PLACEMENT_3D('',#64973,#34675,#34676);
#28197=AXIS2_PLACEMENT_3D('',#64977,#34679,#34680);
#28198=AXIS2_PLACEMENT_3D('',#64981,#34682,#34683);
#28199=AXIS2_PLACEMENT_3D('',#64983,#34685,#34686);
#28200=AXIS2_PLACEMENT_3D('',#64987,#34689,#34690);
#28201=AXIS2_PLACEMENT_3D('',#64990,#34692,#34693);
#28202=AXIS2_PLACEMENT_3D('',#64991,#34694,#34695);
#28203=AXIS2_PLACEMENT_3D('',#64995,#34698,#34699);
#28204=AXIS2_PLACEMENT_3D('',#64998,#34701,#34702);
#28205=AXIS2_PLACEMENT_3D('',#64999,#34703,#34704);
#28206=AXIS2_PLACEMENT_3D('',#65001,#34706,#34707);
#28207=AXIS2_PLACEMENT_3D('',#65022,#34709,#34710);
#28208=AXIS2_PLACEMENT_3D('',#65024,#34712,#34713);
#28209=AXIS2_PLACEMENT_3D('',#65025,#34714,#34715);
#28210=AXIS2_PLACEMENT_3D('',#65026,#34716,#34717);
#28211=AXIS2_PLACEMENT_3D('',#65028,#34718,#34719);
#28212=AXIS2_PLACEMENT_3D('',#65041,#34726,#34727);
#28213=AXIS2_PLACEMENT_3D('',#65043,#34728,#34729);
#28214=AXIS2_PLACEMENT_3D('',#65044,#34730,#34731);
#28215=AXIS2_PLACEMENT_3D('',#65046,#34733,#34734);
#28216=AXIS2_PLACEMENT_3D('',#65059,#34741,#34742);
#28217=AXIS2_PLACEMENT_3D('',#65062,#34745,#34746);
#28218=AXIS2_PLACEMENT_3D('',#65064,#34748,#34749);
#28219=AXIS2_PLACEMENT_3D('',#65066,#34751,#34752);
#28220=AXIS2_PLACEMENT_3D('',#65068,#34754,#34755);
#28221=AXIS2_PLACEMENT_3D('',#65070,#34757,#34758);
#28222=AXIS2_PLACEMENT_3D('',#65071,#34759,#34760);
#28223=AXIS2_PLACEMENT_3D('',#65072,#34761,#34762);
#28224=AXIS2_PLACEMENT_3D('',#65074,#34763,#34764);
#28225=AXIS2_PLACEMENT_3D('',#65076,#34765,#34766);
#28226=AXIS2_PLACEMENT_3D('',#65077,#34767,#34768);
#28227=AXIS2_PLACEMENT_3D('',#65080,#34770,#34771);
#28228=AXIS2_PLACEMENT_3D('',#65081,#34772,#34773);
#28229=AXIS2_PLACEMENT_3D('',#65083,#34774,#34775);
#28230=AXIS2_PLACEMENT_3D('',#65084,#34776,#34777);
#28231=AXIS2_PLACEMENT_3D('',#65085,#34778,#34779);
#28232=AXIS2_PLACEMENT_3D('',#65098,#34786,#34787);
#28233=AXIS2_PLACEMENT_3D('',#65111,#34794,#34795);
#28234=AXIS2_PLACEMENT_3D('',#65114,#34798,#34799);
#28235=AXIS2_PLACEMENT_3D('',#65116,#34801,#34802);
#28236=AXIS2_PLACEMENT_3D('',#65118,#34804,#34805);
#28237=AXIS2_PLACEMENT_3D('',#65120,#34807,#34808);
#28238=AXIS2_PLACEMENT_3D('',#65122,#34810,#34811);
#28239=AXIS2_PLACEMENT_3D('',#65123,#34812,#34813);
#28240=AXIS2_PLACEMENT_3D('',#65125,#34814,#34815);
#28241=AXIS2_PLACEMENT_3D('',#65126,#34816,#34817);
#28242=AXIS2_PLACEMENT_3D('',#65128,#34818,#34819);
#28243=AXIS2_PLACEMENT_3D('',#65130,#34821,#34822);
#28244=AXIS2_PLACEMENT_3D('',#65132,#34824,#34825);
#28245=AXIS2_PLACEMENT_3D('',#65133,#34826,#34827);
#28246=AXIS2_PLACEMENT_3D('',#65135,#34828,#34829);
#28247=AXIS2_PLACEMENT_3D('',#65137,#34830,#34831);
#28248=AXIS2_PLACEMENT_3D('',#65138,#34832,#34833);
#28249=AXIS2_PLACEMENT_3D('',#65141,#34835,#34836);
#28250=AXIS2_PLACEMENT_3D('',#65142,#34837,#34838);
#28251=AXIS2_PLACEMENT_3D('',#65144,#34839,#34840);
#28252=AXIS2_PLACEMENT_3D('',#65145,#34841,#34842);
#28253=AXIS2_PLACEMENT_3D('',#65146,#34843,#34844);
#28254=AXIS2_PLACEMENT_3D('',#65159,#34851,#34852);
#28255=AXIS2_PLACEMENT_3D('',#65172,#34859,#34860);
#28256=AXIS2_PLACEMENT_3D('',#65175,#34863,#34864);
#28257=AXIS2_PLACEMENT_3D('',#65177,#34866,#34867);
#28258=AXIS2_PLACEMENT_3D('',#65179,#34869,#34870);
#28259=AXIS2_PLACEMENT_3D('',#65181,#34872,#34873);
#28260=AXIS2_PLACEMENT_3D('',#65183,#34875,#34876);
#28261=AXIS2_PLACEMENT_3D('',#65184,#34877,#34878);
#28262=AXIS2_PLACEMENT_3D('',#65186,#34879,#34880);
#28263=AXIS2_PLACEMENT_3D('',#65187,#34881,#34882);
#28264=AXIS2_PLACEMENT_3D('',#65189,#34883,#34884);
#28265=AXIS2_PLACEMENT_3D('',#65191,#34886,#34887);
#28266=AXIS2_PLACEMENT_3D('',#65193,#34889,#34890);
#28267=AXIS2_PLACEMENT_3D('',#65194,#34891,#34892);
#28268=AXIS2_PLACEMENT_3D('',#65199,#34894,#34895);
#28269=AXIS2_PLACEMENT_3D('',#65202,#34897,#34898);
#28270=AXIS2_PLACEMENT_3D('',#65203,#34899,#34900);
#28271=AXIS2_PLACEMENT_3D('',#65206,#34901,#34902);
#28272=AXIS2_PLACEMENT_3D('',#65209,#34905,#34906);
#28273=AXIS2_PLACEMENT_3D('',#65212,#34907,#34908);
#28274=AXIS2_PLACEMENT_3D('',#65214,#34909,#34910);
#28275=AXIS2_PLACEMENT_3D('',#65216,#34911,#34912);
#28276=AXIS2_PLACEMENT_3D('',#65217,#34913,#34914);
#28277=AXIS2_PLACEMENT_3D('',#65218,#34915,#34916);
#28278=AXIS2_PLACEMENT_3D('',#65221,#34917,#34918);
#28279=AXIS2_PLACEMENT_3D('',#65223,#34919,#34920);
#28280=AXIS2_PLACEMENT_3D('',#65225,#34921,#34922);
#28281=AXIS2_PLACEMENT_3D('',#65226,#34923,#34924);
#28282=AXIS2_PLACEMENT_3D('',#65227,#34925,#34926);
#28283=AXIS2_PLACEMENT_3D('',#65230,#34927,#34928);
#28284=AXIS2_PLACEMENT_3D('',#65233,#34931,#34932);
#28285=AXIS2_PLACEMENT_3D('',#65238,#34935,#34936);
#28286=AXIS2_PLACEMENT_3D('',#65239,#34937,#34938);
#28287=AXIS2_PLACEMENT_3D('',#65242,#34940,#34941);
#28288=AXIS2_PLACEMENT_3D('',#65243,#34942,#34943);
#28289=AXIS2_PLACEMENT_3D('',#65246,#34945,#34946);
#28290=AXIS2_PLACEMENT_3D('',#65247,#34947,#34948);
#28291=AXIS2_PLACEMENT_3D('',#65249,#34949,#34950);
#28292=AXIS2_PLACEMENT_3D('',#65251,#34952,#34953);
#28293=AXIS2_PLACEMENT_3D('',#65253,#34954,#34955);
#28294=AXIS2_PLACEMENT_3D('',#65255,#34957,#34958);
#28295=AXIS2_PLACEMENT_3D('',#65256,#34959,#34960);
#28296=AXIS2_PLACEMENT_3D('',#65258,#34961,#34962);
#28297=AXIS2_PLACEMENT_3D('',#65262,#34965,#34966);
#28298=AXIS2_PLACEMENT_3D('',#65341,#34968,#34969);
#28299=AXIS2_PLACEMENT_3D('',#65345,#34971,#34972);
#28300=AXIS2_PLACEMENT_3D('',#65347,#34974,#34975);
#28301=AXIS2_PLACEMENT_3D('',#65350,#34978,#34979);
#28302=AXIS2_PLACEMENT_3D('',#65353,#34981,#34982);
#28303=AXIS2_PLACEMENT_3D('',#65354,#34983,#34984);
#28304=AXIS2_PLACEMENT_3D('',#65355,#34985,#34986);
#28305=AXIS2_PLACEMENT_3D('',#65357,#34987,#34988);
#28306=AXIS2_PLACEMENT_3D('',#65358,#34989,#34990);
#28307=AXIS2_PLACEMENT_3D('',#65360,#34991,#34992);
#28308=AXIS2_PLACEMENT_3D('',#65362,#34994,#34995);
#28309=AXIS2_PLACEMENT_3D('',#65364,#34996,#34997);
#28310=AXIS2_PLACEMENT_3D('',#65365,#34998,#34999);
#28311=AXIS2_PLACEMENT_3D('',#65367,#35000,#35001);
#28312=AXIS2_PLACEMENT_3D('',#65369,#35003,#35004);
#28313=AXIS2_PLACEMENT_3D('',#65370,#35005,#35006);
#28314=AXIS2_PLACEMENT_3D('',#65371,#35007,#35008);
#28315=AXIS2_PLACEMENT_3D('',#65372,#35009,#35010);
#28316=AXIS2_PLACEMENT_3D('',#65375,#35011,#35012);
#28317=AXIS2_PLACEMENT_3D('',#65406,#35013,#35014);
#28318=AXIS2_PLACEMENT_3D('',#65418,#35020,#35021);
#28319=AXIS2_PLACEMENT_3D('',#65419,#35022,#35023);
#28320=AXIS2_PLACEMENT_3D('',#65463,#35025,#35026);
#28321=AXIS2_PLACEMENT_3D('',#65465,#35027,#35028);
#28322=AXIS2_PLACEMENT_3D('',#65468,#35030,#35031);
#28323=AXIS2_PLACEMENT_3D('',#65469,#35032,#35033);
#28324=AXIS2_PLACEMENT_3D('',#65471,#35034,#35035);
#28325=AXIS2_PLACEMENT_3D('',#65472,#35036,#35037);
#28326=AXIS2_PLACEMENT_3D('',#65475,#35039,#35040);
#28327=AXIS2_PLACEMENT_3D('',#65476,#35041,#35042);
#28328=AXIS2_PLACEMENT_3D('',#65478,#35044,#35045);
#28329=AXIS2_PLACEMENT_3D('',#65489,#35051,#35052);
#28330=AXIS2_PLACEMENT_3D('',#65491,#35053,#35054);
#28331=AXIS2_PLACEMENT_3D('',#65498,#35058,#35059);
#28332=AXIS2_PLACEMENT_3D('',#65499,#35060,#35061);
#28333=AXIS2_PLACEMENT_3D('',#65500,#35062,#35063);
#28334=AXIS2_PLACEMENT_3D('',#65501,#35064,#35065);
#28335=AXIS2_PLACEMENT_3D('',#65502,#35066,#35067);
#28336=AXIS2_PLACEMENT_3D('',#65504,#35068,#35069);
#28337=AXIS2_PLACEMENT_3D('',#65506,#35070,#35071);
#28338=AXIS2_PLACEMENT_3D('',#65508,#35072,#35073);
#28339=AXIS2_PLACEMENT_3D('',#65510,#35074,#35075);
#28340=AXIS2_PLACEMENT_3D('',#65512,#35076,#35077);
#28341=AXIS2_PLACEMENT_3D('',#65514,#35078,#35079);
#28342=AXIS2_PLACEMENT_3D('',#65516,#35080,#35081);
#28343=AXIS2_PLACEMENT_3D('',#65518,#35082,#35083);
#28344=AXIS2_PLACEMENT_3D('',#65519,#35084,#35085);
#28345=AXIS2_PLACEMENT_3D('',#65521,#35086,#35087);
#28346=AXIS2_PLACEMENT_3D('',#65528,#35091,#35092);
#28347=AXIS2_PLACEMENT_3D('',#65529,#35093,#35094);
#28348=AXIS2_PLACEMENT_3D('',#65531,#35096,#35097);
#28349=AXIS2_PLACEMENT_3D('',#65533,#35099,#35100);
#28350=AXIS2_PLACEMENT_3D('',#65558,#35103,#35104);
#28351=AXIS2_PLACEMENT_3D('',#65559,#35105,#35106);
#28352=AXIS2_PLACEMENT_3D('',#65561,#35107,#35108);
#28353=AXIS2_PLACEMENT_3D('',#65655,#35110,#35111);
#28354=AXIS2_PLACEMENT_3D('',#65657,#35113,#35114);
#28355=AXIS2_PLACEMENT_3D('',#65659,#35116,#35117);
#28356=AXIS2_PLACEMENT_3D('',#65660,#35118,#35119);
#28357=AXIS2_PLACEMENT_3D('',#65663,#35120,#35121);
#28358=AXIS2_PLACEMENT_3D('',#65666,#35124,#35125);
#28359=AXIS2_PLACEMENT_3D('',#65669,#35126,#35127);
#28360=AXIS2_PLACEMENT_3D('',#65672,#35130,#35131);
#28361=AXIS2_PLACEMENT_3D('',#65676,#35133,#35134);
#28362=AXIS2_PLACEMENT_3D('',#65678,#35136,#35137);
#28363=AXIS2_PLACEMENT_3D('',#65680,#35138,#35139);
#28364=AXIS2_PLACEMENT_3D('',#65682,#35141,#35142);
#28365=AXIS2_PLACEMENT_3D('',#65683,#35143,#35144);
#28366=AXIS2_PLACEMENT_3D('',#65684,#35145,#35146);
#28367=AXIS2_PLACEMENT_3D('',#65687,#35148,#35149);
#28368=AXIS2_PLACEMENT_3D('',#65688,#35150,#35151);
#28369=AXIS2_PLACEMENT_3D('',#65689,#35152,#35153);
#28370=AXIS2_PLACEMENT_3D('',#65690,#35154,#35155);
#28371=AXIS2_PLACEMENT_3D('',#65691,#35156,#35157);
#28372=AXIS2_PLACEMENT_3D('',#65692,#35158,#35159);
#28373=AXIS2_PLACEMENT_3D('',#65712,#35160,#35161);
#28374=AXIS2_PLACEMENT_3D('',#65716,#35163,#35164);
#28375=AXIS2_PLACEMENT_3D('',#65720,#35166,#35167);
#28376=AXIS2_PLACEMENT_3D('',#65724,#35169,#35170);
#28377=AXIS2_PLACEMENT_3D('',#65728,#35172,#35173);
#28378=AXIS2_PLACEMENT_3D('',#65732,#35175,#35176);
#28379=AXIS2_PLACEMENT_3D('',#65736,#35178,#35179);
#28380=AXIS2_PLACEMENT_3D('',#65740,#35181,#35182);
#28381=AXIS2_PLACEMENT_3D('',#65746,#35185,#35186);
#28382=AXIS2_PLACEMENT_3D('',#65748,#35187,#35188);
#28383=AXIS2_PLACEMENT_3D('',#65752,#35190,#35191);
#28384=AXIS2_PLACEMENT_3D('',#65753,#35192,#35193);
#28385=AXIS2_PLACEMENT_3D('',#65756,#35194,#35195);
#28386=AXIS2_PLACEMENT_3D('',#65760,#35197,#35198);
#28387=AXIS2_PLACEMENT_3D('',#65762,#35199,#35200);
#28388=AXIS2_PLACEMENT_3D('',#65766,#35202,#35203);
#28389=AXIS2_PLACEMENT_3D('',#65770,#35205,#35206);
#28390=AXIS2_PLACEMENT_3D('',#65772,#35207,#35208);
#28391=AXIS2_PLACEMENT_3D('',#65775,#35210,#35211);
#28392=AXIS2_PLACEMENT_3D('',#65778,#35212,#35213);
#28393=AXIS2_PLACEMENT_3D('',#65782,#35215,#35216);
#28394=AXIS2_PLACEMENT_3D('',#65784,#35217,#35218);
#28395=AXIS2_PLACEMENT_3D('',#65787,#35220,#35221);
#28396=AXIS2_PLACEMENT_3D('',#65788,#35222,#35223);
#28397=AXIS2_PLACEMENT_3D('',#65791,#35224,#35225);
#28398=AXIS2_PLACEMENT_3D('',#65795,#35227,#35228);
#28399=AXIS2_PLACEMENT_3D('',#65799,#35230,#35231);
#28400=AXIS2_PLACEMENT_3D('',#65803,#35233,#35234);
#28401=AXIS2_PLACEMENT_3D('',#65805,#35236,#35237);
#28402=AXIS2_PLACEMENT_3D('',#65808,#35240,#35241);
#28403=AXIS2_PLACEMENT_3D('',#65810,#35243,#35244);
#28404=AXIS2_PLACEMENT_3D('',#65812,#35246,#35247);
#28405=AXIS2_PLACEMENT_3D('',#65814,#35249,#35250);
#28406=AXIS2_PLACEMENT_3D('',#65816,#35252,#35253);
#28407=AXIS2_PLACEMENT_3D('',#65818,#35255,#35256);
#28408=AXIS2_PLACEMENT_3D('',#65820,#35258,#35259);
#28409=AXIS2_PLACEMENT_3D('',#65821,#35260,#35261);
#28410=AXIS2_PLACEMENT_3D('',#65825,#35263,#35264);
#28411=AXIS2_PLACEMENT_3D('',#65827,#35266,#35267);
#28412=AXIS2_PLACEMENT_3D('',#65831,#35270,#35271);
#28413=AXIS2_PLACEMENT_3D('',#65834,#35273,#35274);
#28414=AXIS2_PLACEMENT_3D('',#65835,#35275,#35276);
#28415=AXIS2_PLACEMENT_3D('',#65841,#35280,#35281);
#28416=AXIS2_PLACEMENT_3D('',#65844,#35283,#35284);
#28417=AXIS2_PLACEMENT_3D('',#65845,#35285,#35286);
#28418=AXIS2_PLACEMENT_3D('',#65848,#35288,#35289);
#28419=AXIS2_PLACEMENT_3D('',#65849,#35290,#35291);
#28420=AXIS2_PLACEMENT_3D('',#65853,#35294,#35295);
#28421=AXIS2_PLACEMENT_3D('',#65856,#35297,#35298);
#28422=AXIS2_PLACEMENT_3D('',#65857,#35299,#35300);
#28423=AXIS2_PLACEMENT_3D('',#65861,#35303,#35304);
#28424=AXIS2_PLACEMENT_3D('',#65862,#35305,#35306);
#28425=AXIS2_PLACEMENT_3D('',#65863,#35307,#35308);
#28426=AXIS2_PLACEMENT_3D('',#65864,#35309,#35310);
#28427=AXIS2_PLACEMENT_3D('',#65865,#35311,#35312);
#28428=AXIS2_PLACEMENT_3D('',#65866,#35313,#35314);
#28429=AXIS2_PLACEMENT_3D('',#65869,#35315,#35316);
#28430=AXIS2_PLACEMENT_3D('',#65873,#35318,#35319);
#28431=AXIS2_PLACEMENT_3D('',#65875,#35320,#35321);
#28432=AXIS2_PLACEMENT_3D('',#65878,#35323,#35324);
#28433=AXIS2_PLACEMENT_3D('',#65879,#35325,#35326);
#28434=AXIS2_PLACEMENT_3D('',#65882,#35329,#35330);
#28435=AXIS2_PLACEMENT_3D('',#65884,#35332,#35333);
#28436=AXIS2_PLACEMENT_3D('',#65886,#35335,#35336);
#28437=AXIS2_PLACEMENT_3D('',#65888,#35338,#35339);
#28438=AXIS2_PLACEMENT_3D('',#65890,#35341,#35342);
#28439=AXIS2_PLACEMENT_3D('',#65891,#35343,#35344);
#28440=AXIS2_PLACEMENT_3D('',#65897,#35348,#35349);
#28441=AXIS2_PLACEMENT_3D('',#65900,#35351,#35352);
#28442=AXIS2_PLACEMENT_3D('',#65901,#35353,#35354);
#28443=AXIS2_PLACEMENT_3D('',#65904,#35356,#35357);
#28444=AXIS2_PLACEMENT_3D('',#65905,#35358,#35359);
#28445=AXIS2_PLACEMENT_3D('',#65909,#35362,#35363);
#28446=AXIS2_PLACEMENT_3D('',#65911,#35364,#35365);
#28447=AXIS2_PLACEMENT_3D('',#65913,#35367,#35368);
#28448=AXIS2_PLACEMENT_3D('',#65914,#35369,#35370);
#28449=AXIS2_PLACEMENT_3D('',#65915,#35371,#35372);
#28450=AXIS2_PLACEMENT_3D('',#65916,#35373,#35374);
#28451=AXIS2_PLACEMENT_3D('',#65920,#35376,#35377);
#28452=AXIS2_PLACEMENT_3D('',#65922,#35379,#35380);
#28453=AXIS2_PLACEMENT_3D('',#65926,#35383,#35384);
#28454=AXIS2_PLACEMENT_3D('',#65929,#35386,#35387);
#28455=AXIS2_PLACEMENT_3D('',#65930,#35388,#35389);
#28456=AXIS2_PLACEMENT_3D('',#65949,#35391,#35392);
#28457=AXIS2_PLACEMENT_3D('',#65953,#35395,#35396);
#28458=AXIS2_PLACEMENT_3D('',#65957,#35398,#35399);
#28459=AXIS2_PLACEMENT_3D('',#65959,#35401,#35402);
#28460=AXIS2_PLACEMENT_3D('',#65963,#35405,#35406);
#28461=AXIS2_PLACEMENT_3D('',#65966,#35408,#35409);
#28462=AXIS2_PLACEMENT_3D('',#65967,#35410,#35411);
#28463=AXIS2_PLACEMENT_3D('',#65971,#35414,#35415);
#28464=AXIS2_PLACEMENT_3D('',#65974,#35417,#35418);
#28465=AXIS2_PLACEMENT_3D('',#65975,#35419,#35420);
#28466=AXIS2_PLACEMENT_3D('',#65977,#35422,#35423);
#28467=AXIS2_PLACEMENT_3D('',#65998,#35425,#35426);
#28468=AXIS2_PLACEMENT_3D('',#66000,#35428,#35429);
#28469=AXIS2_PLACEMENT_3D('',#66001,#35430,#35431);
#28470=AXIS2_PLACEMENT_3D('',#66002,#35432,#35433);
#28471=AXIS2_PLACEMENT_3D('',#66003,#35434,#35435);
#28472=AXIS2_PLACEMENT_3D('',#66004,#35436,#35437);
#28473=AXIS2_PLACEMENT_3D('',#66005,#35438,#35439);
#28474=AXIS2_PLACEMENT_3D('',#66006,#35440,#35441);
#28475=AXIS2_PLACEMENT_3D('',#66007,#35442,#35443);
#28476=AXIS2_PLACEMENT_3D('',#66008,#35444,#35445);
#28477=AXIS2_PLACEMENT_3D('',#66009,#35446,#35447);
#28478=AXIS2_PLACEMENT_3D('',#66010,#35448,#35449);
#28479=AXIS2_PLACEMENT_3D('',#66011,#35450,#35451);
#28480=AXIS2_PLACEMENT_3D('',#66012,#35452,#35453);
#28481=AXIS2_PLACEMENT_3D('',#66014,#35454,#35455);
#28482=AXIS2_PLACEMENT_3D('',#66017,#35457,#35458);
#28483=AXIS2_PLACEMENT_3D('',#66018,#35459,#35460);
#28484=AXIS2_PLACEMENT_3D('',#66021,#35462,#35463);
#28485=AXIS2_PLACEMENT_3D('',#66023,#35464,#35465);
#28486=AXIS2_PLACEMENT_3D('',#66026,#35467,#35468);
#28487=AXIS2_PLACEMENT_3D('',#66027,#35469,#35470);
#28488=AXIS2_PLACEMENT_3D('',#66030,#35472,#35473);
#28489=AXIS2_PLACEMENT_3D('',#66032,#35474,#35475);
#28490=AXIS2_PLACEMENT_3D('',#66035,#35477,#35478);
#28491=AXIS2_PLACEMENT_3D('',#66036,#35479,#35480);
#28492=AXIS2_PLACEMENT_3D('',#66039,#35482,#35483);
#28493=AXIS2_PLACEMENT_3D('',#66041,#35484,#35485);
#28494=AXIS2_PLACEMENT_3D('',#66044,#35487,#35488);
#28495=AXIS2_PLACEMENT_3D('',#66045,#35489,#35490);
#28496=AXIS2_PLACEMENT_3D('',#66048,#35492,#35493);
#28497=AXIS2_PLACEMENT_3D('',#66050,#35494,#35495);
#28498=AXIS2_PLACEMENT_3D('',#66053,#35497,#35498);
#28499=AXIS2_PLACEMENT_3D('',#66054,#35499,#35500);
#28500=AXIS2_PLACEMENT_3D('',#66057,#35502,#35503);
#28501=AXIS2_PLACEMENT_3D('',#66059,#35504,#35505);
#28502=AXIS2_PLACEMENT_3D('',#66062,#35507,#35508);
#28503=AXIS2_PLACEMENT_3D('',#66063,#35509,#35510);
#28504=AXIS2_PLACEMENT_3D('',#66066,#35512,#35513);
#28505=AXIS2_PLACEMENT_3D('',#66068,#35514,#35515);
#28506=AXIS2_PLACEMENT_3D('',#66071,#35517,#35518);
#28507=AXIS2_PLACEMENT_3D('',#66072,#35519,#35520);
#28508=AXIS2_PLACEMENT_3D('',#66075,#35522,#35523);
#28509=AXIS2_PLACEMENT_3D('',#66077,#35524,#35525);
#28510=AXIS2_PLACEMENT_3D('',#66080,#35527,#35528);
#28511=AXIS2_PLACEMENT_3D('',#66081,#35529,#35530);
#28512=AXIS2_PLACEMENT_3D('',#66084,#35532,#35533);
#28513=AXIS2_PLACEMENT_3D('',#66086,#35534,#35535);
#28514=AXIS2_PLACEMENT_3D('',#66089,#35537,#35538);
#28515=AXIS2_PLACEMENT_3D('',#66090,#35539,#35540);
#28516=AXIS2_PLACEMENT_3D('',#66093,#35542,#35543);
#28517=AXIS2_PLACEMENT_3D('',#66095,#35544,#35545);
#28518=AXIS2_PLACEMENT_3D('',#66098,#35547,#35548);
#28519=AXIS2_PLACEMENT_3D('',#66099,#35549,#35550);
#28520=AXIS2_PLACEMENT_3D('',#66102,#35552,#35553);
#28521=AXIS2_PLACEMENT_3D('',#66104,#35554,#35555);
#28522=AXIS2_PLACEMENT_3D('',#66107,#35557,#35558);
#28523=AXIS2_PLACEMENT_3D('',#66108,#35559,#35560);
#28524=AXIS2_PLACEMENT_3D('',#66111,#35562,#35563);
#28525=AXIS2_PLACEMENT_3D('',#66113,#35564,#35565);
#28526=AXIS2_PLACEMENT_3D('',#66116,#35567,#35568);
#28527=AXIS2_PLACEMENT_3D('',#66117,#35569,#35570);
#28528=AXIS2_PLACEMENT_3D('',#66120,#35572,#35573);
#28529=AXIS2_PLACEMENT_3D('',#66122,#35574,#35575);
#28530=AXIS2_PLACEMENT_3D('',#66125,#35577,#35578);
#28531=AXIS2_PLACEMENT_3D('',#66126,#35579,#35580);
#28532=AXIS2_PLACEMENT_3D('',#66129,#35582,#35583);
#28533=AXIS2_PLACEMENT_3D('',#66131,#35584,#35585);
#28534=AXIS2_PLACEMENT_3D('',#66134,#35587,#35588);
#28535=AXIS2_PLACEMENT_3D('',#66135,#35589,#35590);
#28536=AXIS2_PLACEMENT_3D('',#66138,#35592,#35593);
#28537=AXIS2_PLACEMENT_3D('',#66140,#35594,#35595);
#28538=AXIS2_PLACEMENT_3D('',#66143,#35597,#35598);
#28539=AXIS2_PLACEMENT_3D('',#66144,#35599,#35600);
#28540=AXIS2_PLACEMENT_3D('',#66147,#35602,#35603);
#28541=AXIS2_PLACEMENT_3D('',#66149,#35604,#35605);
#28542=AXIS2_PLACEMENT_3D('',#66152,#35607,#35608);
#28543=AXIS2_PLACEMENT_3D('',#66153,#35609,#35610);
#28544=AXIS2_PLACEMENT_3D('',#66156,#35612,#35613);
#28545=AXIS2_PLACEMENT_3D('',#66158,#35614,#35615);
#28546=AXIS2_PLACEMENT_3D('',#66161,#35617,#35618);
#28547=AXIS2_PLACEMENT_3D('',#66162,#35619,#35620);
#28548=AXIS2_PLACEMENT_3D('',#66165,#35622,#35623);
#28549=AXIS2_PLACEMENT_3D('',#66174,#35628,#35629);
#28550=AXIS2_PLACEMENT_3D('',#66178,#35631,#35632);
#28551=AXIS2_PLACEMENT_3D('',#66182,#35634,#35635);
#28552=AXIS2_PLACEMENT_3D('',#66192,#35641,#35642);
#28553=AXIS2_PLACEMENT_3D('',#66198,#35646,#35647);
#28554=AXIS2_PLACEMENT_3D('',#66203,#35649,#35650);
#28555=AXIS2_PLACEMENT_3D('',#66207,#35652,#35653);
#28556=AXIS2_PLACEMENT_3D('',#66213,#35658,#35659);
#28557=AXIS2_PLACEMENT_3D('',#66216,#35662,#35663);
#28558=AXIS2_PLACEMENT_3D('',#66217,#35664,#35665);
#28559=AXIS2_PLACEMENT_3D('',#66218,#35666,#35667);
#28560=AXIS2_PLACEMENT_3D('',#66220,#35669,#35670);
#28561=AXIS2_PLACEMENT_3D('',#66223,#35673,#35674);
#28562=AXIS2_PLACEMENT_3D('',#66225,#35676,#35677);
#28563=AXIS2_PLACEMENT_3D('',#66226,#35678,#35679);
#28564=AXIS2_PLACEMENT_3D('',#66227,#35680,#35681);
#28565=AXIS2_PLACEMENT_3D('',#66228,#35682,#35683);
#28566=AXIS2_PLACEMENT_3D('',#66230,#35684,#35685);
#28567=AXIS2_PLACEMENT_3D('',#66233,#35687,#35688);
#28568=AXIS2_PLACEMENT_3D('',#66234,#35689,#35690);
#28569=AXIS2_PLACEMENT_3D('',#66237,#35692,#35693);
#28570=AXIS2_PLACEMENT_3D('',#66238,#35694,#35695);
#28571=AXIS2_PLACEMENT_3D('',#66241,#35696,#35697);
#28572=AXIS2_PLACEMENT_3D('',#66244,#35699,#35700);
#28573=AXIS2_PLACEMENT_3D('',#66245,#35701,#35702);
#28574=AXIS2_PLACEMENT_3D('',#66246,#35703,#35704);
#28575=AXIS2_PLACEMENT_3D('',#66249,#35706,#35707);
#28576=AXIS2_PLACEMENT_3D('',#66250,#35708,#35709);
#28577=AXIS2_PLACEMENT_3D('',#66251,#35710,#35711);
#28578=AXIS2_PLACEMENT_3D('',#66264,#35718,#35719);
#28579=AXIS2_PLACEMENT_3D('',#66265,#35720,#35721);
#28580=AXIS2_PLACEMENT_3D('',#66271,#35725,#35726);
#28581=AXIS2_PLACEMENT_3D('',#66275,#35729,#35730);
#28582=AXIS2_PLACEMENT_3D('',#66279,#35733,#35734);
#28583=AXIS2_PLACEMENT_3D('',#66283,#35737,#35738);
#28584=AXIS2_PLACEMENT_3D('',#66287,#35741,#35742);
#28585=AXIS2_PLACEMENT_3D('',#66289,#35744,#35745);
#28586=AXIS2_PLACEMENT_3D('',#66290,#35746,#35747);
#28587=AXIS2_PLACEMENT_3D('',#66291,#35748,#35749);
#28588=AXIS2_PLACEMENT_3D('',#66294,#35750,#35751);
#28589=AXIS2_PLACEMENT_3D('',#66295,#35752,#35753);
#28590=AXIS2_PLACEMENT_3D('',#66298,#35755,#35756);
#28591=AXIS2_PLACEMENT_3D('',#66299,#35757,#35758);
#28592=AXIS2_PLACEMENT_3D('',#66304,#35760,#35761);
#28593=AXIS2_PLACEMENT_3D('',#66306,#35762,#35763);
#28594=AXIS2_PLACEMENT_3D('',#66308,#35764,#35765);
#28595=AXIS2_PLACEMENT_3D('',#66310,#35766,#35767);
#28596=AXIS2_PLACEMENT_3D('',#66312,#35768,#35769);
#28597=AXIS2_PLACEMENT_3D('',#66314,#35770,#35771);
#28598=AXIS2_PLACEMENT_3D('',#66315,#35772,#35773);
#28599=AXIS2_PLACEMENT_3D('',#66316,#35774,#35775);
#28600=AXIS2_PLACEMENT_3D('',#66319,#35777,#35778);
#28601=AXIS2_PLACEMENT_3D('',#66320,#35779,#35780);
#28602=AXIS2_PLACEMENT_3D('',#66322,#35781,#35782);
#28603=AXIS2_PLACEMENT_3D('',#66325,#35784,#35785);
#28604=AXIS2_PLACEMENT_3D('',#66326,#35786,#35787);
#28605=AXIS2_PLACEMENT_3D('',#66328,#35788,#35789);
#28606=AXIS2_PLACEMENT_3D('',#66331,#35791,#35792);
#28607=AXIS2_PLACEMENT_3D('',#66332,#35793,#35794);
#28608=AXIS2_PLACEMENT_3D('',#66345,#35801,#35802);
#28609=AXIS2_PLACEMENT_3D('',#66346,#35803,#35804);
#28610=AXIS2_PLACEMENT_3D('',#66347,#35805,#35806);
#28611=AXIS2_PLACEMENT_3D('',#66348,#35807,#35808);
#28612=AXIS2_PLACEMENT_3D('',#66355,#35813,#35814);
#28613=AXIS2_PLACEMENT_3D('',#66360,#35818,#35819);
#28614=AXIS2_PLACEMENT_3D('',#66365,#35823,#35824);
#28615=AXIS2_PLACEMENT_3D('',#66370,#35828,#35829);
#28616=AXIS2_PLACEMENT_3D('',#66375,#35833,#35834);
#28617=AXIS2_PLACEMENT_3D('',#66378,#35837,#35838);
#28618=AXIS2_PLACEMENT_3D('',#66379,#35839,#35840);
#28619=AXIS2_PLACEMENT_3D('',#66380,#35841,#35842);
#28620=AXIS2_PLACEMENT_3D('',#66381,#35843,#35844);
#28621=AXIS2_PLACEMENT_3D('',#66382,#35845,#35846);
#28622=AXIS2_PLACEMENT_3D('',#66383,#35847,#35848);
#28623=AXIS2_PLACEMENT_3D('',#66384,#35849,#35850);
#28624=AXIS2_PLACEMENT_3D('',#66386,#35851,#35852);
#28625=AXIS2_PLACEMENT_3D('',#66389,#35854,#35855);
#28626=AXIS2_PLACEMENT_3D('',#66390,#35856,#35857);
#28627=AXIS2_PLACEMENT_3D('',#66392,#35858,#35859);
#28628=AXIS2_PLACEMENT_3D('',#66395,#35861,#35862);
#28629=AXIS2_PLACEMENT_3D('',#66396,#35863,#35864);
#28630=AXIS2_PLACEMENT_3D('',#66397,#35865,#35866);
#28631=AXIS2_PLACEMENT_3D('',#66398,#35867,#35868);
#28632=AXIS2_PLACEMENT_3D('',#66401,#35869,#35870);
#28633=AXIS2_PLACEMENT_3D('',#66405,#35872,#35873);
#28634=AXIS2_PLACEMENT_3D('',#66407,#35875,#35876);
#28635=AXIS2_PLACEMENT_3D('',#66410,#35877,#35878);
#28636=AXIS2_PLACEMENT_3D('',#66414,#35880,#35881);
#28637=AXIS2_PLACEMENT_3D('',#66416,#35883,#35884);
#28638=AXIS2_PLACEMENT_3D('',#66419,#35887,#35888);
#28639=AXIS2_PLACEMENT_3D('',#66422,#35891,#35892);
#28640=AXIS2_PLACEMENT_3D('',#66423,#35893,#35894);
#28641=AXIS2_PLACEMENT_3D('',#66424,#35895,#35896);
#28642=AXIS2_PLACEMENT_3D('',#66425,#35897,#35898);
#28643=AXIS2_PLACEMENT_3D('',#66427,#35899,#35900);
#28644=AXIS2_PLACEMENT_3D('',#66430,#35902,#35903);
#28645=AXIS2_PLACEMENT_3D('',#66431,#35904,#35905);
#28646=AXIS2_PLACEMENT_3D('',#66433,#35906,#35907);
#28647=AXIS2_PLACEMENT_3D('',#66436,#35909,#35910);
#28648=AXIS2_PLACEMENT_3D('',#66437,#35911,#35912);
#28649=AXIS2_PLACEMENT_3D('',#66439,#35913,#35914);
#28650=AXIS2_PLACEMENT_3D('',#66442,#35916,#35917);
#28651=AXIS2_PLACEMENT_3D('',#66443,#35918,#35919);
#28652=AXIS2_PLACEMENT_3D('',#66445,#35920,#35921);
#28653=AXIS2_PLACEMENT_3D('',#66448,#35923,#35924);
#28654=AXIS2_PLACEMENT_3D('',#66449,#35925,#35926);
#28655=AXIS2_PLACEMENT_3D('',#66451,#35927,#35928);
#28656=AXIS2_PLACEMENT_3D('',#66454,#35930,#35931);
#28657=AXIS2_PLACEMENT_3D('',#66455,#35932,#35933);
#28658=AXIS2_PLACEMENT_3D('',#66457,#35934,#35935);
#28659=AXIS2_PLACEMENT_3D('',#66460,#35937,#35938);
#28660=AXIS2_PLACEMENT_3D('',#66461,#35939,#35940);
#28661=AXIS2_PLACEMENT_3D('',#66463,#35941,#35942);
#28662=AXIS2_PLACEMENT_3D('',#66466,#35944,#35945);
#28663=AXIS2_PLACEMENT_3D('',#66467,#35946,#35947);
#28664=AXIS2_PLACEMENT_3D('',#66469,#35948,#35949);
#28665=AXIS2_PLACEMENT_3D('',#66472,#35951,#35952);
#28666=AXIS2_PLACEMENT_3D('',#66473,#35953,#35954);
#28667=AXIS2_PLACEMENT_3D('',#66475,#35955,#35956);
#28668=AXIS2_PLACEMENT_3D('',#66478,#35958,#35959);
#28669=AXIS2_PLACEMENT_3D('',#66479,#35960,#35961);
#28670=AXIS2_PLACEMENT_3D('',#66481,#35962,#35963);
#28671=AXIS2_PLACEMENT_3D('',#66484,#35965,#35966);
#28672=AXIS2_PLACEMENT_3D('',#66485,#35967,#35968);
#28673=AXIS2_PLACEMENT_3D('',#66494,#35973,#35974);
#28674=AXIS2_PLACEMENT_3D('',#66500,#35978,#35979);
#28675=AXIS2_PLACEMENT_3D('',#66508,#35984,#35985);
#28676=AXIS2_PLACEMENT_3D('',#66514,#35989,#35990);
#28677=AXIS2_PLACEMENT_3D('',#66519,#35994,#35995);
#28678=AXIS2_PLACEMENT_3D('',#66520,#35996,#35997);
#28679=AXIS2_PLACEMENT_3D('',#66522,#35999,#36000);
#28680=AXIS2_PLACEMENT_3D('',#66523,#36001,#36002);
#28681=AXIS2_PLACEMENT_3D('',#66524,#36003,#36004);
#28682=AXIS2_PLACEMENT_3D('',#66526,#36005,#36006);
#28683=AXIS2_PLACEMENT_3D('',#66529,#36008,#36009);
#28684=AXIS2_PLACEMENT_3D('',#66530,#36010,#36011);
#28685=AXIS2_PLACEMENT_3D('',#66533,#36013,#36014);
#28686=AXIS2_PLACEMENT_3D('',#66534,#36015,#36016);
#28687=AXIS2_PLACEMENT_3D('',#66537,#36017,#36018);
#28688=AXIS2_PLACEMENT_3D('',#66540,#36020,#36021);
#28689=AXIS2_PLACEMENT_3D('',#66541,#36022,#36023);
#28690=AXIS2_PLACEMENT_3D('',#66542,#36024,#36025);
#28691=AXIS2_PLACEMENT_3D('',#66545,#36027,#36028);
#28692=AXIS2_PLACEMENT_3D('',#66546,#36029,#36030);
#28693=AXIS2_PLACEMENT_3D('',#66547,#36031,#36032);
#28694=AXIS2_PLACEMENT_3D('',#66560,#36039,#36040);
#28695=AXIS2_PLACEMENT_3D('',#66561,#36041,#36042);
#28696=AXIS2_PLACEMENT_3D('',#66567,#36046,#36047);
#28697=AXIS2_PLACEMENT_3D('',#66571,#36050,#36051);
#28698=AXIS2_PLACEMENT_3D('',#66575,#36054,#36055);
#28699=AXIS2_PLACEMENT_3D('',#66579,#36058,#36059);
#28700=AXIS2_PLACEMENT_3D('',#66583,#36062,#36063);
#28701=AXIS2_PLACEMENT_3D('',#66585,#36065,#36066);
#28702=AXIS2_PLACEMENT_3D('',#66586,#36067,#36068);
#28703=AXIS2_PLACEMENT_3D('',#66587,#36069,#36070);
#28704=AXIS2_PLACEMENT_3D('',#66588,#36071,#36072);
#28705=AXIS2_PLACEMENT_3D('',#66589,#36073,#36074);
#28706=AXIS2_PLACEMENT_3D('',#66590,#36075,#36076);
#28707=AXIS2_PLACEMENT_3D('',#66591,#36077,#36078);
#28708=AXIS2_PLACEMENT_3D('',#66592,#36079,#36080);
#28709=AXIS2_PLACEMENT_3D('',#66593,#36081,#36082);
#28710=AXIS2_PLACEMENT_3D('',#66594,#36083,#36084);
#28711=AXIS2_PLACEMENT_3D('',#66595,#36085,#36086);
#28712=AXIS2_PLACEMENT_3D('',#66596,#36087,#36088);
#28713=AXIS2_PLACEMENT_3D('',#66597,#36089,#36090);
#28714=AXIS2_PLACEMENT_3D('',#66598,#36091,#36092);
#28715=AXIS2_PLACEMENT_3D('',#66599,#36093,#36094);
#28716=AXIS2_PLACEMENT_3D('',#66600,#36095,#36096);
#28717=AXIS2_PLACEMENT_3D('',#66601,#36097,#36098);
#28718=AXIS2_PLACEMENT_3D('',#66602,#36099,#36100);
#28719=AXIS2_PLACEMENT_3D('',#66603,#36101,#36102);
#28720=AXIS2_PLACEMENT_3D('',#66604,#36103,#36104);
#28721=AXIS2_PLACEMENT_3D('',#66605,#36105,#36106);
#28722=AXIS2_PLACEMENT_3D('',#66606,#36107,#36108);
#28723=AXIS2_PLACEMENT_3D('',#66607,#36109,#36110);
#28724=AXIS2_PLACEMENT_3D('',#66608,#36111,#36112);
#28725=AXIS2_PLACEMENT_3D('',#66609,#36113,#36114);
#28726=AXIS2_PLACEMENT_3D('',#66610,#36115,#36116);
#28727=AXIS2_PLACEMENT_3D('',#66611,#36117,#36118);
#28728=AXIS2_PLACEMENT_3D('',#66612,#36119,#36120);
#28729=AXIS2_PLACEMENT_3D('',#66613,#36121,#36122);
#28730=AXIS2_PLACEMENT_3D('',#66614,#36123,#36124);
#28731=AXIS2_PLACEMENT_3D('',#66615,#36125,#36126);
#28732=AXIS2_PLACEMENT_3D('',#66616,#36127,#36128);
#28733=AXIS2_PLACEMENT_3D('',#66617,#36129,#36130);
#28734=AXIS2_PLACEMENT_3D('',#66618,#36131,#36132);
#28735=AXIS2_PLACEMENT_3D('',#66619,#36133,#36134);
#28736=AXIS2_PLACEMENT_3D('',#66620,#36135,#36136);
#28737=AXIS2_PLACEMENT_3D('',#66621,#36137,#36138);
#28738=AXIS2_PLACEMENT_3D('',#66622,#36139,#36140);
#28739=AXIS2_PLACEMENT_3D('',#66623,#36141,#36142);
#28740=AXIS2_PLACEMENT_3D('',#66624,#36143,#36144);
#28741=AXIS2_PLACEMENT_3D('',#66625,#36145,#36146);
#28742=AXIS2_PLACEMENT_3D('',#66626,#36147,#36148);
#28743=AXIS2_PLACEMENT_3D('',#66627,#36149,#36150);
#28744=AXIS2_PLACEMENT_3D('',#66628,#36151,#36152);
#28745=AXIS2_PLACEMENT_3D('',#66629,#36153,#36154);
#28746=AXIS2_PLACEMENT_3D('',#66630,#36155,#36156);
#28747=AXIS2_PLACEMENT_3D('',#66631,#36157,#36158);
#28748=AXIS2_PLACEMENT_3D('',#66632,#36159,#36160);
#28749=AXIS2_PLACEMENT_3D('',#66633,#36161,#36162);
#28750=AXIS2_PLACEMENT_3D('',#66634,#36163,#36164);
#28751=AXIS2_PLACEMENT_3D('',#66635,#36165,#36166);
#28752=AXIS2_PLACEMENT_3D('',#66636,#36167,#36168);
#28753=AXIS2_PLACEMENT_3D('',#66637,#36169,#36170);
#28754=AXIS2_PLACEMENT_3D('',#66638,#36171,#36172);
#28755=AXIS2_PLACEMENT_3D('',#66639,#36173,#36174);
#28756=DIRECTION('axis',(0.,0.,1.));
#28757=DIRECTION('refdir',(1.,0.,0.));
#28758=DIRECTION('axis',(0.,0.,1.));
#28759=DIRECTION('refdir',(1.,0.,0.));
#28760=DIRECTION('center_axis',(0.,0.,1.));
#28761=DIRECTION('ref_axis',(1.,0.,0.));
#28762=DIRECTION('center_axis',(0.,0.,1.));
#28763=DIRECTION('ref_axis',(1.,0.,0.));
#28764=DIRECTION('',(0.,0.,1.));
#28765=DIRECTION('center_axis',(0.,0.,1.));
#28766=DIRECTION('ref_axis',(1.,0.,0.));
#28767=DIRECTION('center_axis',(0.,0.,1.));
#28768=DIRECTION('ref_axis',(1.,0.,0.));
#28769=DIRECTION('center_axis',(0.,0.,1.));
#28770=DIRECTION('ref_axis',(1.,0.,0.));
#28771=DIRECTION('',(0.,0.,1.));
#28772=DIRECTION('center_axis',(0.,0.,1.));
#28773=DIRECTION('ref_axis',(1.,0.,0.));
#28774=DIRECTION('center_axis',(0.,0.,1.));
#28775=DIRECTION('ref_axis',(1.,0.,0.));
#28776=DIRECTION('center_axis',(0.,0.,1.));
#28777=DIRECTION('ref_axis',(1.,0.,0.));
#28778=DIRECTION('',(0.,0.,1.));
#28779=DIRECTION('center_axis',(0.,0.,1.));
#28780=DIRECTION('ref_axis',(1.,0.,0.));
#28781=DIRECTION('center_axis',(0.,0.,1.));
#28782=DIRECTION('ref_axis',(1.,0.,0.));
#28783=DIRECTION('center_axis',(0.,0.,1.));
#28784=DIRECTION('ref_axis',(1.,0.,0.));
#28785=DIRECTION('',(0.,0.,1.));
#28786=DIRECTION('center_axis',(0.,0.,1.));
#28787=DIRECTION('ref_axis',(1.,0.,0.));
#28788=DIRECTION('center_axis',(-1.,0.,0.));
#28789=DIRECTION('ref_axis',(0.,0.,1.));
#28790=DIRECTION('',(0.,1.,0.));
#28791=DIRECTION('',(0.,0.,-1.));
#28792=DIRECTION('',(0.,1.,0.));
#28793=DIRECTION('',(0.,0.,-1.));
#28794=DIRECTION('center_axis',(0.,-1.,0.));
#28795=DIRECTION('ref_axis',(0.,0.,-1.));
#28796=DIRECTION('',(-1.,0.,0.));
#28797=DIRECTION('',(0.,0.,-1.));
#28798=DIRECTION('',(-1.,0.,0.));
#28799=DIRECTION('center_axis',(1.,0.,0.));
#28800=DIRECTION('ref_axis',(0.,0.,-1.));
#28801=DIRECTION('',(0.,-1.,0.));
#28802=DIRECTION('',(0.,0.,-1.));
#28803=DIRECTION('',(0.,-1.,0.));
#28804=DIRECTION('center_axis',(0.,1.,0.));
#28805=DIRECTION('ref_axis',(0.,0.,1.));
#28806=DIRECTION('',(1.,0.,0.));
#28807=DIRECTION('',(1.,0.,0.));
#28808=DIRECTION('center_axis',(0.,0.,-1.));
#28809=DIRECTION('ref_axis',(-1.,0.,0.));
#28810=DIRECTION('',(1.,-3.46944695195361E-16,0.));
#28811=DIRECTION('',(6.93889390390723E-17,-1.,0.));
#28812=DIRECTION('',(-1.,0.,0.));
#28813=DIRECTION('',(-1.38777878078145E-16,1.,0.));
#28814=DIRECTION('',(1.,0.,0.));
#28815=DIRECTION('',(1.38777878078145E-16,-1.,0.));
#28816=DIRECTION('',(-1.,0.,0.));
#28817=DIRECTION('',(-2.77555756156289E-16,1.,0.));
#28818=DIRECTION('center_axis',(0.,0.,-1.));
#28819=DIRECTION('ref_axis',(-1.,0.,0.));
#28820=DIRECTION('',(6.93889390390723E-17,-1.,0.));
#28821=DIRECTION('',(1.,-3.46944695195361E-16,0.));
#28822=DIRECTION('',(-1.38777878078145E-16,1.,0.));
#28823=DIRECTION('',(-1.,0.,0.));
#28824=DIRECTION('',(1.38777878078145E-16,-1.,0.));
#28825=DIRECTION('',(1.,0.,0.));
#28826=DIRECTION('',(-2.77555756156289E-16,1.,0.));
#28827=DIRECTION('',(-1.,0.,0.));
#28828=DIRECTION('center_axis',(-1.,-1.38777878078145E-16,0.));
#28829=DIRECTION('ref_axis',(1.38777878078145E-16,-1.,0.));
#28830=DIRECTION('',(0.,0.,1.));
#28831=DIRECTION('',(0.,0.,1.));
#28832=DIRECTION('center_axis',(0.,1.,0.));
#28833=DIRECTION('ref_axis',(0.,0.,1.));
#28834=DIRECTION('',(0.,0.,1.));
#28835=DIRECTION('center_axis',(1.,2.77555756156289E-16,0.));
#28836=DIRECTION('ref_axis',(-2.77555756156289E-16,1.,0.));
#28837=DIRECTION('',(0.,0.,1.));
#28838=DIRECTION('center_axis',(0.,-1.,0.));
#28839=DIRECTION('ref_axis',(0.,0.,-1.));
#28840=DIRECTION('center_axis',(-1.,-6.93889390390723E-17,0.));
#28841=DIRECTION('ref_axis',(6.93889390390723E-17,-1.,0.));
#28842=DIRECTION('',(0.,0.,1.));
#28843=DIRECTION('',(0.,0.,1.));
#28844=DIRECTION('center_axis',(0.,1.,0.));
#28845=DIRECTION('ref_axis',(0.,0.,1.));
#28846=DIRECTION('',(0.,0.,1.));
#28847=DIRECTION('center_axis',(1.,1.38777878078145E-16,0.));
#28848=DIRECTION('ref_axis',(-1.38777878078145E-16,1.,0.));
#28849=DIRECTION('',(0.,0.,1.));
#28850=DIRECTION('center_axis',(-3.46944695195361E-16,-1.,0.));
#28851=DIRECTION('ref_axis',(1.,-3.46944695195361E-16,0.));
#28852=DIRECTION('axis',(0.,0.,1.));
#28853=DIRECTION('refdir',(1.,0.,0.));
#28854=DIRECTION('axis',(0.,0.,1.));
#28855=DIRECTION('refdir',(1.,0.,0.));
#28856=DIRECTION('center_axis',(0.,0.,1.));
#28857=DIRECTION('ref_axis',(1.,0.,0.));
#28858=DIRECTION('center_axis',(0.,0.,1.));
#28859=DIRECTION('ref_axis',(1.,0.,0.));
#28860=DIRECTION('',(0.,0.,1.));
#28861=DIRECTION('center_axis',(0.,0.,1.));
#28862=DIRECTION('ref_axis',(1.,0.,0.));
#28863=DIRECTION('center_axis',(0.,0.,1.));
#28864=DIRECTION('ref_axis',(1.,0.,0.));
#28865=DIRECTION('center_axis',(0.,0.,1.));
#28866=DIRECTION('ref_axis',(1.,0.,0.));
#28867=DIRECTION('',(0.,0.,1.));
#28868=DIRECTION('center_axis',(0.,0.,1.));
#28869=DIRECTION('ref_axis',(1.,0.,0.));
#28870=DIRECTION('center_axis',(0.,0.,1.));
#28871=DIRECTION('ref_axis',(1.,0.,0.));
#28872=DIRECTION('center_axis',(0.,0.,1.));
#28873=DIRECTION('ref_axis',(1.,0.,0.));
#28874=DIRECTION('',(0.,0.,1.));
#28875=DIRECTION('center_axis',(0.,0.,1.));
#28876=DIRECTION('ref_axis',(1.,0.,0.));
#28877=DIRECTION('center_axis',(0.,0.,1.));
#28878=DIRECTION('ref_axis',(1.,0.,0.));
#28879=DIRECTION('center_axis',(0.,0.,1.));
#28880=DIRECTION('ref_axis',(1.,0.,0.));
#28881=DIRECTION('',(0.,0.,1.));
#28882=DIRECTION('center_axis',(0.,0.,1.));
#28883=DIRECTION('ref_axis',(1.,0.,0.));
#28884=DIRECTION('center_axis',(0.,0.,1.));
#28885=DIRECTION('ref_axis',(1.,0.,0.));
#28886=DIRECTION('',(-5.33761069531325E-16,1.,0.));
#28887=DIRECTION('',(-1.,0.,0.));
#28888=DIRECTION('',(0.,1.,0.));
#28889=DIRECTION('',(-1.,0.,0.));
#28890=DIRECTION('center_axis',(-1.,0.,0.));
#28891=DIRECTION('ref_axis',(0.,0.,1.));
#28892=DIRECTION('',(0.,0.,1.));
#28893=DIRECTION('',(6.93889390390723E-16,1.,0.));
#28894=DIRECTION('',(0.,0.,-1.));
#28895=DIRECTION('',(0.,1.,0.));
#28896=DIRECTION('',(0.,0.,-1.));
#28897=DIRECTION('center_axis',(0.,-1.,0.));
#28898=DIRECTION('ref_axis',(0.,0.,-1.));
#28899=DIRECTION('',(-1.,0.,0.));
#28900=DIRECTION('',(0.,0.,1.));
#28901=DIRECTION('',(-1.,0.,0.));
#28902=DIRECTION('',(0.,0.,-1.));
#28903=DIRECTION('center_axis',(1.,0.,0.));
#28904=DIRECTION('ref_axis',(0.,0.,-1.));
#28905=DIRECTION('',(0.,-1.,0.));
#28906=DIRECTION('',(0.,0.,1.));
#28907=DIRECTION('',(0.,-1.,0.));
#28908=DIRECTION('',(0.,-1.,0.));
#28909=DIRECTION('',(0.,0.,-1.));
#28910=DIRECTION('center_axis',(0.,1.,0.));
#28911=DIRECTION('ref_axis',(0.,0.,1.));
#28912=DIRECTION('',(1.,-8.67361737988404E-17,0.));
#28913=DIRECTION('',(0.,0.,1.));
#28914=DIRECTION('',(1.,0.,0.));
#28915=DIRECTION('',(1.,0.,0.));
#28916=DIRECTION('center_axis',(0.,0.,1.));
#28917=DIRECTION('ref_axis',(1.,0.,0.));
#28918=DIRECTION('',(0.,-1.,0.));
#28919=DIRECTION('',(1.,0.,0.));
#28920=DIRECTION('center_axis',(0.,0.,1.));
#28921=DIRECTION('ref_axis',(1.,0.,0.));
#28922=DIRECTION('center_axis',(1.,5.33761069531325E-16,0.));
#28923=DIRECTION('ref_axis',(-5.33761069531325E-16,1.,0.));
#28924=DIRECTION('',(-5.33761069531325E-16,1.,0.));
#28925=DIRECTION('',(0.,0.,1.));
#28926=DIRECTION('center_axis',(0.,1.,0.));
#28927=DIRECTION('ref_axis',(0.,0.,1.));
#28928=DIRECTION('',(-1.,0.,0.));
#28929=DIRECTION('center_axis',(-1.,0.,0.));
#28930=DIRECTION('ref_axis',(0.,0.,1.));
#28931=DIRECTION('',(0.,-1.,0.));
#28932=DIRECTION('',(0.,0.,1.));
#28933=DIRECTION('center_axis',(0.,-1.,0.));
#28934=DIRECTION('ref_axis',(0.,0.,-1.));
#28935=DIRECTION('',(1.,0.,0.));
#28936=DIRECTION('center_axis',(0.,0.,1.));
#28937=DIRECTION('ref_axis',(1.,0.,0.));
#28938=DIRECTION('axis',(0.,0.,1.));
#28939=DIRECTION('refdir',(1.,0.,0.));
#28940=DIRECTION('center_axis',(0.,0.,1.));
#28941=DIRECTION('ref_axis',(1.,0.,0.));
#28942=DIRECTION('center_axis',(0.,0.,1.));
#28943=DIRECTION('ref_axis',(1.,0.,0.));
#28944=DIRECTION('',(0.,0.,1.));
#28945=DIRECTION('center_axis',(0.,0.,1.));
#28946=DIRECTION('ref_axis',(1.,0.,0.));
#28947=DIRECTION('center_axis',(0.,0.,1.));
#28948=DIRECTION('ref_axis',(1.,0.,0.));
#28949=DIRECTION('center_axis',(0.,0.,1.));
#28950=DIRECTION('ref_axis',(1.,0.,0.));
#28951=DIRECTION('',(0.,0.,1.));
#28952=DIRECTION('center_axis',(0.,0.,1.));
#28953=DIRECTION('ref_axis',(1.,0.,0.));
#28954=DIRECTION('center_axis',(0.,0.,1.));
#28955=DIRECTION('ref_axis',(1.,0.,0.));
#28956=DIRECTION('center_axis',(0.,0.,1.));
#28957=DIRECTION('ref_axis',(1.,0.,0.));
#28958=DIRECTION('',(0.,0.,1.));
#28959=DIRECTION('center_axis',(0.,0.,1.));
#28960=DIRECTION('ref_axis',(1.,0.,0.));
#28961=DIRECTION('center_axis',(0.,0.,1.));
#28962=DIRECTION('ref_axis',(1.,0.,0.));
#28963=DIRECTION('center_axis',(0.,0.,1.));
#28964=DIRECTION('ref_axis',(1.,0.,0.));
#28965=DIRECTION('',(0.,0.,1.));
#28966=DIRECTION('center_axis',(0.,0.,1.));
#28967=DIRECTION('ref_axis',(1.,0.,0.));
#28968=DIRECTION('center_axis',(0.,0.,1.));
#28969=DIRECTION('ref_axis',(1.,0.,0.));
#28970=DIRECTION('center_axis',(0.,0.,1.));
#28971=DIRECTION('ref_axis',(1.,0.,0.));
#28972=DIRECTION('',(0.,0.,1.));
#28973=DIRECTION('center_axis',(0.,0.,1.));
#28974=DIRECTION('ref_axis',(1.,0.,0.));
#28975=DIRECTION('center_axis',(0.,0.,1.));
#28976=DIRECTION('ref_axis',(1.,0.,0.));
#28977=DIRECTION('center_axis',(0.,0.,1.));
#28978=DIRECTION('ref_axis',(1.,0.,0.));
#28979=DIRECTION('',(0.,0.,1.));
#28980=DIRECTION('center_axis',(0.,0.,1.));
#28981=DIRECTION('ref_axis',(1.,0.,0.));
#28982=DIRECTION('center_axis',(0.,0.,1.));
#28983=DIRECTION('ref_axis',(1.,0.,0.));
#28984=DIRECTION('center_axis',(0.,0.,1.));
#28985=DIRECTION('ref_axis',(1.,0.,0.));
#28986=DIRECTION('',(0.,0.,1.));
#28987=DIRECTION('center_axis',(0.,0.,1.));
#28988=DIRECTION('ref_axis',(1.,0.,0.));
#28989=DIRECTION('center_axis',(0.,0.,1.));
#28990=DIRECTION('ref_axis',(1.,0.,0.));
#28991=DIRECTION('center_axis',(0.,0.,1.));
#28992=DIRECTION('ref_axis',(1.,0.,0.));
#28993=DIRECTION('',(0.,0.,1.));
#28994=DIRECTION('center_axis',(0.,0.,1.));
#28995=DIRECTION('ref_axis',(1.,0.,0.));
#28996=DIRECTION('center_axis',(0.,0.,1.));
#28997=DIRECTION('ref_axis',(1.,0.,0.));
#28998=DIRECTION('center_axis',(0.,0.,1.));
#28999=DIRECTION('ref_axis',(1.,0.,0.));
#29000=DIRECTION('',(0.,0.,1.));
#29001=DIRECTION('center_axis',(0.,0.,1.));
#29002=DIRECTION('ref_axis',(1.,0.,0.));
#29003=DIRECTION('center_axis',(0.,0.,1.));
#29004=DIRECTION('ref_axis',(1.,0.,0.));
#29005=DIRECTION('center_axis',(0.,0.,1.));
#29006=DIRECTION('ref_axis',(1.,0.,0.));
#29007=DIRECTION('',(0.,0.,1.));
#29008=DIRECTION('center_axis',(0.,0.,1.));
#29009=DIRECTION('ref_axis',(1.,0.,0.));
#29010=DIRECTION('center_axis',(0.,0.,1.));
#29011=DIRECTION('ref_axis',(1.,0.,0.));
#29012=DIRECTION('center_axis',(0.,0.,1.));
#29013=DIRECTION('ref_axis',(1.,0.,0.));
#29014=DIRECTION('',(0.,0.,1.));
#29015=DIRECTION('center_axis',(0.,0.,1.));
#29016=DIRECTION('ref_axis',(1.,0.,0.));
#29017=DIRECTION('center_axis',(0.,0.,1.));
#29018=DIRECTION('ref_axis',(1.,0.,0.));
#29019=DIRECTION('center_axis',(0.,0.,1.));
#29020=DIRECTION('ref_axis',(1.,0.,0.));
#29021=DIRECTION('',(0.,0.,1.));
#29022=DIRECTION('center_axis',(0.,0.,1.));
#29023=DIRECTION('ref_axis',(1.,0.,0.));
#29024=DIRECTION('center_axis',(0.,0.,-1.));
#29025=DIRECTION('ref_axis',(-1.,0.,0.));
#29026=DIRECTION('',(0.,1.,0.));
#29027=DIRECTION('',(1.,0.,0.));
#29028=DIRECTION('',(0.,-1.,0.));
#29029=DIRECTION('',(-1.,0.,0.));
#29030=DIRECTION('center_axis',(-1.,0.,0.));
#29031=DIRECTION('ref_axis',(0.,0.,1.));
#29032=DIRECTION('',(0.,0.,-1.));
#29033=DIRECTION('',(0.,1.,0.));
#29034=DIRECTION('',(0.,0.,-1.));
#29035=DIRECTION('center_axis',(0.,-1.,0.));
#29036=DIRECTION('ref_axis',(0.,0.,-1.));
#29037=DIRECTION('',(0.,0.,-1.));
#29038=DIRECTION('',(-1.,0.,0.));
#29039=DIRECTION('center_axis',(1.,0.,0.));
#29040=DIRECTION('ref_axis',(0.,0.,-1.));
#29041=DIRECTION('',(0.,0.,-1.));
#29042=DIRECTION('',(0.,-1.,0.));
#29043=DIRECTION('center_axis',(0.,1.,0.));
#29044=DIRECTION('ref_axis',(0.,0.,1.));
#29045=DIRECTION('',(1.,0.,0.));
#29046=DIRECTION('center_axis',(0.,0.,-1.));
#29047=DIRECTION('ref_axis',(-1.,0.,0.));
#29048=DIRECTION('center_axis',(0.,0.,1.));
#29049=DIRECTION('ref_axis',(1.,0.,0.));
#29050=DIRECTION('center_axis',(0.,0.,-1.));
#29051=DIRECTION('ref_axis',(-1.,0.,0.));
#29052=DIRECTION('center_axis',(0.,0.,-1.));
#29053=DIRECTION('ref_axis',(-1.,0.,0.));
#29054=DIRECTION('axis',(0.,0.,1.));
#29055=DIRECTION('refdir',(1.,0.,0.));
#29056=DIRECTION('axis',(0.,0.,1.));
#29057=DIRECTION('refdir',(1.,0.,0.));
#29058=DIRECTION('center_axis',(0.,-1.,0.));
#29059=DIRECTION('ref_axis',(0.,0.,-1.));
#29060=DIRECTION('center_axis',(0.,-1.,0.));
#29061=DIRECTION('ref_axis',(0.,0.,-1.));
#29062=DIRECTION('',(0.,-1.,0.));
#29063=DIRECTION('center_axis',(0.,-1.,0.));
#29064=DIRECTION('ref_axis',(0.,0.,-1.));
#29065=DIRECTION('center_axis',(0.,-1.,0.));
#29066=DIRECTION('ref_axis',(0.,0.,-1.));
#29067=DIRECTION('center_axis',(0.,-1.,0.));
#29068=DIRECTION('ref_axis',(0.,0.,-1.));
#29069=DIRECTION('',(0.,-1.,0.));
#29070=DIRECTION('center_axis',(0.,-1.,0.));
#29071=DIRECTION('ref_axis',(0.,0.,-1.));
#29072=DIRECTION('center_axis',(0.,-1.,0.));
#29073=DIRECTION('ref_axis',(0.,0.,-1.));
#29074=DIRECTION('center_axis',(0.,-1.,0.));
#29075=DIRECTION('ref_axis',(0.,0.,-1.));
#29076=DIRECTION('',(0.,-1.,0.));
#29077=DIRECTION('center_axis',(0.,-1.,0.));
#29078=DIRECTION('ref_axis',(0.,0.,-1.));
#29079=DIRECTION('center_axis',(0.,-1.,0.));
#29080=DIRECTION('ref_axis',(0.,0.,-1.));
#29081=DIRECTION('center_axis',(0.,-1.,0.));
#29082=DIRECTION('ref_axis',(0.,0.,-1.));
#29083=DIRECTION('',(0.,-1.,0.));
#29084=DIRECTION('center_axis',(0.,-1.,0.));
#29085=DIRECTION('ref_axis',(0.,0.,-1.));
#29086=DIRECTION('center_axis',(0.,-1.,0.));
#29087=DIRECTION('ref_axis',(0.,0.,-1.));
#29088=DIRECTION('center_axis',(0.,-1.,0.));
#29089=DIRECTION('ref_axis',(0.,0.,-1.));
#29090=DIRECTION('',(0.,-1.,0.));
#29091=DIRECTION('center_axis',(0.,-1.,0.));
#29092=DIRECTION('ref_axis',(0.,0.,-1.));
#29093=DIRECTION('center_axis',(0.,-1.,0.));
#29094=DIRECTION('ref_axis',(0.,0.,-1.));
#29095=DIRECTION('center_axis',(0.,-1.,0.));
#29096=DIRECTION('ref_axis',(0.,0.,-1.));
#29097=DIRECTION('',(0.,-1.,0.));
#29098=DIRECTION('center_axis',(0.,-1.,0.));
#29099=DIRECTION('ref_axis',(0.,0.,-1.));
#29100=DIRECTION('center_axis',(0.,-1.,0.));
#29101=DIRECTION('ref_axis',(0.,0.,-1.));
#29102=DIRECTION('center_axis',(0.,-1.,0.));
#29103=DIRECTION('ref_axis',(0.,0.,-1.));
#29104=DIRECTION('',(0.,-1.,0.));
#29105=DIRECTION('center_axis',(0.,-1.,0.));
#29106=DIRECTION('ref_axis',(0.,0.,-1.));
#29107=DIRECTION('center_axis',(0.,1.,0.));
#29108=DIRECTION('ref_axis',(0.,0.,1.));
#29109=DIRECTION('',(0.,0.,-1.));
#29110=DIRECTION('center_axis',(0.,-1.,0.));
#29111=DIRECTION('ref_axis',(0.,0.,1.));
#29112=DIRECTION('',(1.,0.,0.));
#29113=DIRECTION('',(0.,0.,-1.));
#29114=DIRECTION('',(1.,0.,0.));
#29115=DIRECTION('center_axis',(0.,-1.,0.));
#29116=DIRECTION('ref_axis',(0.,0.,1.));
#29117=DIRECTION('center_axis',(-1.,0.,0.));
#29118=DIRECTION('ref_axis',(0.,0.,1.));
#29119=DIRECTION('',(0.,0.,-1.));
#29120=DIRECTION('',(0.,-1.,0.));
#29121=DIRECTION('',(0.,1.,0.));
#29122=DIRECTION('center_axis',(0.,-1.,0.));
#29123=DIRECTION('ref_axis',(0.,0.,-1.));
#29124=DIRECTION('',(-1.,0.,0.));
#29125=DIRECTION('center_axis',(0.,1.,0.));
#29126=DIRECTION('ref_axis',(0.,0.,-1.));
#29127=DIRECTION('center_axis',(0.,1.,0.));
#29128=DIRECTION('ref_axis',(0.,0.,-1.));
#29129=DIRECTION('',(-1.,0.,0.));
#29130=DIRECTION('',(0.,0.,-1.));
#29131=DIRECTION('center_axis',(1.,0.,0.));
#29132=DIRECTION('ref_axis',(0.,0.,-1.));
#29133=DIRECTION('',(0.,-1.,0.));
#29134=DIRECTION('',(0.,-1.,0.));
#29135=DIRECTION('center_axis',(0.,0.,-1.));
#29136=DIRECTION('ref_axis',(-1.,0.,0.));
#29137=DIRECTION('',(0.,1.,0.));
#29138=DIRECTION('center_axis',(0.,0.,-1.));
#29139=DIRECTION('ref_axis',(-1.,0.,0.));
#29140=DIRECTION('',(0.,-1.,0.));
#29141=DIRECTION('center_axis',(0.,1.,0.));
#29142=DIRECTION('ref_axis',(0.,0.,1.));
#29143=DIRECTION('center_axis',(0.,-1.,0.));
#29144=DIRECTION('ref_axis',(0.,0.,-1.));
#29145=DIRECTION('axis',(0.,0.,1.));
#29146=DIRECTION('refdir',(1.,0.,0.));
#29147=DIRECTION('center_axis',(0.,0.,1.));
#29148=DIRECTION('ref_axis',(1.,0.,0.));
#29149=DIRECTION('center_axis',(0.,0.,1.));
#29150=DIRECTION('ref_axis',(1.,0.,0.));
#29151=DIRECTION('',(0.,0.,1.));
#29152=DIRECTION('center_axis',(0.,0.,1.));
#29153=DIRECTION('ref_axis',(1.,0.,0.));
#29154=DIRECTION('center_axis',(0.,0.,1.));
#29155=DIRECTION('ref_axis',(1.,0.,0.));
#29156=DIRECTION('center_axis',(0.,0.,1.));
#29157=DIRECTION('ref_axis',(1.,0.,0.));
#29158=DIRECTION('',(0.,0.,1.));
#29159=DIRECTION('center_axis',(0.,0.,1.));
#29160=DIRECTION('ref_axis',(1.,0.,0.));
#29161=DIRECTION('center_axis',(0.,0.,1.));
#29162=DIRECTION('ref_axis',(1.,0.,0.));
#29163=DIRECTION('center_axis',(0.,0.,1.));
#29164=DIRECTION('ref_axis',(1.,0.,0.));
#29165=DIRECTION('',(0.,0.,1.));
#29166=DIRECTION('center_axis',(0.,0.,1.));
#29167=DIRECTION('ref_axis',(1.,0.,0.));
#29168=DIRECTION('center_axis',(0.,0.,1.));
#29169=DIRECTION('ref_axis',(1.,0.,0.));
#29170=DIRECTION('center_axis',(0.,0.,1.));
#29171=DIRECTION('ref_axis',(1.,0.,0.));
#29172=DIRECTION('',(0.,0.,1.));
#29173=DIRECTION('center_axis',(0.,0.,1.));
#29174=DIRECTION('ref_axis',(1.,0.,0.));
#29175=DIRECTION('center_axis',(0.,0.,1.));
#29176=DIRECTION('ref_axis',(1.,0.,0.));
#29177=DIRECTION('center_axis',(0.,0.,1.));
#29178=DIRECTION('ref_axis',(1.,0.,0.));
#29179=DIRECTION('',(0.,0.,1.));
#29180=DIRECTION('center_axis',(0.,0.,1.));
#29181=DIRECTION('ref_axis',(1.,0.,0.));
#29182=DIRECTION('center_axis',(0.,0.,1.));
#29183=DIRECTION('ref_axis',(1.,0.,0.));
#29184=DIRECTION('center_axis',(0.,0.,1.));
#29185=DIRECTION('ref_axis',(1.,0.,0.));
#29186=DIRECTION('',(0.,0.,1.));
#29187=DIRECTION('center_axis',(0.,0.,1.));
#29188=DIRECTION('ref_axis',(1.,0.,0.));
#29189=DIRECTION('center_axis',(-1.,-1.46081976924363E-16,0.));
#29190=DIRECTION('ref_axis',(1.46081976924363E-16,-1.,0.));
#29191=DIRECTION('',(-1.46081976924363E-16,1.,0.));
#29192=DIRECTION('',(0.,0.,-1.));
#29193=DIRECTION('',(-1.46081976924363E-16,1.,0.));
#29194=DIRECTION('',(0.,0.,-1.));
#29195=DIRECTION('center_axis',(0.,-1.,0.));
#29196=DIRECTION('ref_axis',(0.,0.,-1.));
#29197=DIRECTION('',(-1.,0.,0.));
#29198=DIRECTION('',(0.,0.,-1.));
#29199=DIRECTION('',(-1.,0.,0.));
#29200=DIRECTION('center_axis',(1.,1.46081976924363E-16,0.));
#29201=DIRECTION('ref_axis',(-1.46081976924363E-16,1.,0.));
#29202=DIRECTION('',(1.46081976924363E-16,-1.,0.));
#29203=DIRECTION('',(0.,0.,-1.));
#29204=DIRECTION('',(1.46081976924363E-16,-1.,0.));
#29205=DIRECTION('center_axis',(0.,1.,0.));
#29206=DIRECTION('ref_axis',(0.,0.,1.));
#29207=DIRECTION('',(1.,0.,0.));
#29208=DIRECTION('',(1.,0.,0.));
#29209=DIRECTION('center_axis',(0.,0.,1.));
#29210=DIRECTION('ref_axis',(1.,0.,0.));
#29211=DIRECTION('center_axis',(0.,0.,1.));
#29212=DIRECTION('ref_axis',(1.,0.,0.));
#29213=DIRECTION('',(-6.16297582203385E-33,4.59047288926841E-32,1.));
#29214=DIRECTION('',(1.,-4.93038065763132E-32,6.16297582203385E-33));
#29215=DIRECTION('',(-1.,1.22464679914694E-16,9.47091042991064E-17));
#29216=DIRECTION('',(9.47091042991064E-17,-1.22464679914778E-16,1.));
#29217=DIRECTION('axis',(0.,0.,1.));
#29218=DIRECTION('refdir',(1.,0.,0.));
#29219=DIRECTION('center_axis',(0.,0.,1.));
#29220=DIRECTION('ref_axis',(1.,0.,0.));
#29221=DIRECTION('center_axis',(0.,0.,1.));
#29222=DIRECTION('ref_axis',(1.,0.,0.));
#29223=DIRECTION('',(0.,0.,1.));
#29224=DIRECTION('center_axis',(0.,0.,1.));
#29225=DIRECTION('ref_axis',(1.,0.,0.));
#29226=DIRECTION('center_axis',(0.,0.,1.));
#29227=DIRECTION('ref_axis',(1.,0.,0.));
#29228=DIRECTION('center_axis',(0.,0.,1.));
#29229=DIRECTION('ref_axis',(1.,0.,0.));
#29230=DIRECTION('',(0.,0.,1.));
#29231=DIRECTION('center_axis',(0.,0.,1.));
#29232=DIRECTION('ref_axis',(1.,0.,0.));
#29233=DIRECTION('center_axis',(0.,0.,1.));
#29234=DIRECTION('ref_axis',(1.,0.,0.));
#29235=DIRECTION('center_axis',(0.,0.,1.));
#29236=DIRECTION('ref_axis',(1.,0.,0.));
#29237=DIRECTION('',(0.,0.,1.));
#29238=DIRECTION('center_axis',(0.,0.,1.));
#29239=DIRECTION('ref_axis',(1.,0.,0.));
#29240=DIRECTION('center_axis',(0.,0.,1.));
#29241=DIRECTION('ref_axis',(1.,0.,0.));
#29242=DIRECTION('center_axis',(0.,0.,1.));
#29243=DIRECTION('ref_axis',(1.,0.,0.));
#29244=DIRECTION('',(0.,0.,1.));
#29245=DIRECTION('center_axis',(0.,0.,1.));
#29246=DIRECTION('ref_axis',(1.,0.,0.));
#29247=DIRECTION('center_axis',(0.,0.,1.));
#29248=DIRECTION('ref_axis',(1.,0.,0.));
#29249=DIRECTION('center_axis',(0.,0.,1.));
#29250=DIRECTION('ref_axis',(1.,0.,0.));
#29251=DIRECTION('',(0.,0.,1.));
#29252=DIRECTION('center_axis',(0.,0.,1.));
#29253=DIRECTION('ref_axis',(1.,0.,0.));
#29254=DIRECTION('center_axis',(0.,0.,1.));
#29255=DIRECTION('ref_axis',(1.,0.,0.));
#29256=DIRECTION('center_axis',(0.,0.,1.));
#29257=DIRECTION('ref_axis',(1.,0.,0.));
#29258=DIRECTION('',(0.,0.,1.));
#29259=DIRECTION('center_axis',(0.,0.,1.));
#29260=DIRECTION('ref_axis',(1.,0.,0.));
#29261=DIRECTION('center_axis',(-1.,1.26161707343768E-16,0.));
#29262=DIRECTION('ref_axis',(-1.26161707343768E-16,-1.,0.));
#29263=DIRECTION('',(1.26161707343768E-16,1.,0.));
#29264=DIRECTION('',(0.,0.,-1.));
#29265=DIRECTION('',(1.26161707343768E-16,1.,0.));
#29266=DIRECTION('',(0.,0.,-1.));
#29267=DIRECTION('center_axis',(0.,-1.,0.));
#29268=DIRECTION('ref_axis',(0.,0.,-1.));
#29269=DIRECTION('',(-1.,0.,0.));
#29270=DIRECTION('',(0.,0.,-1.));
#29271=DIRECTION('',(-1.,0.,0.));
#29272=DIRECTION('center_axis',(1.,0.,0.));
#29273=DIRECTION('ref_axis',(0.,0.,-1.));
#29274=DIRECTION('',(0.,-1.,0.));
#29275=DIRECTION('',(0.,0.,-1.));
#29276=DIRECTION('',(0.,-1.,0.));
#29277=DIRECTION('center_axis',(0.,1.,0.));
#29278=DIRECTION('ref_axis',(0.,0.,1.));
#29279=DIRECTION('',(1.,0.,0.));
#29280=DIRECTION('',(1.,0.,0.));
#29281=DIRECTION('center_axis',(0.,0.,1.));
#29282=DIRECTION('ref_axis',(1.,0.,0.));
#29283=DIRECTION('center_axis',(0.,0.,1.));
#29284=DIRECTION('ref_axis',(1.,0.,0.));
#29285=DIRECTION('axis',(0.,0.,1.));
#29286=DIRECTION('refdir',(1.,0.,0.));
#29287=DIRECTION('axis',(0.,0.,1.));
#29288=DIRECTION('refdir',(1.,0.,0.));
#29289=DIRECTION('center_axis',(0.,1.,0.));
#29290=DIRECTION('ref_axis',(0.,0.,1.));
#29291=DIRECTION('center_axis',(0.,1.,0.));
#29292=DIRECTION('ref_axis',(0.,0.,1.));
#29293=DIRECTION('',(0.,1.,0.));
#29294=DIRECTION('center_axis',(0.,1.,0.));
#29295=DIRECTION('ref_axis',(0.,0.,1.));
#29296=DIRECTION('center_axis',(0.,1.,0.));
#29297=DIRECTION('ref_axis',(0.,0.,1.));
#29298=DIRECTION('center_axis',(6.19544098563146E-17,1.,0.));
#29299=DIRECTION('ref_axis',(-1.,6.19544098563146E-17,0.));
#29300=DIRECTION('center_axis',(-0.707106781186749,0.707106781186346,6.63628373648637E-13));
#29301=DIRECTION('ref_axis',(0.707106781186346,0.707106781186749,2.23245825814312E-8));
#29302=DIRECTION('center_axis',(0.,1.,0.));
#29303=DIRECTION('ref_axis',(0.,0.,1.));
#29304=DIRECTION('center_axis',(-0.707106781186739,0.707106781186356,-6.35085217767548E-13));
#29305=DIRECTION('ref_axis',(0.707106781186356,0.707106781186739,4.00793704510469E-8));
#29306=DIRECTION('center_axis',(6.19544098563146E-17,1.,0.));
#29307=DIRECTION('ref_axis',(-1.,6.19544098563146E-17,0.));
#29308=DIRECTION('',(0.,1.,0.));
#29309=DIRECTION('center_axis',(0.,1.,0.));
#29310=DIRECTION('ref_axis',(0.,0.,1.));
#29311=DIRECTION('center_axis',(6.19544098563146E-17,1.,0.));
#29312=DIRECTION('ref_axis',(-1.,6.19544098563146E-17,0.));
#29313=DIRECTION('center_axis',(0.707106781186538,0.707106781186557,3.68682429798511E-14));
#29314=DIRECTION('ref_axis',(0.707106781186557,-0.707106781186538,1.32375375864267E-10));
#29315=DIRECTION('center_axis',(0.,1.,0.));
#29316=DIRECTION('ref_axis',(0.,0.,1.));
#29317=DIRECTION('center_axis',(0.707106781186323,0.707106781186772,-7.32607666957653E-13));
#29318=DIRECTION('ref_axis',(0.707106781186772,-0.707106781186323,-6.06018510665849E-9));
#29319=DIRECTION('center_axis',(0.,1.,0.));
#29320=DIRECTION('ref_axis',(0.,0.,1.));
#29321=DIRECTION('center_axis',(0.,1.,0.));
#29322=DIRECTION('ref_axis',(0.,0.,1.));
#29323=DIRECTION('',(0.,1.,0.));
#29324=DIRECTION('center_axis',(0.,1.,0.));
#29325=DIRECTION('ref_axis',(0.,0.,1.));
#29326=DIRECTION('center_axis',(0.,1.,0.));
#29327=DIRECTION('ref_axis',(0.,0.,1.));
#29328=DIRECTION('center_axis',(6.19544098563146E-17,1.,0.));
#29329=DIRECTION('ref_axis',(-1.,6.19544098563146E-17,0.));
#29330=DIRECTION('center_axis',(-0.707106781186744,0.707106781186351,6.50546093878307E-13));
#29331=DIRECTION('ref_axis',(0.707106781186351,0.707106781186744,7.42984904174717E-10));
#29332=DIRECTION('center_axis',(0.,1.,0.));
#29333=DIRECTION('ref_axis',(0.,0.,1.));
#29334=DIRECTION('center_axis',(-0.707106781186742,0.707106781186353,-6.42221006739863E-13));
#29335=DIRECTION('ref_axis',(0.707106781186353,0.707106781186742,2.97716291710107E-8));
#29336=DIRECTION('center_axis',(6.19544098563146E-17,1.,0.));
#29337=DIRECTION('ref_axis',(-1.,6.19544098563146E-17,0.));
#29338=DIRECTION('',(0.,1.,0.));
#29339=DIRECTION('center_axis',(0.,1.,0.));
#29340=DIRECTION('ref_axis',(0.,0.,1.));
#29341=DIRECTION('center_axis',(6.19544098563146E-17,1.,0.));
#29342=DIRECTION('ref_axis',(-1.,6.19544098563146E-17,0.));
#29343=DIRECTION('center_axis',(0.707106781186537,0.707106781186558,3.56789448193693E-14));
#29344=DIRECTION('ref_axis',(0.707106781186557,-0.707106781186537,-9.53308819765748E-9));
#29345=DIRECTION('center_axis',(0.,1.,0.));
#29346=DIRECTION('ref_axis',(0.,0.,1.));
#29347=DIRECTION('center_axis',(0.707106781186315,0.70710678118678,-7.56393630180537E-13));
#29348=DIRECTION('ref_axis',(0.70710678118678,-0.707106781186315,-2.44027645301359E-8));
#29349=DIRECTION('center_axis',(0.,1.,0.));
#29350=DIRECTION('ref_axis',(0.,0.,1.));
#29351=DIRECTION('center_axis',(0.,1.,0.));
#29352=DIRECTION('ref_axis',(0.,0.,1.));
#29353=DIRECTION('',(0.,1.,0.));
#29354=DIRECTION('center_axis',(0.,1.,0.));
#29355=DIRECTION('ref_axis',(0.,0.,1.));
#29356=DIRECTION('center_axis',(0.,1.,0.));
#29357=DIRECTION('ref_axis',(0.,0.,1.));
#29358=DIRECTION('center_axis',(6.19544098563146E-17,1.,0.));
#29359=DIRECTION('ref_axis',(-1.,6.19544098563146E-17,0.));
#29360=DIRECTION('center_axis',(-0.707106781186747,0.707106781186348,6.58871181003077E-13));
#29361=DIRECTION('ref_axis',(0.707106781186348,0.707106781186747,1.69840014417738E-8));
#29362=DIRECTION('center_axis',(0.,1.,0.));
#29363=DIRECTION('ref_axis',(0.,0.,1.));
#29364=DIRECTION('center_axis',(-0.707106781186741,0.707106781186354,-6.42221006748515E-13));
#29365=DIRECTION('ref_axis',(0.707106781186354,0.707106781186741,1.98080202652188E-8));
#29366=DIRECTION('center_axis',(6.19544098563146E-17,1.,0.));
#29367=DIRECTION('ref_axis',(-1.,6.19544098563146E-17,0.));
#29368=DIRECTION('',(0.,1.,0.));
#29369=DIRECTION('center_axis',(0.,1.,0.));
#29370=DIRECTION('ref_axis',(0.,0.,1.));
#29371=DIRECTION('center_axis',(6.19544098563146E-17,1.,0.));
#29372=DIRECTION('ref_axis',(-1.,6.19544098563146E-17,0.));
#29373=DIRECTION('center_axis',(0.707106781186533,0.707106781186562,4.51933301047554E-14));
#29374=DIRECTION('ref_axis',(0.707106781186562,-0.707106781186533,-3.30550302651237E-9));
#29375=DIRECTION('center_axis',(0.,1.,0.));
#29376=DIRECTION('ref_axis',(0.,0.,1.));
#29377=DIRECTION('center_axis',(0.707106781186314,0.707106781186781,-7.5639363017397E-13));
#29378=DIRECTION('ref_axis',(0.707106781186781,-0.707106781186314,-1.22471854963268E-8));
#29379=DIRECTION('center_axis',(0.,1.,0.));
#29380=DIRECTION('ref_axis',(0.,0.,1.));
#29381=DIRECTION('center_axis',(0.,1.,0.));
#29382=DIRECTION('ref_axis',(0.,0.,1.));
#29383=DIRECTION('',(0.,1.,0.));
#29384=DIRECTION('center_axis',(0.,1.,0.));
#29385=DIRECTION('ref_axis',(0.,0.,1.));
#29386=DIRECTION('center_axis',(0.,1.,0.));
#29387=DIRECTION('ref_axis',(0.,0.,1.));
#29388=DIRECTION('center_axis',(6.19544098563146E-17,1.,0.));
#29389=DIRECTION('ref_axis',(-1.,6.19544098563146E-17,0.));
#29390=DIRECTION('center_axis',(-0.707106781186749,0.707106781186347,6.60060479163914E-13));
#29391=DIRECTION('ref_axis',(0.707106781186346,0.707106781186748,2.47609223171707E-8));
#29392=DIRECTION('center_axis',(0.,1.,0.));
#29393=DIRECTION('ref_axis',(0.,0.,1.));
#29394=DIRECTION('center_axis',(-0.707106781186743,0.707106781186353,-6.44599603075256E-13));
#29395=DIRECTION('ref_axis',(0.707106781186353,0.707106781186743,7.64517967052409E-9));
#29396=DIRECTION('center_axis',(6.19544098563146E-17,1.,0.));
#29397=DIRECTION('ref_axis',(-1.,6.19544098563146E-17,0.));
#29398=DIRECTION('',(0.,1.,0.));
#29399=DIRECTION('center_axis',(0.,1.,0.));
#29400=DIRECTION('ref_axis',(0.,0.,1.));
#29401=DIRECTION('center_axis',(6.19544098563146E-17,1.,0.));
#29402=DIRECTION('ref_axis',(-1.,6.19544098563146E-17,0.));
#29403=DIRECTION('center_axis',(0.707106781186532,0.707106781186563,5.11398209079768E-14));
#29404=DIRECTION('ref_axis',(0.707106781186563,-0.707106781186532,-3.95517993196584E-9));
#29405=DIRECTION('center_axis',(0.,1.,0.));
#29406=DIRECTION('ref_axis',(0.,0.,1.));
#29407=DIRECTION('center_axis',(0.707106781186319,0.707106781186776,-7.42122052246304E-13));
#29408=DIRECTION('ref_axis',(0.707106781186776,-0.707106781186319,-4.45259227831794E-9));
#29409=DIRECTION('center_axis',(0.,1.,0.));
#29410=DIRECTION('ref_axis',(0.,0.,1.));
#29411=DIRECTION('center_axis',(0.,1.,0.));
#29412=DIRECTION('ref_axis',(0.,0.,1.));
#29413=DIRECTION('',(0.,1.,0.));
#29414=DIRECTION('center_axis',(0.,1.,0.));
#29415=DIRECTION('ref_axis',(0.,0.,1.));
#29416=DIRECTION('center_axis',(0.,1.,0.));
#29417=DIRECTION('ref_axis',(0.,0.,1.));
#29418=DIRECTION('center_axis',(6.19544098563146E-17,1.,0.));
#29419=DIRECTION('ref_axis',(-1.,6.19544098563146E-17,0.));
#29420=DIRECTION('center_axis',(-0.707106781186743,0.707106781186353,6.43410304908884E-13));
#29421=DIRECTION('ref_axis',(0.707106781186353,0.707106781186743,-5.80498325499735E-9));
#29422=DIRECTION('center_axis',(0.,1.,0.));
#29423=DIRECTION('ref_axis',(0.,0.,1.));
#29424=DIRECTION('center_axis',(-0.707106781186738,0.707106781186357,-6.32706621460411E-13));
#29425=DIRECTION('ref_axis',(0.707106781186357,0.707106781186739,7.95059306801949E-9));
#29426=DIRECTION('center_axis',(6.19544098563146E-17,1.,0.));
#29427=DIRECTION('ref_axis',(-1.,6.19544098563146E-17,0.));
#29428=DIRECTION('',(0.,1.,0.));
#29429=DIRECTION('center_axis',(0.,1.,0.));
#29430=DIRECTION('ref_axis',(0.,0.,1.));
#29431=DIRECTION('center_axis',(6.19544098563146E-17,1.,0.));
#29432=DIRECTION('ref_axis',(-1.,6.19544098563146E-17,0.));
#29433=DIRECTION('center_axis',(0.70710678118653,0.707106781186565,5.70863117107439E-14));
#29434=DIRECTION('ref_axis',(0.707106781186565,-0.70710678118653,-9.09071113315049E-9));
#29435=DIRECTION('center_axis',(0.,1.,0.));
#29436=DIRECTION('ref_axis',(0.,0.,1.));
#29437=DIRECTION('center_axis',(0.707106781186317,0.707106781186778,-7.46879244888732E-13));
#29438=DIRECTION('ref_axis',(0.707106781186778,-0.707106781186317,-1.00256530335873E-9));
#29439=DIRECTION('center_axis',(0.,1.,0.));
#29440=DIRECTION('ref_axis',(0.,0.,1.));
#29441=DIRECTION('center_axis',(0.,1.,0.));
#29442=DIRECTION('ref_axis',(0.,0.,1.));
#29443=DIRECTION('',(0.,1.,0.));
#29444=DIRECTION('center_axis',(0.,1.,0.));
#29445=DIRECTION('ref_axis',(0.,0.,1.));
#29446=DIRECTION('center_axis',(0.,1.,0.));
#29447=DIRECTION('ref_axis',(0.,0.,1.));
#29448=DIRECTION('center_axis',(6.19544098563146E-17,1.,0.));
#29449=DIRECTION('ref_axis',(-1.,6.19544098563146E-17,0.));
#29450=DIRECTION('center_axis',(-0.707106781186744,0.707106781186351,6.48167497551415E-13));
#29451=DIRECTION('ref_axis',(0.707106781186351,0.707106781186744,-6.09200717301252E-9));
#29452=DIRECTION('center_axis',(0.,1.,0.));
#29453=DIRECTION('ref_axis',(0.,0.,1.));
#29454=DIRECTION('center_axis',(-0.707106781186739,0.707106781186356,-6.35085217784288E-13));
#29455=DIRECTION('ref_axis',(0.707106781186356,0.707106781186739,2.19719109990964E-8));
#29456=DIRECTION('center_axis',(6.19544098563146E-17,1.,0.));
#29457=DIRECTION('ref_axis',(-1.,6.19544098563146E-17,0.));
#29458=DIRECTION('',(0.,1.,0.));
#29459=DIRECTION('center_axis',(0.,1.,0.));
#29460=DIRECTION('ref_axis',(0.,0.,1.));
#29461=DIRECTION('center_axis',(6.19544098563146E-17,1.,0.));
#29462=DIRECTION('ref_axis',(-1.,6.19544098563146E-17,0.));
#29463=DIRECTION('center_axis',(0.707106781186531,0.707106781186564,5.35184172289345E-14));
#29464=DIRECTION('ref_axis',(0.707106781186564,-0.707106781186531,-2.37666658604641E-9));
#29465=DIRECTION('center_axis',(0.,1.,0.));
#29466=DIRECTION('ref_axis',(0.,0.,1.));
#29467=DIRECTION('center_axis',(0.707106781186313,0.707106781186782,-7.61150822819952E-13));
#29468=DIRECTION('ref_axis',(0.707106781186782,-0.707106781186313,-1.44200498676106E-8));
#29469=DIRECTION('center_axis',(0.,1.,0.));
#29470=DIRECTION('ref_axis',(0.,0.,1.));
#29471=DIRECTION('center_axis',(0.,1.,0.));
#29472=DIRECTION('ref_axis',(0.,0.,1.));
#29473=DIRECTION('',(0.,1.,0.));
#29474=DIRECTION('center_axis',(0.,1.,0.));
#29475=DIRECTION('ref_axis',(0.,0.,1.));
#29476=DIRECTION('center_axis',(0.,1.,0.));
#29477=DIRECTION('ref_axis',(0.,0.,1.));
#29478=DIRECTION('center_axis',(6.19544098563146E-17,1.,0.));
#29479=DIRECTION('ref_axis',(-1.,6.19544098563146E-17,0.));
#29480=DIRECTION('center_axis',(-0.707106781186525,0.70710678118657,-6.42221006747096E-14));
#29481=DIRECTION('ref_axis',(0.70710678118657,0.707106781186525,-6.27115230759585E-9));
#29482=DIRECTION('center_axis',(0.,1.,0.));
#29483=DIRECTION('ref_axis',(0.,0.,1.));
#29484=DIRECTION('center_axis',(-0.707106781186519,0.707106781186576,7.84936786023992E-14));
#29485=DIRECTION('ref_axis',(0.707106781186576,0.707106781186519,-6.37187636878396E-9));
#29486=DIRECTION('center_axis',(6.19544098563146E-17,1.,0.));
#29487=DIRECTION('ref_axis',(-1.,6.19544098563146E-17,0.));
#29488=DIRECTION('',(0.,1.,0.));
#29489=DIRECTION('center_axis',(0.,1.,0.));
#29490=DIRECTION('ref_axis',(0.,0.,1.));
#29491=DIRECTION('center_axis',(6.19544098563146E-17,1.,0.));
#29492=DIRECTION('ref_axis',(-1.,6.19544098563146E-17,0.));
#29493=DIRECTION('center_axis',(0.707106781186529,0.707106781186566,5.82756098715003E-14));
#29494=DIRECTION('ref_axis',(0.707106781186566,-0.707106781186529,-1.41665956895109E-8));
#29495=DIRECTION('center_axis',(0.,1.,0.));
#29496=DIRECTION('ref_axis',(0.,0.,1.));
#29497=DIRECTION('center_axis',(0.707106781186545,0.707106781186551,-1.18929816065332E-14));
#29498=DIRECTION('ref_axis',(0.707106781186551,-0.707106781186544,8.15266177051329E-10));
#29499=DIRECTION('center_axis',(0.,1.,0.));
#29500=DIRECTION('ref_axis',(0.,0.,1.));
#29501=DIRECTION('center_axis',(0.,1.,0.));
#29502=DIRECTION('ref_axis',(0.,0.,1.));
#29503=DIRECTION('',(0.,1.,0.));
#29504=DIRECTION('center_axis',(0.,1.,0.));
#29505=DIRECTION('ref_axis',(0.,0.,1.));
#29506=DIRECTION('center_axis',(0.,1.,0.));
#29507=DIRECTION('ref_axis',(0.,0.,1.));
#29508=DIRECTION('center_axis',(6.19544098563146E-17,1.,0.));
#29509=DIRECTION('ref_axis',(-1.,6.19544098563146E-17,0.));
#29510=DIRECTION('center_axis',(-0.70710678118652,0.707106781186575,-7.61150822814556E-14));
#29511=DIRECTION('ref_axis',(0.707106781186575,0.70710678118652,-4.07577956776154E-9));
#29512=DIRECTION('center_axis',(0.,1.,0.));
#29513=DIRECTION('ref_axis',(0.,0.,1.));
#29514=DIRECTION('center_axis',(-0.707106781186515,0.70710678118658,9.0386660208839E-14));
#29515=DIRECTION('ref_axis',(0.70710678118658,0.707106781186515,-1.02669175321909E-8));
#29516=DIRECTION('center_axis',(6.19544098563146E-17,1.,0.));
#29517=DIRECTION('ref_axis',(-1.,6.19544098563146E-17,0.));
#29518=DIRECTION('',(0.,1.,0.));
#29519=DIRECTION('center_axis',(0.,1.,0.));
#29520=DIRECTION('ref_axis',(0.,0.,1.));
#29521=DIRECTION('center_axis',(6.19544098563146E-17,1.,0.));
#29522=DIRECTION('ref_axis',(-1.,6.19544098563146E-17,0.));
#29523=DIRECTION('center_axis',(0.707106781186539,0.707106781186556,2.8543155855425E-14));
#29524=DIRECTION('ref_axis',(0.707106781186556,-0.707106781186539,-4.86876680138915E-9));
#29525=DIRECTION('center_axis',(0.,1.,0.));
#29526=DIRECTION('ref_axis',(0.,0.,1.));
#29527=DIRECTION('center_axis',(0.707106781186531,0.707106781186564,-5.23291190687391E-14));
#29528=DIRECTION('ref_axis',(0.707106781186564,-0.707106781186531,-1.99327366961659E-9));
#29529=DIRECTION('center_axis',(0.,1.,0.));
#29530=DIRECTION('ref_axis',(0.,0.,1.));
#29531=DIRECTION('center_axis',(0.,1.,0.));
#29532=DIRECTION('ref_axis',(0.,0.,1.));
#29533=DIRECTION('',(0.,1.,0.));
#29534=DIRECTION('center_axis',(0.,1.,0.));
#29535=DIRECTION('ref_axis',(0.,0.,1.));
#29536=DIRECTION('center_axis',(0.,1.,0.));
#29537=DIRECTION('ref_axis',(0.,0.,1.));
#29538=DIRECTION('center_axis',(6.19544098563146E-17,1.,0.));
#29539=DIRECTION('ref_axis',(-1.,6.19544098563146E-17,0.));
#29540=DIRECTION('center_axis',(-0.707106781186522,0.707106781186573,-7.13578896385657E-14));
#29541=DIRECTION('ref_axis',(0.707106781186573,0.707106781186522,6.06499231681277E-9));
#29542=DIRECTION('center_axis',(0.,1.,0.));
#29543=DIRECTION('ref_axis',(0.,0.,1.));
#29544=DIRECTION('center_axis',(-0.707106781186519,0.707106781186576,8.08722749240661E-14));
#29545=DIRECTION('ref_axis',(0.707106781186576,0.707106781186519,-1.40864771617222E-10));
#29546=DIRECTION('center_axis',(6.19544098563146E-17,1.,0.));
#29547=DIRECTION('ref_axis',(-1.,6.19544098563146E-17,0.));
#29548=DIRECTION('',(0.,1.,0.));
#29549=DIRECTION('center_axis',(0.,1.,0.));
#29550=DIRECTION('ref_axis',(0.,0.,1.));
#29551=DIRECTION('center_axis',(6.19544098563146E-17,1.,0.));
#29552=DIRECTION('ref_axis',(-1.,6.19544098563146E-17,0.));
#29553=DIRECTION('center_axis',(0.707106781186539,0.707106781186557,3.21110503373454E-14));
#29554=DIRECTION('ref_axis',(0.707106781186556,-0.707106781186539,-4.86391357561765E-9));
#29555=DIRECTION('center_axis',(0.,1.,0.));
#29556=DIRECTION('ref_axis',(0.,0.,1.));
#29557=DIRECTION('center_axis',(0.707106781186532,0.707106781186563,-4.99505227472087E-14));
#29558=DIRECTION('ref_axis',(0.707106781186563,-0.707106781186532,-5.10750268434258E-9));
#29559=DIRECTION('center_axis',(0.,1.,0.));
#29560=DIRECTION('ref_axis',(0.,0.,1.));
#29561=DIRECTION('center_axis',(0.,1.,0.));
#29562=DIRECTION('ref_axis',(0.,0.,1.));
#29563=DIRECTION('',(0.,1.,0.));
#29564=DIRECTION('center_axis',(0.,1.,0.));
#29565=DIRECTION('ref_axis',(0.,0.,1.));
#29566=DIRECTION('center_axis',(0.,1.,0.));
#29567=DIRECTION('ref_axis',(0.,0.,1.));
#29568=DIRECTION('center_axis',(6.19544098563146E-17,1.,0.));
#29569=DIRECTION('ref_axis',(-1.,6.19544098563146E-17,0.));
#29570=DIRECTION('center_axis',(-0.707106781186522,0.707106781186573,-7.13578896387188E-14));
#29571=DIRECTION('ref_axis',(0.707106781186573,0.707106781186522,7.5295440732973E-10));
#29572=DIRECTION('center_axis',(0.,1.,0.));
#29573=DIRECTION('ref_axis',(0.,0.,1.));
#29574=DIRECTION('center_axis',(-0.707106781186517,0.707106781186578,8.32508712456219E-14));
#29575=DIRECTION('ref_axis',(0.707106781186578,0.707106781186517,-1.68444693514637E-9));
#29576=DIRECTION('center_axis',(6.19544098563146E-17,1.,0.));
#29577=DIRECTION('ref_axis',(-1.,6.19544098563146E-17,0.));
#29578=DIRECTION('',(0.,1.,0.));
#29579=DIRECTION('center_axis',(0.,1.,0.));
#29580=DIRECTION('ref_axis',(0.,0.,1.));
#29581=DIRECTION('center_axis',(6.19544098563146E-17,1.,0.));
#29582=DIRECTION('ref_axis',(-1.,6.19544098563146E-17,0.));
#29583=DIRECTION('center_axis',(0.707106781186545,0.707106781186551,1.54608760883638E-14));
#29584=DIRECTION('ref_axis',(0.70710678118655,-0.707106781186544,-3.54497137075718E-9));
#29585=DIRECTION('center_axis',(0.,1.,0.));
#29586=DIRECTION('ref_axis',(0.,0.,1.));
#29587=DIRECTION('center_axis',(0.707106781186539,0.707106781186556,-3.09217521768553E-14));
#29588=DIRECTION('ref_axis',(0.707106781186556,-0.707106781186539,-6.02871288395333E-10));
#29589=DIRECTION('center_axis',(0.,1.,0.));
#29590=DIRECTION('ref_axis',(0.,0.,1.));
#29591=DIRECTION('center_axis',(0.,1.,0.));
#29592=DIRECTION('ref_axis',(0.,0.,1.));
#29593=DIRECTION('',(0.,1.,0.));
#29594=DIRECTION('center_axis',(0.,1.,0.));
#29595=DIRECTION('ref_axis',(0.,0.,1.));
#29596=DIRECTION('center_axis',(0.,1.,0.));
#29597=DIRECTION('ref_axis',(0.,0.,1.));
#29598=DIRECTION('center_axis',(6.19544098563146E-17,1.,0.));
#29599=DIRECTION('ref_axis',(-1.,6.19544098563146E-17,0.));
#29600=DIRECTION('center_axis',(-0.707106781186537,0.707106781186558,-2.14073668916551E-14));
#29601=DIRECTION('ref_axis',(0.707106781186558,0.707106781186537,-4.91138244991823E-9));
#29602=DIRECTION('center_axis',(0.,1.,0.));
#29603=DIRECTION('ref_axis',(0.,0.,1.));
#29604=DIRECTION('center_axis',(-0.707106781186534,0.707106781186561,3.09217521768376E-14));
#29605=DIRECTION('ref_axis',(0.707106781186561,0.707106781186534,-5.32748781420606E-10));
#29606=DIRECTION('center_axis',(6.19544098563146E-17,1.,0.));
#29607=DIRECTION('ref_axis',(-1.,6.19544098563146E-17,0.));
#29608=DIRECTION('',(0.,1.,0.));
#29609=DIRECTION('center_axis',(0.,1.,0.));
#29610=DIRECTION('ref_axis',(0.,0.,1.));
#29611=DIRECTION('center_axis',(6.19544098563146E-17,1.,0.));
#29612=DIRECTION('ref_axis',(-1.,6.19544098563146E-17,0.));
#29613=DIRECTION('center_axis',(0.707106781186538,0.707106781186557,3.33003484980685E-14));
#29614=DIRECTION('ref_axis',(0.707106781186557,-0.707106781186538,-2.51785900200259E-9));
#29615=DIRECTION('center_axis',(0.,1.,0.));
#29616=DIRECTION('ref_axis',(0.,0.,1.));
#29617=DIRECTION('center_axis',(0.707106781186537,0.707106781186558,-3.56789448195543E-14));
#29618=DIRECTION('ref_axis',(0.707106781186558,-0.707106781186537,-1.21671693251198E-9));
#29619=DIRECTION('center_axis',(0.,1.,0.));
#29620=DIRECTION('ref_axis',(0.,0.,1.));
#29621=DIRECTION('center_axis',(0.,1.,0.));
#29622=DIRECTION('ref_axis',(0.,0.,1.));
#29623=DIRECTION('',(0.,1.,0.));
#29624=DIRECTION('center_axis',(0.,1.,0.));
#29625=DIRECTION('ref_axis',(0.,0.,1.));
#29626=DIRECTION('center_axis',(0.,1.,0.));
#29627=DIRECTION('ref_axis',(0.,0.,1.));
#29628=DIRECTION('center_axis',(6.19544098563146E-17,1.,0.));
#29629=DIRECTION('ref_axis',(-1.,6.19544098563146E-17,0.));
#29630=DIRECTION('center_axis',(-0.707106781186544,0.707106781186551,-1.18929816064752E-15));
#29631=DIRECTION('ref_axis',(0.707106781186551,0.707106781186544,-2.79028008532548E-9));
#29632=DIRECTION('center_axis',(0.,1.,0.));
#29633=DIRECTION('ref_axis',(0.,0.,1.));
#29634=DIRECTION('center_axis',(-0.707106781186539,0.707106781186556,1.42715779277559E-14));
#29635=DIRECTION('ref_axis',(0.707106781186556,0.707106781186539,-3.56410008544113E-9));
#29636=DIRECTION('center_axis',(6.19544098563146E-17,1.,0.));
#29637=DIRECTION('ref_axis',(-1.,6.19544098563146E-17,0.));
#29638=DIRECTION('',(0.,1.,0.));
#29639=DIRECTION('center_axis',(0.,1.,0.));
#29640=DIRECTION('ref_axis',(0.,0.,1.));
#29641=DIRECTION('center_axis',(6.19544098563146E-17,1.,0.));
#29642=DIRECTION('ref_axis',(-1.,6.19544098563146E-17,0.));
#29643=DIRECTION('center_axis',(0.707106781186545,0.707106781186551,1.42715779278094E-14));
#29644=DIRECTION('ref_axis',(0.70710678118655,-0.707106781186544,2.08661794038888E-9));
#29645=DIRECTION('center_axis',(0.,1.,0.));
#29646=DIRECTION('ref_axis',(0.,0.,1.));
#29647=DIRECTION('center_axis',(0.707106781186539,0.707106781186556,-3.09217521767969E-14));
#29648=DIRECTION('ref_axis',(0.707106781186556,-0.707106781186539,-1.0692782140686E-9));
#29649=DIRECTION('center_axis',(0.,1.,0.));
#29650=DIRECTION('ref_axis',(0.,0.,1.));
#29651=DIRECTION('center_axis',(0.,1.,0.));
#29652=DIRECTION('ref_axis',(0.,0.,1.));
#29653=DIRECTION('',(0.,1.,0.));
#29654=DIRECTION('center_axis',(0.,1.,0.));
#29655=DIRECTION('ref_axis',(0.,0.,1.));
#29656=DIRECTION('center_axis',(0.,1.,0.));
#29657=DIRECTION('ref_axis',(0.,0.,1.));
#29658=DIRECTION('center_axis',(6.19544098563146E-17,1.,0.));
#29659=DIRECTION('ref_axis',(-1.,6.19544098563146E-17,0.));
#29660=DIRECTION('center_axis',(-0.707106781186536,0.707106781186559,-2.37859632129691E-14));
#29661=DIRECTION('ref_axis',(0.707106781186559,0.707106781186536,1.5906322003989E-9));
#29662=DIRECTION('center_axis',(0.,1.,0.));
#29663=DIRECTION('ref_axis',(0.,0.,1.));
#29664=DIRECTION('center_axis',(-0.707106781186543,0.707106781186552,4.75719264259406E-15));
#29665=DIRECTION('ref_axis',(0.707106781186552,0.707106781186543,-1.87099840895288E-9));
#29666=DIRECTION('center_axis',(6.19544098563146E-17,1.,0.));
#29667=DIRECTION('ref_axis',(-1.,6.19544098563146E-17,0.));
#29668=DIRECTION('',(0.,1.,0.));
#29669=DIRECTION('center_axis',(0.,1.,0.));
#29670=DIRECTION('ref_axis',(0.,0.,1.));
#29671=DIRECTION('center_axis',(6.19544098563146E-17,1.,0.));
#29672=DIRECTION('ref_axis',(-1.,6.19544098563146E-17,0.));
#29673=DIRECTION('center_axis',(0.707106781186536,0.707106781186559,3.80575411406882E-14));
#29674=DIRECTION('ref_axis',(0.707106781186559,-0.707106781186536,-4.18851469439042E-10));
#29675=DIRECTION('center_axis',(0.,1.,0.));
#29676=DIRECTION('ref_axis',(0.,0.,1.));
#29677=DIRECTION('center_axis',(0.707106781186532,0.707106781186563,-4.99505227472632E-14));
#29678=DIRECTION('ref_axis',(0.707106781186563,-0.707106781186532,3.80158663483794E-10));
#29679=DIRECTION('center_axis',(0.,1.,0.));
#29680=DIRECTION('ref_axis',(0.,0.,1.));
#29681=DIRECTION('center_axis',(0.,1.,0.));
#29682=DIRECTION('ref_axis',(0.,0.,1.));
#29683=DIRECTION('',(0.,1.,0.));
#29684=DIRECTION('center_axis',(0.,1.,0.));
#29685=DIRECTION('ref_axis',(0.,0.,1.));
#29686=DIRECTION('center_axis',(0.,1.,0.));
#29687=DIRECTION('ref_axis',(0.,0.,1.));
#29688=DIRECTION('center_axis',(6.19544098563146E-17,1.,0.));
#29689=DIRECTION('ref_axis',(-1.,6.19544098563146E-17,0.));
#29690=DIRECTION('center_axis',(-0.707106781186545,0.707106781186551,2.37859632129592E-15));
#29691=DIRECTION('ref_axis',(0.70710678118655,0.707106781186545,4.53820074720942E-10));
#29692=DIRECTION('center_axis',(0.,1.,0.));
#29693=DIRECTION('ref_axis',(0.,0.,1.));
#29694=DIRECTION('center_axis',(-0.707106781186518,0.707106781186577,8.32508712452785E-14));
#29695=DIRECTION('ref_axis',(0.707106781186577,0.707106781186518,-3.07005203925342E-10));
#29696=DIRECTION('center_axis',(6.19544098563146E-17,1.,0.));
#29697=DIRECTION('ref_axis',(-1.,6.19544098563146E-17,0.));
#29698=DIRECTION('',(0.,1.,0.));
#29699=DIRECTION('center_axis',(0.,1.,0.));
#29700=DIRECTION('ref_axis',(0.,0.,1.));
#29701=DIRECTION('center_axis',(6.19544098563146E-17,1.,0.));
#29702=DIRECTION('ref_axis',(-1.,6.19544098563146E-17,0.));
#29703=DIRECTION('center_axis',(0.707106781186542,0.707106781186553,2.14073668916295E-14));
#29704=DIRECTION('ref_axis',(0.707106781186554,-0.707106781186542,8.8715406950362E-11));
#29705=DIRECTION('center_axis',(0.,1.,0.));
#29706=DIRECTION('ref_axis',(0.,0.,1.));
#29707=DIRECTION('center_axis',(0.707106781186542,0.707106781186553,-2.14073668916982E-14));
#29708=DIRECTION('ref_axis',(0.707106781186553,-0.707106781186542,5.58949393343591E-11));
#29709=DIRECTION('center_axis',(0.,1.,0.));
#29710=DIRECTION('ref_axis',(0.,0.,1.));
#29711=DIRECTION('center_axis',(0.,1.,0.));
#29712=DIRECTION('ref_axis',(0.,0.,1.));
#29713=DIRECTION('',(0.,1.,0.));
#29714=DIRECTION('center_axis',(0.,1.,0.));
#29715=DIRECTION('ref_axis',(0.,0.,1.));
#29716=DIRECTION('center_axis',(0.,1.,0.));
#29717=DIRECTION('ref_axis',(0.,0.,1.));
#29718=DIRECTION('center_axis',(6.19544098563146E-17,1.,0.));
#29719=DIRECTION('ref_axis',(-1.,6.19544098563146E-17,0.));
#29720=DIRECTION('center_axis',(-0.707106781186529,0.707106781186566,-4.51933301046057E-14));
#29721=DIRECTION('ref_axis',(0.707106781186566,0.707106781186529,-4.56830670056408E-11));
#29722=DIRECTION('center_axis',(0.,1.,0.));
#29723=DIRECTION('ref_axis',(0.,0.,1.));
#29724=DIRECTION('center_axis',(-0.707106781186538,0.707106781186557,1.90287705703604E-14));
#29725=DIRECTION('ref_axis',(0.707106781186557,0.707106781186538,3.34877097628957E-11));
#29726=DIRECTION('center_axis',(6.19544098563146E-17,1.,0.));
#29727=DIRECTION('ref_axis',(-1.,6.19544098563146E-17,0.));
#29728=DIRECTION('',(0.,1.,0.));
#29729=DIRECTION('center_axis',(0.,1.,0.));
#29730=DIRECTION('ref_axis',(0.,0.,1.));
#29731=DIRECTION('center_axis',(6.19544098563146E-17,1.,0.));
#29732=DIRECTION('ref_axis',(-1.,6.19544098563146E-17,0.));
#29733=DIRECTION('center_axis',(0.707106781186535,0.70710678118656,4.16254356226834E-14));
#29734=DIRECTION('ref_axis',(0.70710678118656,-0.707106781186535,-8.62446084296705E-11));
#29735=DIRECTION('center_axis',(0.,1.,0.));
#29736=DIRECTION('ref_axis',(0.,0.,1.));
#29737=DIRECTION('center_axis',(0.707106781186536,0.707106781186559,-4.04361374620356E-14));
#29738=DIRECTION('ref_axis',(0.707106781186559,-0.707106781186536,7.09281942410052E-11));
#29739=DIRECTION('center_axis',(-0.707106781186544,0.707106781186551,0.));
#29740=DIRECTION('ref_axis',(-0.707106781186551,-0.707106781186544,0.));
#29741=DIRECTION('',(0.,0.,1.));
#29742=DIRECTION('',(0.,0.,1.));
#29743=DIRECTION('',(-0.707106781186551,-0.707106781186544,0.));
#29744=DIRECTION('center_axis',(0.707106781186551,0.707106781186544,0.));
#29745=DIRECTION('ref_axis',(-0.707106781186544,0.707106781186551,0.));
#29746=DIRECTION('',(0.,0.,1.));
#29747=DIRECTION('',(0.,0.,1.));
#29748=DIRECTION('center_axis',(1.22464679914735E-16,-1.,0.));
#29749=DIRECTION('ref_axis',(1.,1.22464679914735E-16,0.));
#29750=DIRECTION('',(0.,0.,1.));
#29751=DIRECTION('',(0.,0.,1.));
#29752=DIRECTION('',(0.,0.,1.));
#29753=DIRECTION('',(0.,0.,1.));
#29754=DIRECTION('',(0.,0.,1.));
#29755=DIRECTION('',(0.,0.,1.));
#29756=DIRECTION('',(0.,0.,1.));
#29757=DIRECTION('',(0.,0.,1.));
#29758=DIRECTION('',(0.,0.,1.));
#29759=DIRECTION('',(0.,0.,1.));
#29760=DIRECTION('',(0.,0.,1.));
#29761=DIRECTION('',(0.,0.,1.));
#29762=DIRECTION('',(0.,0.,1.));
#29763=DIRECTION('',(0.,0.,1.));
#29764=DIRECTION('',(0.,0.,1.));
#29765=DIRECTION('',(1.,1.22464679914735E-16,0.));
#29766=DIRECTION('',(0.,0.,1.));
#29767=DIRECTION('',(1.,1.22464679914735E-16,0.));
#29768=DIRECTION('center_axis',(6.19544098563146E-17,1.,0.));
#29769=DIRECTION('ref_axis',(-1.,6.19544098563146E-17,0.));
#29770=DIRECTION('',(0.,0.,1.));
#29771=DIRECTION('center_axis',(1.22464679914735E-16,-1.,0.));
#29772=DIRECTION('ref_axis',(1.,1.22464679914735E-16,0.));
#29773=DIRECTION('',(0.,0.,1.));
#29774=DIRECTION('',(1.,1.22464679914735E-16,0.));
#29775=DIRECTION('',(0.,0.,1.));
#29776=DIRECTION('',(1.,1.22464679914735E-16,0.));
#29777=DIRECTION('',(0.,0.,1.));
#29778=DIRECTION('',(0.,0.,1.));
#29779=DIRECTION('',(0.,0.,1.));
#29780=DIRECTION('',(0.,0.,1.));
#29781=DIRECTION('',(0.,0.,1.));
#29782=DIRECTION('',(0.,0.,1.));
#29783=DIRECTION('',(0.,0.,1.));
#29784=DIRECTION('',(0.,0.,1.));
#29785=DIRECTION('',(0.,0.,1.));
#29786=DIRECTION('',(0.,0.,1.));
#29787=DIRECTION('',(0.,0.,1.));
#29788=DIRECTION('',(0.,0.,1.));
#29789=DIRECTION('',(0.,0.,1.));
#29790=DIRECTION('',(0.,0.,1.));
#29791=DIRECTION('center_axis',(-0.707106781186544,0.707106781186551,0.));
#29792=DIRECTION('ref_axis',(-0.707106781186551,-0.707106781186544,0.));
#29793=DIRECTION('center_axis',(6.19544098563146E-17,1.,0.));
#29794=DIRECTION('ref_axis',(-1.,6.19544098563146E-17,0.));
#29795=DIRECTION('',(0.,0.,1.));
#29796=DIRECTION('',(0.,0.,1.));
#29797=DIRECTION('center_axis',(0.707106781186551,0.707106781186544,0.));
#29798=DIRECTION('ref_axis',(-0.707106781186544,0.707106781186551,0.));
#29799=DIRECTION('center_axis',(-0.707106781186544,0.707106781186551,0.));
#29800=DIRECTION('ref_axis',(-0.707106781186551,-0.707106781186544,0.));
#29801=DIRECTION('center_axis',(6.19544098563146E-17,1.,0.));
#29802=DIRECTION('ref_axis',(-1.,6.19544098563146E-17,0.));
#29803=DIRECTION('',(0.,0.,1.));
#29804=DIRECTION('',(0.,0.,1.));
#29805=DIRECTION('center_axis',(0.707106781186551,0.707106781186544,0.));
#29806=DIRECTION('ref_axis',(-0.707106781186544,0.707106781186551,0.));
#29807=DIRECTION('center_axis',(-0.707106781186544,0.707106781186551,0.));
#29808=DIRECTION('ref_axis',(-0.707106781186551,-0.707106781186544,0.));
#29809=DIRECTION('center_axis',(6.19544098563146E-17,1.,0.));
#29810=DIRECTION('ref_axis',(-1.,6.19544098563146E-17,0.));
#29811=DIRECTION('',(0.,0.,1.));
#29812=DIRECTION('',(0.,0.,1.));
#29813=DIRECTION('center_axis',(0.707106781186551,0.707106781186544,0.));
#29814=DIRECTION('ref_axis',(-0.707106781186544,0.707106781186551,0.));
#29815=DIRECTION('center_axis',(-0.707106781186544,0.707106781186551,0.));
#29816=DIRECTION('ref_axis',(-0.707106781186551,-0.707106781186544,0.));
#29817=DIRECTION('center_axis',(6.19544098563146E-17,1.,0.));
#29818=DIRECTION('ref_axis',(-1.,6.19544098563146E-17,0.));
#29819=DIRECTION('',(0.,0.,1.));
#29820=DIRECTION('',(0.,0.,1.));
#29821=DIRECTION('center_axis',(0.707106781186551,0.707106781186544,0.));
#29822=DIRECTION('ref_axis',(-0.707106781186544,0.707106781186551,0.));
#29823=DIRECTION('center_axis',(-0.707106781186544,0.707106781186551,0.));
#29824=DIRECTION('ref_axis',(-0.707106781186551,-0.707106781186544,0.));
#29825=DIRECTION('center_axis',(6.19544098563146E-17,1.,0.));
#29826=DIRECTION('ref_axis',(-1.,6.19544098563146E-17,0.));
#29827=DIRECTION('',(0.,0.,1.));
#29828=DIRECTION('',(0.,0.,1.));
#29829=DIRECTION('center_axis',(0.707106781186551,0.707106781186544,0.));
#29830=DIRECTION('ref_axis',(-0.707106781186544,0.707106781186551,0.));
#29831=DIRECTION('center_axis',(-0.707106781186544,0.707106781186551,0.));
#29832=DIRECTION('ref_axis',(-0.707106781186551,-0.707106781186544,0.));
#29833=DIRECTION('center_axis',(6.19544098563146E-17,1.,0.));
#29834=DIRECTION('ref_axis',(-1.,6.19544098563146E-17,0.));
#29835=DIRECTION('',(0.,0.,1.));
#29836=DIRECTION('',(0.,0.,1.));
#29837=DIRECTION('center_axis',(0.707106781186551,0.707106781186544,0.));
#29838=DIRECTION('ref_axis',(-0.707106781186544,0.707106781186551,0.));
#29839=DIRECTION('center_axis',(-0.707106781186544,0.707106781186551,0.));
#29840=DIRECTION('ref_axis',(-0.707106781186551,-0.707106781186544,0.));
#29841=DIRECTION('center_axis',(6.19544098563146E-17,1.,0.));
#29842=DIRECTION('ref_axis',(-1.,6.19544098563146E-17,0.));
#29843=DIRECTION('',(0.,0.,1.));
#29844=DIRECTION('',(0.,0.,1.));
#29845=DIRECTION('center_axis',(0.707106781186551,0.707106781186544,0.));
#29846=DIRECTION('ref_axis',(-0.707106781186544,0.707106781186551,0.));
#29847=DIRECTION('center_axis',(-0.707106781186544,0.707106781186551,0.));
#29848=DIRECTION('ref_axis',(-0.707106781186551,-0.707106781186544,0.));
#29849=DIRECTION('center_axis',(6.19544098563146E-17,1.,0.));
#29850=DIRECTION('ref_axis',(-1.,6.19544098563146E-17,0.));
#29851=DIRECTION('',(0.,0.,1.));
#29852=DIRECTION('',(0.,0.,1.));
#29853=DIRECTION('center_axis',(0.707106781186551,0.707106781186544,0.));
#29854=DIRECTION('ref_axis',(-0.707106781186544,0.707106781186551,0.));
#29855=DIRECTION('center_axis',(-0.707106781186544,0.707106781186551,0.));
#29856=DIRECTION('ref_axis',(-0.707106781186551,-0.707106781186544,0.));
#29857=DIRECTION('center_axis',(6.19544098563146E-17,1.,0.));
#29858=DIRECTION('ref_axis',(-1.,6.19544098563146E-17,0.));
#29859=DIRECTION('',(0.,0.,1.));
#29860=DIRECTION('',(0.,0.,1.));
#29861=DIRECTION('center_axis',(0.707106781186551,0.707106781186544,0.));
#29862=DIRECTION('ref_axis',(-0.707106781186544,0.707106781186551,0.));
#29863=DIRECTION('center_axis',(6.19544098563146E-17,1.,0.));
#29864=DIRECTION('ref_axis',(-1.,6.19544098563146E-17,0.));
#29865=DIRECTION('',(0.,0.,1.));
#29866=DIRECTION('',(0.,0.,1.));
#29867=DIRECTION('center_axis',(-0.707106781186544,0.707106781186551,0.));
#29868=DIRECTION('ref_axis',(-0.707106781186551,-0.707106781186544,0.));
#29869=DIRECTION('center_axis',(0.707106781186551,0.707106781186544,0.));
#29870=DIRECTION('ref_axis',(-0.707106781186544,0.707106781186551,0.));
#29871=DIRECTION('center_axis',(-0.707106781186544,0.707106781186551,0.));
#29872=DIRECTION('ref_axis',(-0.707106781186551,-0.707106781186544,0.));
#29873=DIRECTION('center_axis',(6.19544098563146E-17,1.,0.));
#29874=DIRECTION('ref_axis',(-1.,6.19544098563146E-17,0.));
#29875=DIRECTION('',(0.,0.,1.));
#29876=DIRECTION('',(0.,0.,1.));
#29877=DIRECTION('center_axis',(0.707106781186551,0.707106781186544,0.));
#29878=DIRECTION('ref_axis',(-0.707106781186544,0.707106781186551,0.));
#29879=DIRECTION('center_axis',(-0.707106781186544,0.707106781186551,0.));
#29880=DIRECTION('ref_axis',(-0.707106781186551,-0.707106781186544,0.));
#29881=DIRECTION('center_axis',(6.19544098563146E-17,1.,0.));
#29882=DIRECTION('ref_axis',(-1.,6.19544098563146E-17,0.));
#29883=DIRECTION('',(0.,0.,1.));
#29884=DIRECTION('',(0.,0.,1.));
#29885=DIRECTION('center_axis',(0.707106781186551,0.707106781186544,0.));
#29886=DIRECTION('ref_axis',(-0.707106781186544,0.707106781186551,0.));
#29887=DIRECTION('center_axis',(6.19544098563146E-17,1.,0.));
#29888=DIRECTION('ref_axis',(-1.,6.19544098563146E-17,0.));
#29889=DIRECTION('',(0.,0.,1.));
#29890=DIRECTION('',(0.,0.,1.));
#29891=DIRECTION('center_axis',(-0.707106781186544,0.707106781186551,0.));
#29892=DIRECTION('ref_axis',(-0.707106781186551,-0.707106781186544,0.));
#29893=DIRECTION('center_axis',(0.707106781186551,0.707106781186544,0.));
#29894=DIRECTION('ref_axis',(-0.707106781186544,0.707106781186551,0.));
#29895=DIRECTION('center_axis',(6.19544098563146E-17,1.,0.));
#29896=DIRECTION('ref_axis',(-1.,6.19544098563146E-17,0.));
#29897=DIRECTION('',(0.,0.,1.));
#29898=DIRECTION('',(0.,0.,1.));
#29899=DIRECTION('',(-1.,6.19544098563146E-17,0.));
#29900=DIRECTION('center_axis',(-0.707106781186544,0.707106781186551,0.));
#29901=DIRECTION('ref_axis',(-0.707106781186551,-0.707106781186544,0.));
#29902=DIRECTION('center_axis',(0.707106781186551,0.707106781186544,0.));
#29903=DIRECTION('ref_axis',(-0.707106781186544,0.707106781186551,0.));
#29904=DIRECTION('',(-0.707106781186544,0.707106781186551,0.));
#29905=DIRECTION('center_axis',(0.,0.,-1.));
#29906=DIRECTION('ref_axis',(-1.,0.,0.));
#29907=DIRECTION('',(0.707106781186544,-0.707106781186551,0.));
#29908=DIRECTION('',(0.,-1.,0.));
#29909=DIRECTION('center_axis',(0.,0.,-1.));
#29910=DIRECTION('ref_axis',(-1.,0.,0.));
#29911=DIRECTION('',(-0.707106781186551,-0.707106781186544,0.));
#29912=DIRECTION('center_axis',(0.,0.,1.));
#29913=DIRECTION('ref_axis',(-1.,0.,0.));
#29914=DIRECTION('',(0.,-1.,0.));
#29915=DIRECTION('center_axis',(0.,0.,1.));
#29916=DIRECTION('ref_axis',(-1.,0.,0.));
#29917=DIRECTION('',(0.707106781186544,-0.707106781186551,0.));
#29918=DIRECTION('center_axis',(0.,0.,-1.));
#29919=DIRECTION('ref_axis',(-1.,0.,0.));
#29920=DIRECTION('center_axis',(0.,0.,1.));
#29921=DIRECTION('ref_axis',(1.,0.,0.));
#29922=DIRECTION('center_axis',(0.,0.,-1.));
#29923=DIRECTION('ref_axis',(-1.,0.,0.));
#29924=DIRECTION('',(0.707106781186544,-0.707106781186551,0.));
#29925=DIRECTION('center_axis',(0.,0.,-1.));
#29926=DIRECTION('ref_axis',(-1.,0.,0.));
#29927=DIRECTION('',(0.,-1.,0.));
#29928=DIRECTION('center_axis',(0.,0.,-1.));
#29929=DIRECTION('ref_axis',(-1.,0.,0.));
#29930=DIRECTION('',(-0.70710678118655,-0.707106781186545,0.));
#29931=DIRECTION('center_axis',(0.,0.,-1.));
#29932=DIRECTION('ref_axis',(-1.,0.,0.));
#29933=DIRECTION('center_axis',(0.,0.,1.));
#29934=DIRECTION('ref_axis',(1.,0.,0.));
#29935=DIRECTION('center_axis',(0.,0.,-1.));
#29936=DIRECTION('ref_axis',(-1.,0.,0.));
#29937=DIRECTION('',(-0.70710678118655,-0.707106781186545,0.));
#29938=DIRECTION('',(-1.,0.,0.));
#29939=DIRECTION('',(0.70710678118655,-0.707106781186545,0.));
#29940=DIRECTION('center_axis',(0.,0.,-1.));
#29941=DIRECTION('ref_axis',(-1.,0.,0.));
#29942=DIRECTION('center_axis',(0.,0.,-1.));
#29943=DIRECTION('ref_axis',(-1.,0.,0.));
#29944=DIRECTION('center_axis',(0.,0.,-1.));
#29945=DIRECTION('ref_axis',(-1.,0.,0.));
#29946=DIRECTION('',(0.70710678118655,-0.707106781186545,0.));
#29947=DIRECTION('center_axis',(0.,0.,-1.));
#29948=DIRECTION('ref_axis',(-1.,0.,0.));
#29949=DIRECTION('',(0.,-1.,0.));
#29950=DIRECTION('center_axis',(0.,0.,-1.));
#29951=DIRECTION('ref_axis',(-1.,0.,0.));
#29952=DIRECTION('',(-0.707106781186544,-0.707106781186551,0.));
#29953=DIRECTION('center_axis',(0.,0.,-1.));
#29954=DIRECTION('ref_axis',(-1.,0.,0.));
#29955=DIRECTION('center_axis',(0.,0.,-1.));
#29956=DIRECTION('ref_axis',(-1.,0.,0.));
#29957=DIRECTION('center_axis',(0.,0.,-1.));
#29958=DIRECTION('ref_axis',(-1.,0.,0.));
#29959=DIRECTION('',(-0.707106781186544,-0.707106781186551,0.));
#29960=DIRECTION('center_axis',(0.,0.,1.));
#29961=DIRECTION('ref_axis',(-1.,-3.46944695195361E-15,0.));
#29962=DIRECTION('',(0.,-1.,0.));
#29963=DIRECTION('center_axis',(0.,0.,1.));
#29964=DIRECTION('ref_axis',(-1.,0.,0.));
#29965=DIRECTION('',(0.707106781186551,-0.707106781186544,0.));
#29966=DIRECTION('center_axis',(0.,0.,-1.));
#29967=DIRECTION('ref_axis',(-1.,0.,0.));
#29968=DIRECTION('',(0.,-1.,0.));
#29969=DIRECTION('',(-0.707106781186544,-0.707106781186551,0.));
#29970=DIRECTION('',(-0.707106781186544,0.707106781186551,0.));
#29971=DIRECTION('',(-1.,6.19544098563146E-17,0.));
#29972=DIRECTION('center_axis',(0.,0.,-1.));
#29973=DIRECTION('ref_axis',(-1.,0.,0.));
#29974=DIRECTION('',(-0.707106781186551,-0.707106781186544,0.));
#29975=DIRECTION('',(-0.707106781186544,-0.707106781186551,0.));
#29976=DIRECTION('',(0.,-1.,0.));
#29977=DIRECTION('center_axis',(0.,0.,1.));
#29978=DIRECTION('ref_axis',(-1.,1.73472347597681E-15,0.));
#29979=DIRECTION('',(0.707106781186551,-0.707106781186544,0.));
#29980=DIRECTION('center_axis',(0.,0.,-1.));
#29981=DIRECTION('ref_axis',(-1.,0.,0.));
#29982=DIRECTION('',(0.,-1.,0.));
#29983=DIRECTION('center_axis',(0.,0.,-1.));
#29984=DIRECTION('ref_axis',(-1.,0.,0.));
#29985=DIRECTION('',(-0.707106781186544,-0.707106781186551,0.));
#29986=DIRECTION('center_axis',(0.,0.,1.));
#29987=DIRECTION('ref_axis',(-1.,0.,0.));
#29988=DIRECTION('center_axis',(0.,0.,-1.));
#29989=DIRECTION('ref_axis',(-1.,0.,0.));
#29990=DIRECTION('center_axis',(0.,0.,1.));
#29991=DIRECTION('ref_axis',(-1.,-6.93889390390722E-15,0.));
#29992=DIRECTION('',(-0.707106781186544,-0.707106781186551,0.));
#29993=DIRECTION('center_axis',(0.,0.,1.));
#29994=DIRECTION('ref_axis',(-1.,0.,0.));
#29995=DIRECTION('',(0.,-1.,0.));
#29996=DIRECTION('center_axis',(0.,0.,1.));
#29997=DIRECTION('ref_axis',(-1.,0.,0.));
#29998=DIRECTION('',(0.70710678118655,-0.707106781186545,0.));
#29999=DIRECTION('center_axis',(0.,0.,1.));
#30000=DIRECTION('ref_axis',(-1.,0.,0.));
#30001=DIRECTION('center_axis',(0.,0.,-1.));
#30002=DIRECTION('ref_axis',(-1.,0.,0.));
#30003=DIRECTION('center_axis',(0.,0.,1.));
#30004=DIRECTION('ref_axis',(-1.,0.,0.));
#30005=DIRECTION('',(0.70710678118655,-0.707106781186545,0.));
#30006=DIRECTION('',(-1.,0.,0.));
#30007=DIRECTION('',(-0.70710678118655,-0.707106781186545,0.));
#30008=DIRECTION('center_axis',(0.,0.,1.));
#30009=DIRECTION('ref_axis',(-1.,0.,0.));
#30010=DIRECTION('center_axis',(0.,0.,1.));
#30011=DIRECTION('ref_axis',(1.,0.,0.));
#30012=DIRECTION('center_axis',(0.,0.,1.));
#30013=DIRECTION('ref_axis',(-1.,-6.93889390390722E-15,0.));
#30014=DIRECTION('',(-0.70710678118655,-0.707106781186545,0.));
#30015=DIRECTION('center_axis',(0.,0.,1.));
#30016=DIRECTION('ref_axis',(-1.,6.93889390390722E-15,0.));
#30017=DIRECTION('',(0.,-1.,0.));
#30018=DIRECTION('center_axis',(0.,0.,1.));
#30019=DIRECTION('ref_axis',(-1.,0.,0.));
#30020=DIRECTION('',(0.707106781186544,-0.707106781186551,0.));
#30021=DIRECTION('center_axis',(0.,0.,1.));
#30022=DIRECTION('ref_axis',(-1.,0.,0.));
#30023=DIRECTION('center_axis',(0.,0.,1.));
#30024=DIRECTION('ref_axis',(1.,0.,0.));
#30025=DIRECTION('center_axis',(0.,0.,1.));
#30026=DIRECTION('ref_axis',(-1.,0.,0.));
#30027=DIRECTION('',(0.707106781186544,-0.707106781186551,0.));
#30028=DIRECTION('center_axis',(0.,0.,-1.));
#30029=DIRECTION('ref_axis',(-1.,0.,0.));
#30030=DIRECTION('',(0.,-1.,0.));
#30031=DIRECTION('center_axis',(0.,0.,-1.));
#30032=DIRECTION('ref_axis',(-1.,0.,0.));
#30033=DIRECTION('',(-0.707106781186551,-0.707106781186544,0.));
#30034=DIRECTION('center_axis',(0.,0.,1.));
#30035=DIRECTION('ref_axis',(-1.,1.12757025938492E-14,0.));
#30036=DIRECTION('',(0.,-1.,0.));
#30037=DIRECTION('',(0.707106781186544,-0.707106781186551,0.));
#30038=DIRECTION('center_axis',(-0.70710678118655,0.707106781186545,0.));
#30039=DIRECTION('ref_axis',(-0.707106781186545,-0.70710678118655,0.));
#30040=DIRECTION('',(0.,0.,-1.));
#30041=DIRECTION('',(0.,0.,1.));
#30042=DIRECTION('center_axis',(-0.70710678118655,0.707106781186545,0.));
#30043=DIRECTION('ref_axis',(-0.707106781186545,-0.70710678118655,0.));
#30044=DIRECTION('',(0.,0.,1.));
#30045=DIRECTION('',(0.,0.,-1.));
#30046=DIRECTION('center_axis',(-0.707106781186545,-0.70710678118655,0.));
#30047=DIRECTION('ref_axis',(0.70710678118655,-0.707106781186545,0.));
#30048=DIRECTION('',(0.,0.,1.));
#30049=DIRECTION('',(0.,0.,-1.));
#30050=DIRECTION('center_axis',(-0.707106781186545,-0.70710678118655,0.));
#30051=DIRECTION('ref_axis',(0.70710678118655,-0.707106781186545,0.));
#30052=DIRECTION('',(0.,0.,-1.));
#30053=DIRECTION('',(0.,0.,1.));
#30054=DIRECTION('center_axis',(-0.70710678118655,-0.707106781186545,0.));
#30055=DIRECTION('ref_axis',(0.707106781186545,-0.70710678118655,0.));
#30056=DIRECTION('',(0.,0.,1.));
#30057=DIRECTION('',(0.,0.,-1.));
#30058=DIRECTION('center_axis',(-0.707106781186545,0.70710678118655,0.));
#30059=DIRECTION('ref_axis',(-0.70710678118655,-0.707106781186545,0.));
#30060=DIRECTION('',(0.,0.,-1.));
#30061=DIRECTION('',(0.,0.,1.));
#30062=DIRECTION('center_axis',(0.,1.,0.));
#30063=DIRECTION('ref_axis',(0.,0.,1.));
#30064=DIRECTION('',(0.,0.,1.));
#30065=DIRECTION('center_axis',(-0.707106781186551,-0.707106781186544,0.));
#30066=DIRECTION('ref_axis',(0.707106781186544,-0.707106781186551,0.));
#30067=DIRECTION('',(0.,0.,1.));
#30068=DIRECTION('center_axis',(-1.,0.,0.));
#30069=DIRECTION('ref_axis',(0.,0.,1.));
#30070=DIRECTION('',(0.,0.,-1.));
#30071=DIRECTION('center_axis',(-0.707106781186544,0.707106781186551,0.));
#30072=DIRECTION('ref_axis',(-0.707106781186551,-0.707106781186544,0.));
#30073=DIRECTION('',(0.,0.,1.));
#30074=DIRECTION('',(0.,0.,-1.));
#30075=DIRECTION('center_axis',(-1.,0.,0.));
#30076=DIRECTION('ref_axis',(0.,0.,1.));
#30077=DIRECTION('',(0.,0.,1.));
#30078=DIRECTION('',(0.,0.,-1.));
#30079=DIRECTION('center_axis',(-0.70710678118655,-0.707106781186545,0.));
#30080=DIRECTION('ref_axis',(0.707106781186545,-0.70710678118655,0.));
#30081=DIRECTION('',(0.,0.,-1.));
#30082=DIRECTION('',(0.,0.,1.));
#30083=DIRECTION('center_axis',(-1.,0.,0.));
#30084=DIRECTION('ref_axis',(0.,0.,1.));
#30085=DIRECTION('',(0.,0.,-1.));
#30086=DIRECTION('',(0.,0.,1.));
#30087=DIRECTION('center_axis',(-0.707106781186545,0.70710678118655,0.));
#30088=DIRECTION('ref_axis',(-0.70710678118655,-0.707106781186545,0.));
#30089=DIRECTION('',(0.,0.,1.));
#30090=DIRECTION('center_axis',(0.,0.,1.));
#30091=DIRECTION('ref_axis',(1.,0.,0.));
#30092=DIRECTION('',(0.,0.,1.));
#30093=DIRECTION('',(0.,0.,-1.));
#30094=DIRECTION('center_axis',(0.,0.,1.));
#30095=DIRECTION('ref_axis',(1.,0.,0.));
#30096=DIRECTION('',(0.,0.,-1.));
#30097=DIRECTION('',(0.,0.,1.));
#30098=DIRECTION('center_axis',(0.,0.,1.));
#30099=DIRECTION('ref_axis',(1.,0.,0.));
#30100=DIRECTION('center_axis',(0.,0.,1.));
#30101=DIRECTION('ref_axis',(1.,0.,0.));
#30102=DIRECTION('center_axis',(0.,0.,1.));
#30103=DIRECTION('ref_axis',(1.,0.,0.));
#30104=DIRECTION('center_axis',(0.,0.,1.));
#30105=DIRECTION('ref_axis',(1.,0.,0.));
#30106=DIRECTION('center_axis',(0.,0.,-1.));
#30107=DIRECTION('ref_axis',(-1.,0.,0.));
#30108=DIRECTION('center_axis',(0.,0.,-1.));
#30109=DIRECTION('ref_axis',(-1.,0.,0.));
#30110=DIRECTION('center_axis',(0.,0.,1.));
#30111=DIRECTION('ref_axis',(1.,0.,0.));
#30112=DIRECTION('center_axis',(0.,0.,1.));
#30113=DIRECTION('ref_axis',(1.,0.,0.));
#30114=DIRECTION('center_axis',(0.,0.,1.));
#30115=DIRECTION('ref_axis',(1.,0.,0.));
#30116=DIRECTION('center_axis',(-1.,0.,0.));
#30117=DIRECTION('ref_axis',(0.,0.,1.));
#30118=DIRECTION('',(0.,0.,1.));
#30119=DIRECTION('',(0.,0.,-1.));
#30120=DIRECTION('center_axis',(-1.,0.,0.));
#30121=DIRECTION('ref_axis',(0.,0.,1.));
#30122=DIRECTION('',(0.,0.,-1.));
#30123=DIRECTION('',(0.,0.,1.));
#30124=DIRECTION('center_axis',(-0.707106781186544,-0.707106781186551,0.));
#30125=DIRECTION('ref_axis',(0.707106781186551,-0.707106781186544,0.));
#30126=DIRECTION('',(0.,0.,-1.));
#30127=DIRECTION('',(0.,0.,1.));
#30128=DIRECTION('center_axis',(-1.,0.,0.));
#30129=DIRECTION('ref_axis',(0.,0.,1.));
#30130=DIRECTION('',(0.,0.,1.));
#30131=DIRECTION('',(0.,0.,1.));
#30132=DIRECTION('center_axis',(-0.707106781186551,0.707106781186544,0.));
#30133=DIRECTION('ref_axis',(-0.707106781186544,-0.707106781186551,0.));
#30134=DIRECTION('center_axis',(0.,0.,1.));
#30135=DIRECTION('ref_axis',(1.,0.,0.));
#30136=DIRECTION('',(0.,0.,-1.));
#30137=DIRECTION('',(0.,0.,1.));
#30138=DIRECTION('center_axis',(0.,0.,1.));
#30139=DIRECTION('ref_axis',(1.,0.,0.));
#30140=DIRECTION('',(0.,0.,1.));
#30141=DIRECTION('',(0.,0.,-1.));
#30142=DIRECTION('center_axis',(0.,0.,1.));
#30143=DIRECTION('ref_axis',(1.,0.,0.));
#30144=DIRECTION('center_axis',(0.,0.,1.));
#30145=DIRECTION('ref_axis',(1.,0.,0.));
#30146=DIRECTION('center_axis',(0.,0.,1.));
#30147=DIRECTION('ref_axis',(1.,0.,0.));
#30148=DIRECTION('center_axis',(0.,0.,1.));
#30149=DIRECTION('ref_axis',(1.,0.,0.));
#30150=DIRECTION('center_axis',(0.,0.,-1.));
#30151=DIRECTION('ref_axis',(-1.,0.,0.));
#30152=DIRECTION('center_axis',(0.,0.,-1.));
#30153=DIRECTION('ref_axis',(-1.,0.,0.));
#30154=DIRECTION('center_axis',(0.,0.,1.));
#30155=DIRECTION('ref_axis',(1.,0.,0.));
#30156=DIRECTION('center_axis',(0.,0.,1.));
#30157=DIRECTION('ref_axis',(1.,0.,0.));
#30158=DIRECTION('center_axis',(0.,0.,1.));
#30159=DIRECTION('ref_axis',(1.,0.,0.));
#30160=DIRECTION('center_axis',(-0.707106781186544,0.707106781186551,0.));
#30161=DIRECTION('ref_axis',(-0.707106781186551,-0.707106781186544,0.));
#30162=DIRECTION('center_axis',(6.19544098563146E-17,1.,0.));
#30163=DIRECTION('ref_axis',(-1.,6.19544098563146E-17,0.));
#30164=DIRECTION('',(0.,0.,1.));
#30165=DIRECTION('center_axis',(0.707106781186551,0.707106781186544,0.));
#30166=DIRECTION('ref_axis',(-0.707106781186544,0.707106781186551,0.));
#30167=DIRECTION('center_axis',(0.,-1.,0.));
#30168=DIRECTION('ref_axis',(0.,0.,-1.));
#30169=DIRECTION('center_axis',(0.,-1.,0.));
#30170=DIRECTION('ref_axis',(0.,0.,-1.));
#30171=DIRECTION('center_axis',(0.,-1.,0.));
#30172=DIRECTION('ref_axis',(0.,0.,-1.));
#30173=DIRECTION('center_axis',(0.,-1.,0.));
#30174=DIRECTION('ref_axis',(0.,0.,-1.));
#30175=DIRECTION('center_axis',(0.,-1.,0.));
#30176=DIRECTION('ref_axis',(0.,0.,-1.));
#30177=DIRECTION('center_axis',(0.,-1.,0.));
#30178=DIRECTION('ref_axis',(0.,0.,-1.));
#30179=DIRECTION('center_axis',(0.,-1.,0.));
#30180=DIRECTION('ref_axis',(0.,0.,-1.));
#30181=DIRECTION('center_axis',(0.,-1.,0.));
#30182=DIRECTION('ref_axis',(0.,0.,-1.));
#30183=DIRECTION('center_axis',(0.,-1.,0.));
#30184=DIRECTION('ref_axis',(0.,0.,-1.));
#30185=DIRECTION('center_axis',(0.,-1.,0.));
#30186=DIRECTION('ref_axis',(0.,0.,-1.));
#30187=DIRECTION('center_axis',(0.,-1.,0.));
#30188=DIRECTION('ref_axis',(0.,0.,-1.));
#30189=DIRECTION('center_axis',(0.,-1.,0.));
#30190=DIRECTION('ref_axis',(0.,0.,-1.));
#30191=DIRECTION('center_axis',(0.,-1.,0.));
#30192=DIRECTION('ref_axis',(0.,0.,-1.));
#30193=DIRECTION('center_axis',(0.,-1.,0.));
#30194=DIRECTION('ref_axis',(0.,0.,-1.));
#30195=DIRECTION('center_axis',(0.,-1.,0.));
#30196=DIRECTION('ref_axis',(0.,0.,-1.));
#30197=DIRECTION('axis',(0.,0.,1.));
#30198=DIRECTION('refdir',(1.,0.,0.));
#30199=DIRECTION('center_axis',(1.,0.,0.));
#30200=DIRECTION('ref_axis',(0.,0.,-1.));
#30201=DIRECTION('center_axis',(1.,0.,0.));
#30202=DIRECTION('ref_axis',(0.,0.,-1.));
#30203=DIRECTION('',(1.,0.,0.));
#30204=DIRECTION('center_axis',(1.,0.,0.));
#30205=DIRECTION('ref_axis',(0.,0.,-1.));
#30206=DIRECTION('center_axis',(-1.,0.,0.));
#30207=DIRECTION('ref_axis',(0.,0.,1.));
#30208=DIRECTION('center_axis',(-1.,0.,0.));
#30209=DIRECTION('ref_axis',(0.,0.,1.));
#30210=DIRECTION('',(-1.,0.,0.));
#30211=DIRECTION('center_axis',(-1.,0.,0.));
#30212=DIRECTION('ref_axis',(0.,0.,1.));
#30213=DIRECTION('center_axis',(-1.30104260698261E-15,1.,-1.73611473352215E-31));
#30214=DIRECTION('ref_axis',(-1.,-1.30104260698261E-15,-2.16593351677506E-47));
#30215=DIRECTION('center_axis',(-1.30104260698261E-15,1.,-1.73611473352215E-31));
#30216=DIRECTION('ref_axis',(-1.,-1.30104260698261E-15,-2.16593351677507E-47));
#30217=DIRECTION('',(-1.30104260698261E-15,1.,-1.73611473352215E-31));
#30218=DIRECTION('center_axis',(-1.30104260698261E-15,1.,-1.73611473352215E-31));
#30219=DIRECTION('ref_axis',(-1.,-1.30104260698261E-15,-2.16593351677507E-47));
#30220=DIRECTION('center_axis',(1.,0.,0.));
#30221=DIRECTION('ref_axis',(0.,0.,-1.));
#30222=DIRECTION('',(0.515038074910055,-1.04972719113862E-16,0.857167300702112));
#30223=DIRECTION('center_axis',(-1.,0.,0.));
#30224=DIRECTION('ref_axis',(0.,0.,1.));
#30225=DIRECTION('',(-0.515038074910054,-1.04972719113862E-16,-0.857167300702112));
#30226=DIRECTION('center_axis',(0.,1.,0.));
#30227=DIRECTION('ref_axis',(0.,0.,1.));
#30228=DIRECTION('center_axis',(-1.2823896663807E-16,1.,0.));
#30229=DIRECTION('ref_axis',(-1.,-1.2823896663807E-16,0.));
#30230=DIRECTION('',(0.,1.,0.));
#30231=DIRECTION('center_axis',(0.,1.,0.));
#30232=DIRECTION('ref_axis',(0.,0.,1.));
#30233=DIRECTION('center_axis',(0.,1.,0.));
#30234=DIRECTION('ref_axis',(0.,0.,1.));
#30235=DIRECTION('center_axis',(-1.2823896663807E-16,1.,0.));
#30236=DIRECTION('ref_axis',(-1.,-1.2823896663807E-16,0.));
#30237=DIRECTION('',(0.,1.,0.));
#30238=DIRECTION('center_axis',(0.,1.,0.));
#30239=DIRECTION('ref_axis',(0.,0.,1.));
#30240=DIRECTION('center_axis',(0.,1.,0.));
#30241=DIRECTION('ref_axis',(0.,0.,1.));
#30242=DIRECTION('center_axis',(1.2823896663807E-16,1.,0.));
#30243=DIRECTION('ref_axis',(-1.,1.2823896663807E-16,0.));
#30244=DIRECTION('',(0.,1.,0.));
#30245=DIRECTION('center_axis',(0.,1.,0.));
#30246=DIRECTION('ref_axis',(0.,0.,1.));
#30247=DIRECTION('center_axis',(0.,1.,0.));
#30248=DIRECTION('ref_axis',(0.,0.,1.));
#30249=DIRECTION('center_axis',(1.2823896663807E-16,1.,0.));
#30250=DIRECTION('ref_axis',(-1.,1.2823896663807E-16,0.));
#30251=DIRECTION('',(0.,1.,0.));
#30252=DIRECTION('center_axis',(0.,1.,0.));
#30253=DIRECTION('ref_axis',(0.,0.,1.));
#30254=DIRECTION('center_axis',(-1.,0.,0.));
#30255=DIRECTION('ref_axis',(0.,0.,1.));
#30256=DIRECTION('center_axis',(-1.,0.,0.));
#30257=DIRECTION('ref_axis',(0.,0.,1.));
#30258=DIRECTION('',(-1.,0.,0.));
#30259=DIRECTION('center_axis',(-1.,0.,0.));
#30260=DIRECTION('ref_axis',(0.,0.,1.));
#30261=DIRECTION('center_axis',(1.,0.,0.));
#30262=DIRECTION('ref_axis',(0.,0.,-1.));
#30263=DIRECTION('center_axis',(1.,0.,0.));
#30264=DIRECTION('ref_axis',(0.,0.,-1.));
#30265=DIRECTION('',(1.,0.,0.));
#30266=DIRECTION('center_axis',(1.,0.,0.));
#30267=DIRECTION('ref_axis',(0.,0.,-1.));
#30268=DIRECTION('center_axis',(-1.30104260698261E-15,1.,-1.73611473352215E-31));
#30269=DIRECTION('ref_axis',(-1.,-1.30104260698261E-15,-2.16593351677506E-47));
#30270=DIRECTION('center_axis',(-1.30104260698261E-15,1.,-1.73611473352215E-31));
#30271=DIRECTION('ref_axis',(-1.,-1.30104260698261E-15,-2.16593351677507E-47));
#30272=DIRECTION('',(-1.30104260698261E-15,1.,-1.73611473352215E-31));
#30273=DIRECTION('center_axis',(-1.30104260698261E-15,1.,-1.73611473352215E-31));
#30274=DIRECTION('ref_axis',(-1.,-1.30104260698261E-15,-2.16593351677507E-47));
#30275=DIRECTION('center_axis',(-1.30104260698261E-15,1.,-1.73611473352215E-31));
#30276=DIRECTION('ref_axis',(-1.,-1.30104260698261E-15,2.25875923892257E-46));
#30277=DIRECTION('center_axis',(-1.30104260698261E-15,1.,-1.73611473352215E-31));
#30278=DIRECTION('ref_axis',(-1.,-1.30104260698261E-15,2.25875923892257E-46));
#30279=DIRECTION('',(-1.30104260698261E-15,1.,-1.73611473352215E-31));
#30280=DIRECTION('center_axis',(-1.30104260698261E-15,1.,-1.73611473352215E-31));
#30281=DIRECTION('ref_axis',(-1.,-1.30104260698261E-15,2.25875923892257E-46));
#30282=DIRECTION('',(-1.30104260698261E-15,1.,-1.73611473352215E-31));
#30283=DIRECTION('center_axis',(-1.30104260698261E-15,1.,-1.73611473352215E-31));
#30284=DIRECTION('ref_axis',(-1.,-1.30104260698261E-15,2.25875923892257E-46));
#30285=DIRECTION('',(-1.30104260698261E-15,1.,-1.73611473352215E-31));
#30286=DIRECTION('center_axis',(-1.,0.,0.));
#30287=DIRECTION('ref_axis',(0.,0.,1.));
#30288=DIRECTION('',(-0.515038074910054,-1.04972719113862E-16,-0.857167300702112));
#30289=DIRECTION('center_axis',(1.,0.,0.));
#30290=DIRECTION('ref_axis',(0.,0.,-1.));
#30291=DIRECTION('',(0.515038074910055,-1.04972719113862E-16,0.857167300702112));
#30292=DIRECTION('center_axis',(-1.30104260698261E-15,1.,-1.73611473352215E-31));
#30293=DIRECTION('ref_axis',(-1.,-1.30104260698261E-15,2.25875923892257E-46));
#30294=DIRECTION('center_axis',(-1.30104260698261E-15,1.,-1.73611473352215E-31));
#30295=DIRECTION('ref_axis',(-1.,-1.30104260698261E-15,2.25875923892257E-46));
#30296=DIRECTION('',(-1.30104260698261E-15,1.,-1.73611473352215E-31));
#30297=DIRECTION('',(-1.30104260698261E-15,1.,-1.73611473352215E-31));
#30298=DIRECTION('center_axis',(-1.30104260698261E-15,1.,-1.73611473352215E-31));
#30299=DIRECTION('ref_axis',(-1.,-1.30104260698261E-15,2.25875923892257E-46));
#30300=DIRECTION('',(-1.30104260698261E-15,1.,-1.73611473352215E-31));
#30301=DIRECTION('center_axis',(-1.30104260698261E-15,1.,-1.73611473352215E-31));
#30302=DIRECTION('ref_axis',(-1.,-1.30104260698261E-15,2.25875923892257E-46));
#30303=DIRECTION('center_axis',(0.,0.,1.));
#30304=DIRECTION('ref_axis',(-1.,0.,0.));
#30305=DIRECTION('center_axis',(0.,0.,1.));
#30306=DIRECTION('ref_axis',(-1.,0.,0.));
#30307=DIRECTION('center_axis',(0.,0.,1.));
#30308=DIRECTION('ref_axis',(1.,0.,0.));
#30309=DIRECTION('center_axis',(0.,0.,-1.));
#30310=DIRECTION('ref_axis',(-1.,0.,0.));
#30311=DIRECTION('',(0.,0.,-1.));
#30312=DIRECTION('center_axis',(0.,0.,-1.));
#30313=DIRECTION('ref_axis',(-1.,0.,0.));
#30314=DIRECTION('center_axis',(0.,0.,-1.));
#30315=DIRECTION('ref_axis',(-1.,0.,0.));
#30316=DIRECTION('',(0.,0.,-1.));
#30317=DIRECTION('center_axis',(0.,0.,-1.));
#30318=DIRECTION('ref_axis',(-1.,0.,0.));
#30319=DIRECTION('center_axis',(0.61566147532566,-0.788010753606721,0.));
#30320=DIRECTION('ref_axis',(0.78801075360672,0.61566147532566,0.));
#30321=DIRECTION('center_axis',(0.615661475325656,-0.788010753606724,-5.22755357805913E-15));
#30322=DIRECTION('ref_axis',(0.788010753606724,0.615661475325656,-5.17730530723809E-13));
#30323=DIRECTION('',(0.,0.,1.));
#30324=DIRECTION('',(0.78801075360672,0.61566147532566,0.));
#30325=DIRECTION('',(0.,0.,1.));
#30326=DIRECTION('center_axis',(0.61566147532566,-0.788010753606721,0.));
#30327=DIRECTION('ref_axis',(0.78801075360672,0.61566147532566,0.));
#30328=DIRECTION('center_axis',(0.615661475325656,-0.788010753606724,5.27148259972344E-15));
#30329=DIRECTION('ref_axis',(0.788010753606724,0.615661475325656,-9.16833363821094E-14));
#30330=DIRECTION('',(0.,0.,1.));
#30331=DIRECTION('center_axis',(0.615661475325662,-0.788010753606719,1.40572869325959E-15));
#30332=DIRECTION('ref_axis',(0.788010753606719,0.615661475325662,-7.1472163446861E-13));
#30333=DIRECTION('',(0.,0.,1.));
#30334=DIRECTION('center_axis',(-0.61566147532566,-0.788010753606721,0.));
#30335=DIRECTION('ref_axis',(0.78801075360672,-0.61566147532566,0.));
#30336=DIRECTION('center_axis',(-0.615661475325663,-0.788010753606718,-3.73396684147081E-15));
#30337=DIRECTION('ref_axis',(0.788010753606718,-0.615661475325663,1.05496270744081E-13));
#30338=DIRECTION('',(0.,0.,1.));
#30339=DIRECTION('center_axis',(-0.615661475325666,-0.788010753606716,6.32577911966821E-15));
#30340=DIRECTION('ref_axis',(0.788010753606716,-0.615661475325666,2.12834187078208E-13));
#30341=DIRECTION('',(0.,0.,1.));
#30342=DIRECTION('center_axis',(-0.61566147532566,-0.788010753606721,0.));
#30343=DIRECTION('ref_axis',(0.78801075360672,-0.61566147532566,0.));
#30344=DIRECTION('center_axis',(-0.615661475325663,-0.788010753606718,-3.64610879814206E-15));
#30345=DIRECTION('ref_axis',(0.788010753606718,-0.615661475325663,-2.42930938978673E-14));
#30346=DIRECTION('',(0.,0.,1.));
#30347=DIRECTION('',(0.78801075360672,-0.61566147532566,0.));
#30348=DIRECTION('',(0.,0.,1.));
#30349=DIRECTION('center_axis',(-0.707106781186546,0.707106781186549,0.));
#30350=DIRECTION('ref_axis',(-0.707106781186549,-0.707106781186546,0.));
#30351=DIRECTION('',(-0.707106781186549,-0.707106781186546,0.));
#30352=DIRECTION('',(0.,0.,-1.));
#30353=DIRECTION('',(-0.707106781186549,-0.707106781186546,0.));
#30354=DIRECTION('',(0.,0.,1.));
#30355=DIRECTION('center_axis',(-0.707106781186549,-0.707106781186546,0.));
#30356=DIRECTION('ref_axis',(0.707106781186546,-0.707106781186549,0.));
#30357=DIRECTION('',(0.707106781186545,-0.70710678118655,0.));
#30358=DIRECTION('',(0.,0.,-1.));
#30359=DIRECTION('',(0.707106781186546,-0.707106781186549,0.));
#30360=DIRECTION('',(0.,0.,1.));
#30361=DIRECTION('center_axis',(0.707106781186546,0.707106781186549,0.));
#30362=DIRECTION('ref_axis',(-0.707106781186549,0.707106781186546,0.));
#30363=DIRECTION('',(-0.707106781186548,0.707106781186547,0.));
#30364=DIRECTION('',(0.,0.,-1.));
#30365=DIRECTION('',(-0.707106781186549,0.707106781186546,0.));
#30366=DIRECTION('',(0.,0.,1.));
#30367=DIRECTION('center_axis',(0.707106781186549,-0.707106781186546,0.));
#30368=DIRECTION('ref_axis',(0.707106781186546,0.707106781186549,0.));
#30369=DIRECTION('',(0.707106781186546,0.707106781186549,0.));
#30370=DIRECTION('',(0.,0.,-1.));
#30371=DIRECTION('',(0.707106781186546,0.707106781186549,0.));
#30372=DIRECTION('',(0.,0.,1.));
#30373=DIRECTION('center_axis',(0.707106781186549,-0.707106781186546,0.));
#30374=DIRECTION('ref_axis',(0.707106781186546,0.707106781186549,0.));
#30375=DIRECTION('',(0.707106781186545,0.70710678118655,0.));
#30376=DIRECTION('',(0.,0.,-1.));
#30377=DIRECTION('',(0.707106781186546,0.707106781186549,0.));
#30378=DIRECTION('',(0.,0.,1.));
#30379=DIRECTION('center_axis',(1.,0.,0.));
#30380=DIRECTION('ref_axis',(0.,0.,-1.));
#30381=DIRECTION('',(0.,1.,0.));
#30382=DIRECTION('',(0.,0.,-1.));
#30383=DIRECTION('',(0.,1.,0.));
#30384=DIRECTION('',(0.,0.,1.));
#30385=DIRECTION('center_axis',(0.707106781186546,0.707106781186549,0.));
#30386=DIRECTION('ref_axis',(-0.707106781186549,0.707106781186546,0.));
#30387=DIRECTION('',(-0.707106781186549,0.707106781186546,0.));
#30388=DIRECTION('',(0.,0.,-1.));
#30389=DIRECTION('',(-0.707106781186549,0.707106781186546,0.));
#30390=DIRECTION('',(0.,0.,1.));
#30391=DIRECTION('center_axis',(1.,0.,0.));
#30392=DIRECTION('ref_axis',(0.,0.,-1.));
#30393=DIRECTION('',(0.,1.,0.));
#30394=DIRECTION('',(0.,0.,-1.));
#30395=DIRECTION('',(0.,1.,0.));
#30396=DIRECTION('',(0.,0.,1.));
#30397=DIRECTION('center_axis',(0.707106781186549,-0.707106781186546,0.));
#30398=DIRECTION('ref_axis',(0.707106781186546,0.707106781186549,0.));
#30399=DIRECTION('',(0.707106781186546,0.707106781186549,0.));
#30400=DIRECTION('',(0.,0.,1.));
#30401=DIRECTION('',(0.707106781186546,0.707106781186549,0.));
#30402=DIRECTION('',(0.,0.,1.));
#30403=DIRECTION('center_axis',(0.,-1.,0.));
#30404=DIRECTION('ref_axis',(0.,0.,-1.));
#30405=DIRECTION('',(1.,0.,0.));
#30406=DIRECTION('',(0.,0.,1.));
#30407=DIRECTION('',(1.,0.,0.));
#30408=DIRECTION('center_axis',(-6.49101394191508E-16,-1.,0.));
#30409=DIRECTION('ref_axis',(1.,-6.49101394191508E-16,0.));
#30410=DIRECTION('',(1.,-3.50803534070133E-16,0.));
#30411=DIRECTION('',(0.,0.,1.));
#30412=DIRECTION('',(1.,-6.49101394191508E-16,0.));
#30413=DIRECTION('',(0.,0.,1.));
#30414=DIRECTION('center_axis',(-0.707106781186549,-0.707106781186546,0.));
#30415=DIRECTION('ref_axis',(0.707106781186546,-0.707106781186549,0.));
#30416=DIRECTION('',(0.707106781186546,-0.707106781186549,0.));
#30417=DIRECTION('',(0.,0.,-1.));
#30418=DIRECTION('',(0.707106781186546,-0.707106781186549,0.));
#30419=DIRECTION('center_axis',(-1.,0.,0.));
#30420=DIRECTION('ref_axis',(0.,0.,1.));
#30421=DIRECTION('',(0.,-1.,0.));
#30422=DIRECTION('',(0.,0.,-1.));
#30423=DIRECTION('',(0.,-1.,0.));
#30424=DIRECTION('',(0.,0.,1.));
#30425=DIRECTION('center_axis',(-0.707106781186546,0.707106781186549,0.));
#30426=DIRECTION('ref_axis',(-0.707106781186549,-0.707106781186546,0.));
#30427=DIRECTION('',(-0.707106781186548,-0.707106781186547,0.));
#30428=DIRECTION('',(0.,0.,-1.));
#30429=DIRECTION('',(-0.707106781186549,-0.707106781186546,0.));
#30430=DIRECTION('',(0.,0.,1.));
#30431=DIRECTION('center_axis',(-1.,0.,0.));
#30432=DIRECTION('ref_axis',(0.,0.,1.));
#30433=DIRECTION('',(0.,-1.,0.));
#30434=DIRECTION('',(0.,0.,-1.));
#30435=DIRECTION('',(0.,-1.,0.));
#30436=DIRECTION('',(0.,0.,1.));
#30437=DIRECTION('center_axis',(-0.707106781186549,-0.707106781186546,0.));
#30438=DIRECTION('ref_axis',(0.707106781186546,-0.707106781186549,0.));
#30439=DIRECTION('',(0.707106781186546,-0.707106781186549,0.));
#30440=DIRECTION('',(0.,0.,1.));
#30441=DIRECTION('',(0.707106781186546,-0.707106781186549,0.));
#30442=DIRECTION('',(0.,0.,1.));
#30443=DIRECTION('center_axis',(1.22464679914735E-16,-1.,0.));
#30444=DIRECTION('ref_axis',(1.,1.22464679914735E-16,0.));
#30445=DIRECTION('',(1.,1.22464679914735E-16,0.));
#30446=DIRECTION('',(1.,1.22464679914735E-16,0.));
#30447=DIRECTION('center_axis',(0.,0.,1.));
#30448=DIRECTION('ref_axis',(1.,0.,0.));
#30449=DIRECTION('center_axis',(0.,0.,1.));
#30450=DIRECTION('ref_axis',(1.,0.,0.));
#30451=DIRECTION('',(0.,0.,-1.));
#30452=DIRECTION('center_axis',(0.,0.,1.));
#30453=DIRECTION('ref_axis',(1.,0.,0.));
#30454=DIRECTION('',(0.,0.,1.));
#30455=DIRECTION('center_axis',(0.,0.,1.));
#30456=DIRECTION('ref_axis',(1.,0.,0.));
#30457=DIRECTION('center_axis',(0.,0.,1.));
#30458=DIRECTION('ref_axis',(1.,0.,0.));
#30459=DIRECTION('',(0.,0.,-1.));
#30460=DIRECTION('center_axis',(0.,0.,1.));
#30461=DIRECTION('ref_axis',(1.,0.,0.));
#30462=DIRECTION('',(0.,0.,1.));
#30463=DIRECTION('center_axis',(0.,0.,1.));
#30464=DIRECTION('ref_axis',(1.,0.,0.));
#30465=DIRECTION('center_axis',(0.,0.,1.));
#30466=DIRECTION('ref_axis',(1.,0.,0.));
#30467=DIRECTION('',(0.,0.,-1.));
#30468=DIRECTION('center_axis',(0.,0.,1.));
#30469=DIRECTION('ref_axis',(1.,0.,0.));
#30470=DIRECTION('',(0.,0.,1.));
#30471=DIRECTION('center_axis',(0.,0.,1.));
#30472=DIRECTION('ref_axis',(1.,0.,0.));
#30473=DIRECTION('center_axis',(0.,0.,1.));
#30474=DIRECTION('ref_axis',(1.,0.,0.));
#30475=DIRECTION('',(0.,0.,-1.));
#30476=DIRECTION('center_axis',(0.,0.,1.));
#30477=DIRECTION('ref_axis',(1.,0.,0.));
#30478=DIRECTION('',(0.,0.,1.));
#30479=DIRECTION('center_axis',(0.,0.,1.));
#30480=DIRECTION('ref_axis',(1.,0.,0.));
#30481=DIRECTION('center_axis',(0.,0.,1.));
#30482=DIRECTION('ref_axis',(1.,0.,0.));
#30483=DIRECTION('center_axis',(0.,0.,-1.));
#30484=DIRECTION('ref_axis',(-1.,0.,0.));
#30485=DIRECTION('center_axis',(0.,0.,1.));
#30486=DIRECTION('ref_axis',(1.,0.,0.));
#30487=DIRECTION('center_axis',(0.,0.,1.));
#30488=DIRECTION('ref_axis',(1.,0.,0.));
#30489=DIRECTION('center_axis',(0.,0.,-1.));
#30490=DIRECTION('ref_axis',(-1.,0.,0.));
#30491=DIRECTION('center_axis',(0.,0.,-1.));
#30492=DIRECTION('ref_axis',(-1.,0.,0.));
#30493=DIRECTION('center_axis',(0.,0.,-1.));
#30494=DIRECTION('ref_axis',(1.,0.,0.));
#30495=DIRECTION('center_axis',(0.,0.,1.));
#30496=DIRECTION('ref_axis',(-1.,0.,0.));
#30497=DIRECTION('center_axis',(0.,0.,-1.));
#30498=DIRECTION('ref_axis',(-1.,0.,0.));
#30499=DIRECTION('center_axis',(0.,0.,-1.));
#30500=DIRECTION('ref_axis',(1.,0.,0.));
#30501=DIRECTION('center_axis',(0.,0.,1.));
#30502=DIRECTION('ref_axis',(-1.,-5.20417042793042E-15,0.));
#30503=DIRECTION('center_axis',(0.,0.,1.));
#30504=DIRECTION('ref_axis',(1.,0.,0.));
#30505=DIRECTION('center_axis',(0.,0.,-1.));
#30506=DIRECTION('ref_axis',(1.,0.,0.));
#30507=DIRECTION('center_axis',(0.,0.,1.));
#30508=DIRECTION('ref_axis',(-1.,-3.46944695195361E-15,0.));
#30509=DIRECTION('center_axis',(0.,0.,1.));
#30510=DIRECTION('ref_axis',(1.,0.,0.));
#30511=DIRECTION('center_axis',(0.,0.,-1.));
#30512=DIRECTION('ref_axis',(1.,0.,0.));
#30513=DIRECTION('center_axis',(0.,0.,1.));
#30514=DIRECTION('ref_axis',(-1.,5.42101086242752E-15,0.));
#30515=DIRECTION('center_axis',(0.,0.,1.));
#30516=DIRECTION('ref_axis',(1.,0.,0.));
#30517=DIRECTION('center_axis',(0.,0.,-1.));
#30518=DIRECTION('ref_axis',(1.,0.,0.));
#30519=DIRECTION('center_axis',(0.,0.,1.));
#30520=DIRECTION('ref_axis',(-1.,-1.73472347597681E-15,0.));
#30521=DIRECTION('center_axis',(0.,0.,1.));
#30522=DIRECTION('ref_axis',(1.,0.,0.));
#30523=DIRECTION('center_axis',(0.,0.,-1.));
#30524=DIRECTION('ref_axis',(1.,0.,0.));
#30525=DIRECTION('center_axis',(0.,0.,1.));
#30526=DIRECTION('ref_axis',(-1.,8.67361737988403E-15,0.));
#30527=DIRECTION('center_axis',(0.,0.,1.));
#30528=DIRECTION('ref_axis',(1.,0.,0.));
#30529=DIRECTION('center_axis',(0.,0.,1.));
#30530=DIRECTION('ref_axis',(1.,0.,0.));
#30531=DIRECTION('center_axis',(0.,0.,-1.));
#30532=DIRECTION('ref_axis',(-1.,0.,0.));
#30533=DIRECTION('center_axis',(0.,0.,1.));
#30534=DIRECTION('ref_axis',(1.,0.,0.));
#30535=DIRECTION('center_axis',(0.,0.,1.));
#30536=DIRECTION('ref_axis',(1.,0.,0.));
#30537=DIRECTION('center_axis',(0.,0.,-1.));
#30538=DIRECTION('ref_axis',(-1.,0.,0.));
#30539=DIRECTION('center_axis',(0.,0.,1.));
#30540=DIRECTION('ref_axis',(1.,0.,0.));
#30541=DIRECTION('center_axis',(0.,0.,-1.));
#30542=DIRECTION('ref_axis',(1.,0.,0.));
#30543=DIRECTION('center_axis',(0.,0.,1.));
#30544=DIRECTION('ref_axis',(-1.,1.73472347597681E-15,0.));
#30545=DIRECTION('center_axis',(0.,0.,1.));
#30546=DIRECTION('ref_axis',(1.,0.,0.));
#30547=DIRECTION('center_axis',(0.,0.,-1.));
#30548=DIRECTION('ref_axis',(1.,0.,0.));
#30549=DIRECTION('center_axis',(0.,0.,1.));
#30550=DIRECTION('ref_axis',(-1.,0.,0.));
#30551=DIRECTION('center_axis',(0.,0.,-1.));
#30552=DIRECTION('ref_axis',(-1.,0.,0.));
#30553=DIRECTION('center_axis',(0.,0.,-1.));
#30554=DIRECTION('ref_axis',(1.,0.,0.));
#30555=DIRECTION('center_axis',(0.,0.,1.));
#30556=DIRECTION('ref_axis',(-1.,0.,0.));
#30557=DIRECTION('center_axis',(0.,0.,-1.));
#30558=DIRECTION('ref_axis',(-1.,0.,0.));
#30559=DIRECTION('center_axis',(0.,0.,-1.));
#30560=DIRECTION('ref_axis',(1.,0.,0.));
#30561=DIRECTION('center_axis',(0.,0.,1.));
#30562=DIRECTION('ref_axis',(-1.,-1.64798730217797E-14,0.));
#30563=DIRECTION('center_axis',(0.,0.,1.));
#30564=DIRECTION('ref_axis',(1.,0.,0.));
#30565=DIRECTION('center_axis',(0.,0.,-1.));
#30566=DIRECTION('ref_axis',(1.,0.,0.));
#30567=DIRECTION('center_axis',(0.,0.,1.));
#30568=DIRECTION('ref_axis',(-1.,-1.73472347597681E-14,0.));
#30569=DIRECTION('center_axis',(0.,0.,1.));
#30570=DIRECTION('ref_axis',(1.,0.,0.));
#30571=DIRECTION('center_axis',(0.,0.,-1.));
#30572=DIRECTION('ref_axis',(1.,0.,0.));
#30573=DIRECTION('center_axis',(0.,0.,1.));
#30574=DIRECTION('ref_axis',(-1.,1.95156391047391E-14,0.));
#30575=DIRECTION('center_axis',(0.,0.,-1.));
#30576=DIRECTION('ref_axis',(-1.,0.,0.));
#30577=DIRECTION('center_axis',(0.,-1.,0.));
#30578=DIRECTION('ref_axis',(0.,0.,-1.));
#30579=DIRECTION('',(0.,0.,1.));
#30580=DIRECTION('',(-1.,0.,0.));
#30581=DIRECTION('',(0.,0.,1.));
#30582=DIRECTION('',(1.,0.,0.));
#30583=DIRECTION('center_axis',(0.,0.,-1.));
#30584=DIRECTION('ref_axis',(-1.,0.,0.));
#30585=DIRECTION('',(-0.707106781186547,0.707106781186548,0.));
#30586=DIRECTION('',(-1.26161707343768E-16,1.,0.));
#30587=DIRECTION('',(0.707106781186562,0.707106781186533,0.));
#30588=DIRECTION('',(0.707106781186562,-0.707106781186533,0.));
#30589=DIRECTION('',(-1.26161707343768E-16,-1.,0.));
#30590=DIRECTION('',(-0.707106781186547,-0.707106781186548,0.));
#30591=DIRECTION('center_axis',(0.707106781186533,-0.707106781186562,0.));
#30592=DIRECTION('ref_axis',(0.707106781186562,0.707106781186533,0.));
#30593=DIRECTION('',(0.,0.,1.));
#30594=DIRECTION('',(-0.707106781186562,-0.707106781186533,0.));
#30595=DIRECTION('center_axis',(1.,1.26161707343768E-16,0.));
#30596=DIRECTION('ref_axis',(-1.26161707343768E-16,1.,0.));
#30597=DIRECTION('',(0.,0.,1.));
#30598=DIRECTION('',(1.26161707343768E-16,-1.,0.));
#30599=DIRECTION('center_axis',(0.707106781186548,0.707106781186547,0.));
#30600=DIRECTION('ref_axis',(-0.707106781186547,0.707106781186548,0.));
#30601=DIRECTION('',(0.707106781186547,-0.707106781186548,0.));
#30602=DIRECTION('center_axis',(-0.707106781186548,0.707106781186547,0.));
#30603=DIRECTION('ref_axis',(-0.707106781186547,-0.707106781186548,0.));
#30604=DIRECTION('',(0.,0.,1.));
#30605=DIRECTION('',(0.707106781186547,0.707106781186548,0.));
#30606=DIRECTION('center_axis',(-1.,1.26161707343768E-16,0.));
#30607=DIRECTION('ref_axis',(-1.26161707343768E-16,-1.,0.));
#30608=DIRECTION('',(0.,0.,1.));
#30609=DIRECTION('',(1.26161707343768E-16,1.,0.));
#30610=DIRECTION('center_axis',(-0.707106781186533,-0.707106781186562,0.));
#30611=DIRECTION('ref_axis',(0.707106781186562,-0.707106781186533,0.));
#30612=DIRECTION('',(-0.707106781186562,0.707106781186533,0.));
#30613=DIRECTION('center_axis',(-0.866025403784439,0.5,0.));
#30614=DIRECTION('ref_axis',(-0.5,-0.866025403784439,0.));
#30615=DIRECTION('',(0.,0.,-1.));
#30616=DIRECTION('',(0.,0.,-1.));
#30617=DIRECTION('',(0.5,0.866025403784439,0.));
#30618=DIRECTION('center_axis',(-0.866025403784438,-0.5,0.));
#30619=DIRECTION('ref_axis',(0.5,-0.866025403784438,0.));
#30620=DIRECTION('',(-0.5,0.866025403784438,0.));
#30621=DIRECTION('',(0.,0.,-1.));
#30622=DIRECTION('center_axis',(7.51157299368579E-16,-1.,0.));
#30623=DIRECTION('ref_axis',(1.,7.5115729936858E-16,0.));
#30624=DIRECTION('',(0.,0.,-1.));
#30625=DIRECTION('',(-1.,-7.5115729936858E-16,0.));
#30626=DIRECTION('center_axis',(0.866025403784439,-0.5,0.));
#30627=DIRECTION('ref_axis',(0.5,0.866025403784439,0.));
#30628=DIRECTION('',(0.,0.,-1.));
#30629=DIRECTION('',(-0.5,-0.866025403784439,0.));
#30630=DIRECTION('center_axis',(0.866025403784439,0.5,0.));
#30631=DIRECTION('ref_axis',(-0.5,0.866025403784439,0.));
#30632=DIRECTION('',(0.,0.,-1.));
#30633=DIRECTION('',(0.5,-0.866025403784438,0.));
#30634=DIRECTION('center_axis',(0.,1.,0.));
#30635=DIRECTION('ref_axis',(0.,0.,1.));
#30636=DIRECTION('',(1.,0.,0.));
#30637=DIRECTION('center_axis',(0.,0.,-1.));
#30638=DIRECTION('ref_axis',(-1.,0.,0.));
#30639=DIRECTION('center_axis',(0.,0.,-1.));
#30640=DIRECTION('ref_axis',(1.,0.,0.));
#30641=DIRECTION('',(0.707106781186546,-0.707106781186549,0.));
#30642=DIRECTION('center_axis',(0.,0.,1.));
#30643=DIRECTION('ref_axis',(1.,0.,0.));
#30644=DIRECTION('',(0.,-1.,0.));
#30645=DIRECTION('center_axis',(0.,0.,1.));
#30646=DIRECTION('ref_axis',(1.,0.,0.));
#30647=DIRECTION('',(-0.707106781186552,-0.707106781186543,0.));
#30648=DIRECTION('center_axis',(0.,0.,-1.));
#30649=DIRECTION('ref_axis',(1.,0.,0.));
#30650=DIRECTION('center_axis',(0.,0.,1.));
#30651=DIRECTION('ref_axis',(1.,0.,0.));
#30652=DIRECTION('center_axis',(0.,0.,-1.));
#30653=DIRECTION('ref_axis',(1.,0.,0.));
#30654=DIRECTION('',(-0.707106781186552,-0.707106781186543,0.));
#30655=DIRECTION('center_axis',(0.,0.,-1.));
#30656=DIRECTION('ref_axis',(1.,0.,0.));
#30657=DIRECTION('',(0.,-1.,0.));
#30658=DIRECTION('center_axis',(0.,0.,-1.));
#30659=DIRECTION('ref_axis',(1.,0.,0.));
#30660=DIRECTION('',(0.707106781186547,-0.707106781186547,0.));
#30661=DIRECTION('center_axis',(0.,0.,-1.));
#30662=DIRECTION('ref_axis',(1.,0.,0.));
#30663=DIRECTION('center_axis',(0.,0.,1.));
#30664=DIRECTION('ref_axis',(1.,0.,0.));
#30665=DIRECTION('center_axis',(0.,0.,-1.));
#30666=DIRECTION('ref_axis',(1.,0.,0.));
#30667=DIRECTION('',(0.707106781186546,-0.707106781186549,0.));
#30668=DIRECTION('',(1.,4.61786466713945E-17,0.));
#30669=DIRECTION('',(0.707106781186547,0.707106781186548,0.));
#30670=DIRECTION('center_axis',(0.,0.,-1.));
#30671=DIRECTION('ref_axis',(1.,0.,0.));
#30672=DIRECTION('center_axis',(0.,0.,1.));
#30673=DIRECTION('ref_axis',(1.,0.,0.));
#30674=DIRECTION('center_axis',(0.,0.,-1.));
#30675=DIRECTION('ref_axis',(1.,0.,0.));
#30676=DIRECTION('',(0.707106781186546,0.707106781186549,0.));
#30677=DIRECTION('center_axis',(0.,0.,-1.));
#30678=DIRECTION('ref_axis',(1.,0.,0.));
#30679=DIRECTION('',(0.,1.,0.));
#30680=DIRECTION('center_axis',(0.,0.,-1.));
#30681=DIRECTION('ref_axis',(1.,0.,0.));
#30682=DIRECTION('',(-0.707106781186546,0.707106781186549,0.));
#30683=DIRECTION('center_axis',(0.,0.,-1.));
#30684=DIRECTION('ref_axis',(1.,0.,0.));
#30685=DIRECTION('center_axis',(0.,0.,1.));
#30686=DIRECTION('ref_axis',(1.,0.,0.));
#30687=DIRECTION('center_axis',(0.,0.,-1.));
#30688=DIRECTION('ref_axis',(1.,0.,0.));
#30689=DIRECTION('',(-0.707106781186552,0.707106781186543,0.));
#30690=DIRECTION('center_axis',(0.,0.,1.));
#30691=DIRECTION('ref_axis',(1.,0.,0.));
#30692=DIRECTION('',(0.,1.,0.));
#30693=DIRECTION('center_axis',(0.,0.,1.));
#30694=DIRECTION('ref_axis',(1.,0.,0.));
#30695=DIRECTION('',(0.707106781186546,0.707106781186549,0.));
#30696=DIRECTION('',(1.,0.,0.));
#30697=DIRECTION('',(0.707106781186547,-0.707106781186548,0.));
#30698=DIRECTION('',(1.26352022694434E-16,-1.,0.));
#30699=DIRECTION('',(-0.707106781186562,-0.707106781186533,0.));
#30700=DIRECTION('',(-1.,-1.95534159233113E-16,0.));
#30701=DIRECTION('',(-0.707106781186561,0.707106781186534,0.));
#30702=DIRECTION('',(0.,1.,0.));
#30703=DIRECTION('',(0.707106781186546,0.707106781186549,0.));
#30704=DIRECTION('',(1.,0.,0.));
#30705=DIRECTION('center_axis',(-0.707106781186549,-0.707106781186546,0.));
#30706=DIRECTION('ref_axis',(0.707106781186546,-0.707106781186549,0.));
#30707=DIRECTION('',(0.707106781186546,-0.707106781186549,0.));
#30708=DIRECTION('',(0.,0.,1.));
#30709=DIRECTION('',(0.,0.,1.));
#30710=DIRECTION('center_axis',(0.,0.,1.));
#30711=DIRECTION('ref_axis',(1.,0.,0.));
#30712=DIRECTION('center_axis',(0.,0.,1.));
#30713=DIRECTION('ref_axis',(1.,0.,0.));
#30714=DIRECTION('',(0.,0.,1.));
#30715=DIRECTION('center_axis',(-1.,0.,0.));
#30716=DIRECTION('ref_axis',(0.,0.,1.));
#30717=DIRECTION('',(0.,-1.,0.));
#30718=DIRECTION('',(0.,0.,1.));
#30719=DIRECTION('center_axis',(0.,0.,1.));
#30720=DIRECTION('ref_axis',(1.,0.,0.));
#30721=DIRECTION('center_axis',(0.,0.,1.));
#30722=DIRECTION('ref_axis',(1.,0.,0.));
#30723=DIRECTION('',(0.,0.,1.));
#30724=DIRECTION('center_axis',(-0.707106781186543,0.707106781186552,0.));
#30725=DIRECTION('ref_axis',(-0.707106781186552,-0.707106781186543,0.));
#30726=DIRECTION('',(-0.707106781186552,-0.707106781186543,0.));
#30727=DIRECTION('',(0.,0.,1.));
#30728=DIRECTION('center_axis',(0.,0.,1.));
#30729=DIRECTION('ref_axis',(1.,0.,0.));
#30730=DIRECTION('center_axis',(0.,0.,-1.));
#30731=DIRECTION('ref_axis',(1.,0.,0.));
#30732=DIRECTION('',(0.,0.,1.));
#30733=DIRECTION('center_axis',(0.,0.,1.));
#30734=DIRECTION('ref_axis',(1.,0.,0.));
#30735=DIRECTION('center_axis',(0.,0.,1.));
#30736=DIRECTION('ref_axis',(1.,0.,0.));
#30737=DIRECTION('',(0.,0.,1.));
#30738=DIRECTION('center_axis',(0.,0.,1.));
#30739=DIRECTION('ref_axis',(1.,0.,0.));
#30740=DIRECTION('center_axis',(0.,0.,-1.));
#30741=DIRECTION('ref_axis',(1.,0.,0.));
#30742=DIRECTION('',(0.,0.,1.));
#30743=DIRECTION('center_axis',(-0.707106781186543,0.707106781186552,0.));
#30744=DIRECTION('ref_axis',(-0.707106781186552,-0.707106781186543,0.));
#30745=DIRECTION('',(-0.707106781186552,-0.707106781186543,0.));
#30746=DIRECTION('',(0.,0.,1.));
#30747=DIRECTION('center_axis',(0.,0.,1.));
#30748=DIRECTION('ref_axis',(1.,0.,0.));
#30749=DIRECTION('center_axis',(0.,0.,-1.));
#30750=DIRECTION('ref_axis',(1.,0.,0.));
#30751=DIRECTION('',(0.,0.,1.));
#30752=DIRECTION('center_axis',(-1.,0.,0.));
#30753=DIRECTION('ref_axis',(0.,0.,1.));
#30754=DIRECTION('',(0.,-1.,0.));
#30755=DIRECTION('',(0.,0.,1.));
#30756=DIRECTION('center_axis',(0.,0.,1.));
#30757=DIRECTION('ref_axis',(1.,0.,0.));
#30758=DIRECTION('center_axis',(0.,0.,-1.));
#30759=DIRECTION('ref_axis',(1.,0.,0.));
#30760=DIRECTION('',(0.,0.,1.));
#30761=DIRECTION('center_axis',(-0.707106781186548,-0.707106781186548,0.));
#30762=DIRECTION('ref_axis',(0.707106781186548,-0.707106781186548,0.));
#30763=DIRECTION('',(0.707106781186547,-0.707106781186547,0.));
#30764=DIRECTION('',(0.,0.,1.));
#30765=DIRECTION('center_axis',(0.,0.,1.));
#30766=DIRECTION('ref_axis',(1.,0.,0.));
#30767=DIRECTION('center_axis',(0.,0.,-1.));
#30768=DIRECTION('ref_axis',(1.,0.,0.));
#30769=DIRECTION('',(0.,0.,1.));
#30770=DIRECTION('center_axis',(0.,0.,1.));
#30771=DIRECTION('ref_axis',(1.,0.,0.));
#30772=DIRECTION('center_axis',(0.,0.,1.));
#30773=DIRECTION('ref_axis',(1.,0.,0.));
#30774=DIRECTION('',(0.,0.,1.));
#30775=DIRECTION('center_axis',(0.,0.,1.));
#30776=DIRECTION('ref_axis',(1.,0.,0.));
#30777=DIRECTION('center_axis',(0.,0.,-1.));
#30778=DIRECTION('ref_axis',(1.,0.,0.));
#30779=DIRECTION('',(0.,0.,1.));
#30780=DIRECTION('center_axis',(-0.707106781186549,-0.707106781186546,0.));
#30781=DIRECTION('ref_axis',(0.707106781186546,-0.707106781186549,0.));
#30782=DIRECTION('',(0.707106781186546,-0.707106781186549,0.));
#30783=DIRECTION('',(0.,0.,1.));
#30784=DIRECTION('center_axis',(4.61786466713945E-17,-1.,0.));
#30785=DIRECTION('ref_axis',(1.,4.61786466713945E-17,0.));
#30786=DIRECTION('',(1.,4.61786466713945E-17,0.));
#30787=DIRECTION('',(0.,0.,1.));
#30788=DIRECTION('center_axis',(0.707106781186548,-0.707106781186547,0.));
#30789=DIRECTION('ref_axis',(0.707106781186547,0.707106781186548,0.));
#30790=DIRECTION('',(0.707106781186547,0.707106781186548,0.));
#30791=DIRECTION('',(0.,0.,1.));
#30792=DIRECTION('center_axis',(0.,0.,1.));
#30793=DIRECTION('ref_axis',(1.,0.,0.));
#30794=DIRECTION('center_axis',(0.,0.,-1.));
#30795=DIRECTION('ref_axis',(1.,0.,0.));
#30796=DIRECTION('',(0.,0.,1.));
#30797=DIRECTION('center_axis',(0.,0.,1.));
#30798=DIRECTION('ref_axis',(1.,0.,0.));
#30799=DIRECTION('center_axis',(0.,0.,1.));
#30800=DIRECTION('ref_axis',(1.,0.,0.));
#30801=DIRECTION('',(0.,0.,1.));
#30802=DIRECTION('center_axis',(0.,0.,1.));
#30803=DIRECTION('ref_axis',(1.,0.,0.));
#30804=DIRECTION('center_axis',(0.,0.,-1.));
#30805=DIRECTION('ref_axis',(1.,0.,0.));
#30806=DIRECTION('',(0.,0.,1.));
#30807=DIRECTION('center_axis',(0.70710678118655,-0.707106781186545,0.));
#30808=DIRECTION('ref_axis',(0.707106781186545,0.70710678118655,0.));
#30809=DIRECTION('',(0.707106781186546,0.707106781186549,0.));
#30810=DIRECTION('',(0.,0.,1.));
#30811=DIRECTION('center_axis',(0.,0.,1.));
#30812=DIRECTION('ref_axis',(1.,0.,0.));
#30813=DIRECTION('center_axis',(0.,0.,-1.));
#30814=DIRECTION('ref_axis',(1.,0.,0.));
#30815=DIRECTION('',(0.,0.,1.));
#30816=DIRECTION('center_axis',(1.,0.,0.));
#30817=DIRECTION('ref_axis',(0.,0.,-1.));
#30818=DIRECTION('',(0.,1.,0.));
#30819=DIRECTION('',(0.,0.,1.));
#30820=DIRECTION('center_axis',(0.,0.,1.));
#30821=DIRECTION('ref_axis',(1.,0.,0.));
#30822=DIRECTION('center_axis',(0.,0.,-1.));
#30823=DIRECTION('ref_axis',(1.,0.,0.));
#30824=DIRECTION('',(0.,0.,1.));
#30825=DIRECTION('center_axis',(0.707106781186549,0.707106781186546,0.));
#30826=DIRECTION('ref_axis',(-0.707106781186546,0.707106781186549,0.));
#30827=DIRECTION('',(-0.707106781186546,0.707106781186549,0.));
#30828=DIRECTION('',(0.,0.,1.));
#30829=DIRECTION('center_axis',(0.,0.,1.));
#30830=DIRECTION('ref_axis',(1.,0.,0.));
#30831=DIRECTION('center_axis',(0.,0.,-1.));
#30832=DIRECTION('ref_axis',(1.,0.,0.));
#30833=DIRECTION('',(0.,0.,1.));
#30834=DIRECTION('center_axis',(0.,0.,1.));
#30835=DIRECTION('ref_axis',(1.,0.,0.));
#30836=DIRECTION('center_axis',(0.,0.,1.));
#30837=DIRECTION('ref_axis',(1.,0.,0.));
#30838=DIRECTION('',(0.,0.,1.));
#30839=DIRECTION('center_axis',(0.,0.,1.));
#30840=DIRECTION('ref_axis',(1.,0.,0.));
#30841=DIRECTION('center_axis',(0.,0.,-1.));
#30842=DIRECTION('ref_axis',(1.,0.,0.));
#30843=DIRECTION('',(0.,0.,1.));
#30844=DIRECTION('center_axis',(0.707106781186543,0.707106781186552,0.));
#30845=DIRECTION('ref_axis',(-0.707106781186553,0.707106781186543,0.));
#30846=DIRECTION('',(-0.707106781186552,0.707106781186543,0.));
#30847=DIRECTION('',(0.,0.,1.));
#30848=DIRECTION('center_axis',(0.,0.,1.));
#30849=DIRECTION('ref_axis',(1.,0.,0.));
#30850=DIRECTION('center_axis',(0.,0.,1.));
#30851=DIRECTION('ref_axis',(1.,0.,0.));
#30852=DIRECTION('',(0.,0.,1.));
#30853=DIRECTION('center_axis',(1.,0.,0.));
#30854=DIRECTION('ref_axis',(0.,0.,-1.));
#30855=DIRECTION('',(0.,1.,0.));
#30856=DIRECTION('',(0.,0.,1.));
#30857=DIRECTION('center_axis',(0.,0.,1.));
#30858=DIRECTION('ref_axis',(1.,0.,0.));
#30859=DIRECTION('center_axis',(0.,0.,1.));
#30860=DIRECTION('ref_axis',(1.,0.,0.));
#30861=DIRECTION('',(0.,0.,1.));
#30862=DIRECTION('center_axis',(0.707106781186549,-0.707106781186546,0.));
#30863=DIRECTION('ref_axis',(0.707106781186546,0.707106781186549,0.));
#30864=DIRECTION('',(0.707106781186546,0.707106781186549,0.));
#30865=DIRECTION('',(0.,0.,1.));
#30866=DIRECTION('center_axis',(0.,-1.,0.));
#30867=DIRECTION('ref_axis',(0.,0.,-1.));
#30868=DIRECTION('',(1.,0.,0.));
#30869=DIRECTION('',(0.,0.,1.));
#30870=DIRECTION('center_axis',(-0.707106781186548,-0.707106781186547,0.));
#30871=DIRECTION('ref_axis',(0.707106781186547,-0.707106781186548,0.));
#30872=DIRECTION('',(0.707106781186547,-0.707106781186548,0.));
#30873=DIRECTION('',(0.,0.,1.));
#30874=DIRECTION('center_axis',(-1.,-1.26352022694434E-16,0.));
#30875=DIRECTION('ref_axis',(1.26352022694434E-16,-1.,0.));
#30876=DIRECTION('',(1.26352022694434E-16,-1.,0.));
#30877=DIRECTION('',(0.,0.,1.));
#30878=DIRECTION('center_axis',(-0.707106781186533,0.707106781186562,0.));
#30879=DIRECTION('ref_axis',(-0.707106781186562,-0.707106781186533,0.));
#30880=DIRECTION('',(-0.707106781186562,-0.707106781186533,0.));
#30881=DIRECTION('',(0.,0.,1.));
#30882=DIRECTION('center_axis',(-1.95534159233113E-16,1.,0.));
#30883=DIRECTION('ref_axis',(-1.,-1.95534159233113E-16,0.));
#30884=DIRECTION('',(-1.,-1.95534159233113E-16,0.));
#30885=DIRECTION('',(0.,0.,1.));
#30886=DIRECTION('center_axis',(0.707106781186534,0.707106781186561,0.));
#30887=DIRECTION('ref_axis',(-0.707106781186561,0.707106781186534,0.));
#30888=DIRECTION('',(-0.707106781186561,0.707106781186534,0.));
#30889=DIRECTION('',(0.,0.,1.));
#30890=DIRECTION('center_axis',(1.,0.,0.));
#30891=DIRECTION('ref_axis',(0.,0.,-1.));
#30892=DIRECTION('',(0.,1.,0.));
#30893=DIRECTION('',(0.,0.,1.));
#30894=DIRECTION('center_axis',(0.707106781186549,-0.707106781186546,0.));
#30895=DIRECTION('ref_axis',(0.707106781186546,0.707106781186549,0.));
#30896=DIRECTION('',(0.707106781186546,0.707106781186549,0.));
#30897=DIRECTION('',(0.,0.,1.));
#30898=DIRECTION('center_axis',(0.,-1.,0.));
#30899=DIRECTION('ref_axis',(0.,0.,-1.));
#30900=DIRECTION('',(1.,0.,0.));
#30901=DIRECTION('center_axis',(-1.30104260698261E-15,1.,-1.73611473352215E-31));
#30902=DIRECTION('ref_axis',(-1.,-1.30104260698261E-15,0.));
#30903=DIRECTION('center_axis',(-1.30104260698261E-15,1.,-1.73611473352215E-31));
#30904=DIRECTION('ref_axis',(-1.,-1.30104260698261E-15,0.));
#30905=DIRECTION('',(4.33680868994202E-17,0.,1.));
#30906=DIRECTION('center_axis',(-1.30104260698261E-15,1.,-1.73611473352215E-31));
#30907=DIRECTION('ref_axis',(-1.,-1.30104260698261E-15,2.25875923892257E-46));
#30908=DIRECTION('',(4.33680868994202E-17,0.,-1.));
#30909=DIRECTION('center_axis',(0.,0.,-1.));
#30910=DIRECTION('ref_axis',(-1.,0.,0.));
#30911=DIRECTION('',(1.,0.,0.));
#30912=DIRECTION('',(-1.73472347597681E-16,1.,0.));
#30913=DIRECTION('center_axis',(0.,0.,1.));
#30914=DIRECTION('ref_axis',(1.,0.,0.));
#30915=DIRECTION('',(-1.73472347597681E-16,-1.,0.));
#30916=DIRECTION('',(1.,0.,0.));
#30917=DIRECTION('',(0.707106781186562,0.707106781186533,0.));
#30918=DIRECTION('',(-1.26161707343768E-16,1.,0.));
#30919=DIRECTION('',(-0.707106781186547,0.707106781186548,0.));
#30920=DIRECTION('',(1.,0.,0.));
#30921=DIRECTION('',(0.707106781186546,0.707106781186549,0.));
#30922=DIRECTION('center_axis',(0.,0.,1.));
#30923=DIRECTION('ref_axis',(-1.,0.,0.));
#30924=DIRECTION('',(0.,1.,0.));
#30925=DIRECTION('center_axis',(0.,0.,1.));
#30926=DIRECTION('ref_axis',(-1.,0.,0.));
#30927=DIRECTION('',(-0.707106781186549,0.707106781186546,0.));
#30928=DIRECTION('center_axis',(0.,0.,-1.));
#30929=DIRECTION('ref_axis',(-1.,0.,0.));
#30930=DIRECTION('center_axis',(0.,0.,1.));
#30931=DIRECTION('ref_axis',(1.,0.,0.));
#30932=DIRECTION('center_axis',(0.,0.,-1.));
#30933=DIRECTION('ref_axis',(-1.,0.,0.));
#30934=DIRECTION('',(-0.707106781186549,0.707106781186546,0.));
#30935=DIRECTION('center_axis',(0.,0.,-1.));
#30936=DIRECTION('ref_axis',(-1.,0.,0.));
#30937=DIRECTION('',(0.,1.,0.));
#30938=DIRECTION('center_axis',(0.,0.,-1.));
#30939=DIRECTION('ref_axis',(-1.,0.,0.));
#30940=DIRECTION('',(0.707106781186546,0.707106781186549,0.));
#30941=DIRECTION('center_axis',(0.,0.,-1.));
#30942=DIRECTION('ref_axis',(-1.,0.,0.));
#30943=DIRECTION('center_axis',(0.,0.,1.));
#30944=DIRECTION('ref_axis',(1.,0.,0.));
#30945=DIRECTION('center_axis',(0.,0.,-1.));
#30946=DIRECTION('ref_axis',(-1.,0.,0.));
#30947=DIRECTION('',(0.707106781186546,0.707106781186549,0.));
#30948=DIRECTION('',(1.,1.22464679914735E-16,0.));
#30949=DIRECTION('',(0.707106781186546,-0.707106781186549,0.));
#30950=DIRECTION('center_axis',(0.,0.,-1.));
#30951=DIRECTION('ref_axis',(-1.,0.,0.));
#30952=DIRECTION('center_axis',(0.,0.,1.));
#30953=DIRECTION('ref_axis',(1.,0.,0.));
#30954=DIRECTION('center_axis',(0.,0.,-1.));
#30955=DIRECTION('ref_axis',(-1.,0.,0.));
#30956=DIRECTION('',(0.707106781186546,-0.707106781186549,0.));
#30957=DIRECTION('center_axis',(0.,0.,-1.));
#30958=DIRECTION('ref_axis',(-1.,0.,0.));
#30959=DIRECTION('',(0.,-1.,0.));
#30960=DIRECTION('center_axis',(0.,0.,-1.));
#30961=DIRECTION('ref_axis',(-1.,0.,0.));
#30962=DIRECTION('',(-0.707106781186549,-0.707106781186546,0.));
#30963=DIRECTION('center_axis',(0.,0.,-1.));
#30964=DIRECTION('ref_axis',(-1.,0.,0.));
#30965=DIRECTION('center_axis',(0.,0.,1.));
#30966=DIRECTION('ref_axis',(1.,0.,0.));
#30967=DIRECTION('center_axis',(0.,0.,-1.));
#30968=DIRECTION('ref_axis',(-1.,0.,0.));
#30969=DIRECTION('',(-0.707106781186549,-0.707106781186546,0.));
#30970=DIRECTION('center_axis',(0.,0.,1.));
#30971=DIRECTION('ref_axis',(-1.,-3.46944695195361E-15,0.));
#30972=DIRECTION('',(0.,-1.,0.));
#30973=DIRECTION('center_axis',(0.,0.,1.));
#30974=DIRECTION('ref_axis',(-1.,0.,0.));
#30975=DIRECTION('',(0.707106781186546,-0.707106781186549,0.));
#30976=DIRECTION('',(1.,-6.49101394191508E-16,0.));
#30977=DIRECTION('',(-0.707106781186547,-0.707106781186548,0.));
#30978=DIRECTION('',(-1.26161707343768E-16,-1.,0.));
#30979=DIRECTION('',(0.707106781186562,-0.707106781186533,0.));
#30980=DIRECTION('center_axis',(1.,1.30104260698261E-15,4.33680868994202E-17));
#30981=DIRECTION('ref_axis',(-1.30104260698261E-15,1.,5.08894400801554E-48));
#30982=DIRECTION('',(4.33680868994202E-17,0.,-1.));
#30983=DIRECTION('',(-1.30104260698261E-15,1.,-1.73611473352215E-31));
#30984=DIRECTION('center_axis',(-1.,-1.30104260698261E-15,4.33680868994202E-17));
#30985=DIRECTION('ref_axis',(1.30104260698261E-15,-1.,5.08894400801554E-48));
#30986=DIRECTION('',(4.33680868994202E-17,0.,1.));
#30987=DIRECTION('',(-1.30104260698261E-15,1.,-1.73611473352215E-31));
#30988=DIRECTION('center_axis',(-1.30104260698261E-15,1.,-1.73611473352215E-31));
#30989=DIRECTION('ref_axis',(-1.,-1.30104260698261E-15,2.25875923892257E-46));
#30990=DIRECTION('center_axis',(-1.30104260698261E-15,1.,-1.73611473352215E-31));
#30991=DIRECTION('ref_axis',(-1.,-1.30104260698261E-15,2.25875923892257E-46));
#30992=DIRECTION('center_axis',(-1.30104260698261E-15,1.,-1.73611473352215E-31));
#30993=DIRECTION('ref_axis',(-1.,-1.30104260698261E-15,0.));
#30994=DIRECTION('center_axis',(-1.30104260698261E-15,1.,-1.73611473352215E-31));
#30995=DIRECTION('ref_axis',(-1.,-1.30104260698261E-15,0.));
#30996=DIRECTION('',(-1.3010426069826E-16,0.,-1.));
#30997=DIRECTION('center_axis',(-1.30104260698261E-15,1.,-1.73611473352215E-31));
#30998=DIRECTION('ref_axis',(-1.,-1.30104260698261E-15,2.25875923892257E-46));
#30999=DIRECTION('',(1.3010426069826E-16,0.,1.));
#31000=DIRECTION('center_axis',(-6.49101394191508E-16,-1.,0.));
#31001=DIRECTION('ref_axis',(1.,-6.49101394191508E-16,0.));
#31002=DIRECTION('',(1.,-3.50803534070133E-16,0.));
#31003=DIRECTION('',(0.,0.,1.));
#31004=DIRECTION('',(0.,0.,1.));
#31005=DIRECTION('center_axis',(-0.707106781186548,0.707106781186547,0.));
#31006=DIRECTION('ref_axis',(-0.707106781186547,-0.707106781186548,0.));
#31007=DIRECTION('',(0.707106781186547,0.707106781186548,0.));
#31008=DIRECTION('',(0.,0.,1.));
#31009=DIRECTION('center_axis',(-1.,1.26161707343768E-16,0.));
#31010=DIRECTION('ref_axis',(-1.26161707343768E-16,-1.,0.));
#31011=DIRECTION('',(1.26161707343768E-16,1.,0.));
#31012=DIRECTION('',(0.,0.,1.));
#31013=DIRECTION('center_axis',(-0.707106781186533,-0.707106781186562,0.));
#31014=DIRECTION('ref_axis',(0.707106781186562,-0.707106781186533,0.));
#31015=DIRECTION('',(-0.707106781186562,0.707106781186533,0.));
#31016=DIRECTION('',(0.,0.,1.));
#31017=DIRECTION('center_axis',(0.,-1.,0.));
#31018=DIRECTION('ref_axis',(0.,0.,-1.));
#31019=DIRECTION('',(-1.,0.,0.));
#31020=DIRECTION('',(0.,0.,1.));
#31021=DIRECTION('',(-1.,0.,0.));
#31022=DIRECTION('',(0.,0.,1.));
#31023=DIRECTION('',(0.,0.,1.));
#31024=DIRECTION('center_axis',(0.707106781186533,-0.707106781186562,0.));
#31025=DIRECTION('ref_axis',(0.707106781186562,0.707106781186533,0.));
#31026=DIRECTION('',(-0.707106781186562,-0.707106781186533,0.));
#31027=DIRECTION('',(0.,0.,1.));
#31028=DIRECTION('center_axis',(1.,1.26161707343768E-16,0.));
#31029=DIRECTION('ref_axis',(-1.26161707343768E-16,1.,0.));
#31030=DIRECTION('',(1.26161707343768E-16,-1.,0.));
#31031=DIRECTION('',(0.,0.,1.));
#31032=DIRECTION('center_axis',(0.707106781186548,0.707106781186547,0.));
#31033=DIRECTION('ref_axis',(-0.707106781186547,0.707106781186548,0.));
#31034=DIRECTION('',(0.707106781186547,-0.707106781186548,0.));
#31035=DIRECTION('',(0.,0.,1.));
#31036=DIRECTION('center_axis',(0.,-1.,0.));
#31037=DIRECTION('ref_axis',(0.,0.,-1.));
#31038=DIRECTION('',(1.,0.,0.));
#31039=DIRECTION('',(0.,0.,1.));
#31040=DIRECTION('center_axis',(0.707106781186549,-0.707106781186546,0.));
#31041=DIRECTION('ref_axis',(0.707106781186546,0.707106781186549,0.));
#31042=DIRECTION('',(0.707106781186546,0.707106781186549,0.));
#31043=DIRECTION('',(0.,0.,1.));
#31044=DIRECTION('center_axis',(0.,0.,1.));
#31045=DIRECTION('ref_axis',(1.,0.,0.));
#31046=DIRECTION('center_axis',(0.,0.,1.));
#31047=DIRECTION('ref_axis',(1.,0.,0.));
#31048=DIRECTION('',(0.,0.,-1.));
#31049=DIRECTION('center_axis',(1.,0.,0.));
#31050=DIRECTION('ref_axis',(0.,0.,-1.));
#31051=DIRECTION('',(0.,1.,0.));
#31052=DIRECTION('',(0.,0.,1.));
#31053=DIRECTION('center_axis',(0.,0.,1.));
#31054=DIRECTION('ref_axis',(1.,0.,0.));
#31055=DIRECTION('center_axis',(0.,0.,1.));
#31056=DIRECTION('ref_axis',(1.,0.,0.));
#31057=DIRECTION('',(0.,0.,-1.));
#31058=DIRECTION('center_axis',(0.707106781186546,0.707106781186549,0.));
#31059=DIRECTION('ref_axis',(-0.707106781186549,0.707106781186546,0.));
#31060=DIRECTION('',(-0.707106781186549,0.707106781186546,0.));
#31061=DIRECTION('',(0.,0.,1.));
#31062=DIRECTION('center_axis',(0.,0.,1.));
#31063=DIRECTION('ref_axis',(1.,0.,0.));
#31064=DIRECTION('center_axis',(0.,0.,-1.));
#31065=DIRECTION('ref_axis',(1.,0.,0.));
#31066=DIRECTION('',(0.,0.,-1.));
#31067=DIRECTION('center_axis',(0.,0.,1.));
#31068=DIRECTION('ref_axis',(1.,0.,0.));
#31069=DIRECTION('center_axis',(0.,0.,1.));
#31070=DIRECTION('ref_axis',(1.,0.,0.));
#31071=DIRECTION('',(0.,0.,1.));
#31072=DIRECTION('center_axis',(0.,0.,1.));
#31073=DIRECTION('ref_axis',(1.,0.,0.));
#31074=DIRECTION('center_axis',(0.,0.,-1.));
#31075=DIRECTION('ref_axis',(1.,0.,0.));
#31076=DIRECTION('',(0.,0.,-1.));
#31077=DIRECTION('center_axis',(0.707106781186546,0.707106781186549,0.));
#31078=DIRECTION('ref_axis',(-0.707106781186549,0.707106781186546,0.));
#31079=DIRECTION('',(-0.707106781186548,0.707106781186547,0.));
#31080=DIRECTION('',(0.,0.,1.));
#31081=DIRECTION('center_axis',(0.,0.,-1.));
#31082=DIRECTION('ref_axis',(-1.,0.,0.));
#31083=DIRECTION('center_axis',(0.,0.,-1.));
#31084=DIRECTION('ref_axis',(1.,0.,0.));
#31085=DIRECTION('',(0.,0.,-1.));
#31086=DIRECTION('center_axis',(1.,0.,0.));
#31087=DIRECTION('ref_axis',(0.,0.,-1.));
#31088=DIRECTION('',(0.,1.,0.));
#31089=DIRECTION('',(0.,0.,1.));
#31090=DIRECTION('center_axis',(0.,0.,-1.));
#31091=DIRECTION('ref_axis',(-1.,0.,0.));
#31092=DIRECTION('center_axis',(0.,0.,-1.));
#31093=DIRECTION('ref_axis',(1.,0.,0.));
#31094=DIRECTION('',(0.,0.,-1.));
#31095=DIRECTION('center_axis',(0.707106781186549,-0.707106781186546,0.));
#31096=DIRECTION('ref_axis',(0.707106781186546,0.707106781186549,0.));
#31097=DIRECTION('',(0.707106781186545,0.70710678118655,0.));
#31098=DIRECTION('',(0.,0.,1.));
#31099=DIRECTION('center_axis',(0.,0.,1.));
#31100=DIRECTION('ref_axis',(1.,0.,0.));
#31101=DIRECTION('center_axis',(0.,0.,-1.));
#31102=DIRECTION('ref_axis',(1.,0.,0.));
#31103=DIRECTION('',(0.,0.,-1.));
#31104=DIRECTION('center_axis',(0.,0.,1.));
#31105=DIRECTION('ref_axis',(1.,0.,0.));
#31106=DIRECTION('center_axis',(0.,0.,1.));
#31107=DIRECTION('ref_axis',(1.,0.,0.));
#31108=DIRECTION('',(0.,0.,1.));
#31109=DIRECTION('center_axis',(0.,0.,1.));
#31110=DIRECTION('ref_axis',(1.,0.,0.));
#31111=DIRECTION('center_axis',(0.,0.,-1.));
#31112=DIRECTION('ref_axis',(1.,0.,0.));
#31113=DIRECTION('',(0.,0.,-1.));
#31114=DIRECTION('center_axis',(0.707106781186549,-0.707106781186546,0.));
#31115=DIRECTION('ref_axis',(0.707106781186546,0.707106781186549,0.));
#31116=DIRECTION('',(0.707106781186546,0.707106781186549,0.));
#31117=DIRECTION('',(0.,0.,1.));
#31118=DIRECTION('center_axis',(1.22464679914735E-16,-1.,0.));
#31119=DIRECTION('ref_axis',(1.,1.22464679914735E-16,0.));
#31120=DIRECTION('',(1.,1.22464679914735E-16,0.));
#31121=DIRECTION('',(0.,0.,1.));
#31122=DIRECTION('center_axis',(-0.707106781186549,-0.707106781186546,0.));
#31123=DIRECTION('ref_axis',(0.707106781186546,-0.707106781186549,0.));
#31124=DIRECTION('',(0.707106781186546,-0.707106781186549,0.));
#31125=DIRECTION('',(0.,0.,1.));
#31126=DIRECTION('center_axis',(0.,0.,1.));
#31127=DIRECTION('ref_axis',(1.,0.,0.));
#31128=DIRECTION('center_axis',(0.,0.,-1.));
#31129=DIRECTION('ref_axis',(1.,0.,0.));
#31130=DIRECTION('',(0.,0.,-1.));
#31131=DIRECTION('center_axis',(0.,0.,1.));
#31132=DIRECTION('ref_axis',(1.,0.,0.));
#31133=DIRECTION('center_axis',(0.,0.,1.));
#31134=DIRECTION('ref_axis',(1.,0.,0.));
#31135=DIRECTION('',(0.,0.,1.));
#31136=DIRECTION('center_axis',(0.,0.,1.));
#31137=DIRECTION('ref_axis',(1.,0.,0.));
#31138=DIRECTION('center_axis',(0.,0.,-1.));
#31139=DIRECTION('ref_axis',(1.,0.,0.));
#31140=DIRECTION('',(0.,0.,-1.));
#31141=DIRECTION('center_axis',(-0.707106781186549,-0.707106781186546,0.));
#31142=DIRECTION('ref_axis',(0.707106781186546,-0.707106781186549,0.));
#31143=DIRECTION('',(0.707106781186545,-0.70710678118655,0.));
#31144=DIRECTION('',(0.,0.,1.));
#31145=DIRECTION('center_axis',(0.,0.,-1.));
#31146=DIRECTION('ref_axis',(-1.,0.,0.));
#31147=DIRECTION('center_axis',(0.,0.,-1.));
#31148=DIRECTION('ref_axis',(1.,0.,0.));
#31149=DIRECTION('',(0.,0.,-1.));
#31150=DIRECTION('center_axis',(-1.,0.,0.));
#31151=DIRECTION('ref_axis',(0.,0.,1.));
#31152=DIRECTION('',(0.,-1.,0.));
#31153=DIRECTION('',(0.,0.,1.));
#31154=DIRECTION('center_axis',(0.,0.,-1.));
#31155=DIRECTION('ref_axis',(-1.,0.,0.));
#31156=DIRECTION('center_axis',(0.,0.,-1.));
#31157=DIRECTION('ref_axis',(1.,0.,0.));
#31158=DIRECTION('',(0.,0.,-1.));
#31159=DIRECTION('center_axis',(-0.707106781186546,0.707106781186549,0.));
#31160=DIRECTION('ref_axis',(-0.707106781186549,-0.707106781186546,0.));
#31161=DIRECTION('',(-0.707106781186548,-0.707106781186547,0.));
#31162=DIRECTION('',(0.,0.,1.));
#31163=DIRECTION('center_axis',(0.,0.,1.));
#31164=DIRECTION('ref_axis',(1.,0.,0.));
#31165=DIRECTION('center_axis',(0.,0.,-1.));
#31166=DIRECTION('ref_axis',(1.,0.,0.));
#31167=DIRECTION('',(0.,0.,-1.));
#31168=DIRECTION('center_axis',(0.,0.,1.));
#31169=DIRECTION('ref_axis',(1.,0.,0.));
#31170=DIRECTION('center_axis',(0.,0.,1.));
#31171=DIRECTION('ref_axis',(1.,0.,0.));
#31172=DIRECTION('',(0.,0.,1.));
#31173=DIRECTION('center_axis',(0.,0.,1.));
#31174=DIRECTION('ref_axis',(1.,0.,0.));
#31175=DIRECTION('center_axis',(0.,0.,-1.));
#31176=DIRECTION('ref_axis',(1.,0.,0.));
#31177=DIRECTION('',(0.,0.,-1.));
#31178=DIRECTION('center_axis',(-0.707106781186546,0.707106781186549,0.));
#31179=DIRECTION('ref_axis',(-0.707106781186549,-0.707106781186546,0.));
#31180=DIRECTION('',(-0.707106781186549,-0.707106781186546,0.));
#31181=DIRECTION('',(0.,0.,1.));
#31182=DIRECTION('center_axis',(0.,0.,1.));
#31183=DIRECTION('ref_axis',(1.,0.,0.));
#31184=DIRECTION('center_axis',(0.,0.,1.));
#31185=DIRECTION('ref_axis',(1.,0.,0.));
#31186=DIRECTION('',(0.,0.,-1.));
#31187=DIRECTION('center_axis',(-1.,0.,0.));
#31188=DIRECTION('ref_axis',(0.,0.,1.));
#31189=DIRECTION('',(0.,-1.,0.));
#31190=DIRECTION('',(0.,0.,1.));
#31191=DIRECTION('center_axis',(0.,0.,1.));
#31192=DIRECTION('ref_axis',(1.,0.,0.));
#31193=DIRECTION('center_axis',(0.,0.,1.));
#31194=DIRECTION('ref_axis',(1.,0.,0.));
#31195=DIRECTION('',(0.,0.,-1.));
#31196=DIRECTION('center_axis',(-0.707106781186549,-0.707106781186546,0.));
#31197=DIRECTION('ref_axis',(0.707106781186546,-0.707106781186549,0.));
#31198=DIRECTION('',(0.707106781186546,-0.707106781186549,0.));
#31199=DIRECTION('center_axis',(-1.30104260698261E-15,1.,-1.73611473352215E-31));
#31200=DIRECTION('ref_axis',(-1.,-1.30104260698261E-15,0.));
#31201=DIRECTION('center_axis',(-7.96355992932556E-18,-1.,0.));
#31202=DIRECTION('ref_axis',(1.,-7.96355992932556E-18,0.));
#31203=DIRECTION('',(0.,0.,1.));
#31204=DIRECTION('',(-1.,7.96355992932556E-18,0.));
#31205=DIRECTION('',(0.,0.,-1.));
#31206=DIRECTION('',(1.,-7.96355992932556E-18,0.));
#31207=DIRECTION('center_axis',(4.11015771401436E-16,-1.,0.));
#31208=DIRECTION('ref_axis',(1.,4.11015771401436E-16,0.));
#31209=DIRECTION('',(0.,0.,1.));
#31210=DIRECTION('',(-1.,-4.11015771401436E-16,0.));
#31211=DIRECTION('',(0.,0.,-1.));
#31212=DIRECTION('',(-1.,-4.11015771401436E-16,0.));
#31213=DIRECTION('center_axis',(-1.,-1.30104260698261E-15,1.3010426069826E-16));
#31214=DIRECTION('ref_axis',(1.30104260698261E-15,-1.,-3.07902494602621E-48));
#31215=DIRECTION('',(1.3010426069826E-16,0.,1.));
#31216=DIRECTION('',(-1.30104260698261E-15,1.,-1.73611473352215E-31));
#31217=DIRECTION('center_axis',(1.,1.30104260698261E-15,-1.3010426069826E-16));
#31218=DIRECTION('ref_axis',(-1.30104260698261E-15,1.,3.07902494602621E-48));
#31219=DIRECTION('',(-1.3010426069826E-16,0.,-1.));
#31220=DIRECTION('',(-1.30104260698261E-15,1.,-1.73611473352215E-31));
#31221=DIRECTION('center_axis',(-1.30104260698261E-15,1.,-1.73611473352215E-31));
#31222=DIRECTION('ref_axis',(-1.,-1.30104260698261E-15,2.25875923892257E-46));
#31223=DIRECTION('center_axis',(-1.30104260698261E-15,1.,-1.73611473352215E-31));
#31224=DIRECTION('ref_axis',(-1.,-1.30104260698261E-15,2.25875923892257E-46));
#31225=DIRECTION('center_axis',(0.,0.,-1.));
#31226=DIRECTION('ref_axis',(-1.,0.,0.));
#31227=DIRECTION('center_axis',(0.,0.,-1.));
#31228=DIRECTION('ref_axis',(1.,0.,0.));
#31229=DIRECTION('center_axis',(0.,0.,1.));
#31230=DIRECTION('ref_axis',(-1.,-1.73472347597681E-15,0.));
#31231=DIRECTION('',(0.,0.,-1.));
#31232=DIRECTION('center_axis',(0.,0.,1.));
#31233=DIRECTION('ref_axis',(1.,0.,0.));
#31234=DIRECTION('',(-0.258819045102518,0.965925826289069,0.));
#31235=DIRECTION('',(2.04085114820801E-16,1.,0.));
#31236=DIRECTION('',(-1.,1.2823896663807E-16,0.));
#31237=DIRECTION('',(-0.707106781186548,0.707106781186547,0.));
#31238=DIRECTION('center_axis',(1.,-2.04085114820801E-16,0.));
#31239=DIRECTION('ref_axis',(2.04085114820801E-16,1.,0.));
#31240=DIRECTION('',(0.,0.,1.));
#31241=DIRECTION('',(0.,1.,0.));
#31242=DIRECTION('',(0.,0.,1.));
#31243=DIRECTION('center_axis',(-1.,-2.04085114820801E-16,0.));
#31244=DIRECTION('ref_axis',(2.04085114820801E-16,-1.,0.));
#31245=DIRECTION('',(0.,0.,1.));
#31246=DIRECTION('',(0.,-1.,0.));
#31247=DIRECTION('',(0.,0.,-1.));
#31248=DIRECTION('',(2.04085114820801E-16,-1.,0.));
#31249=DIRECTION('center_axis',(0.,0.,1.));
#31250=DIRECTION('ref_axis',(1.,0.,0.));
#31251=DIRECTION('',(-0.258819045102518,-0.965925826289069,0.));
#31252=DIRECTION('center_axis',(0.,0.,-1.));
#31253=DIRECTION('ref_axis',(1.,-1.73472347597681E-15,0.));
#31254=DIRECTION('',(-0.707106781186557,-0.707106781186538,0.));
#31255=DIRECTION('',(-1.,-1.2823896663807E-16,0.));
#31256=DIRECTION('center_axis',(0.,0.,-1.));
#31257=DIRECTION('ref_axis',(-1.,0.,0.));
#31258=DIRECTION('',(0.,0.,1.));
#31259=DIRECTION('center_axis',(0.,0.,-1.));
#31260=DIRECTION('ref_axis',(1.,0.,0.));
#31261=DIRECTION('center_axis',(0.,0.,1.));
#31262=DIRECTION('ref_axis',(1.,0.,0.));
#31263=DIRECTION('',(1.,0.,0.));
#31264=DIRECTION('',(0.707106781186546,0.707106781186549,0.));
#31265=DIRECTION('',(0.,1.,0.));
#31266=DIRECTION('',(-0.707106781186561,0.707106781186534,0.));
#31267=DIRECTION('',(-1.,-1.95534159233113E-16,0.));
#31268=DIRECTION('',(-0.707106781186562,-0.707106781186533,0.));
#31269=DIRECTION('',(1.26352022694434E-16,-1.,0.));
#31270=DIRECTION('',(0.707106781186547,-0.707106781186548,0.));
#31271=DIRECTION('',(1.,0.,0.));
#31272=DIRECTION('',(0.707106781186546,0.707106781186549,0.));
#31273=DIRECTION('center_axis',(0.,0.,1.));
#31274=DIRECTION('ref_axis',(1.,0.,0.));
#31275=DIRECTION('',(0.,1.,0.));
#31276=DIRECTION('center_axis',(0.,0.,1.));
#31277=DIRECTION('ref_axis',(1.,0.,0.));
#31278=DIRECTION('',(-0.707106781186552,0.707106781186543,0.));
#31279=DIRECTION('center_axis',(0.,0.,-1.));
#31280=DIRECTION('ref_axis',(1.,0.,0.));
#31281=DIRECTION('center_axis',(0.,0.,1.));
#31282=DIRECTION('ref_axis',(1.,0.,0.));
#31283=DIRECTION('center_axis',(0.,0.,-1.));
#31284=DIRECTION('ref_axis',(1.,0.,0.));
#31285=DIRECTION('',(-0.707106781186546,0.707106781186549,0.));
#31286=DIRECTION('center_axis',(0.,0.,-1.));
#31287=DIRECTION('ref_axis',(1.,0.,0.));
#31288=DIRECTION('',(0.,1.,0.));
#31289=DIRECTION('center_axis',(0.,0.,-1.));
#31290=DIRECTION('ref_axis',(1.,0.,0.));
#31291=DIRECTION('',(0.707106781186546,0.707106781186549,0.));
#31292=DIRECTION('center_axis',(0.,0.,-1.));
#31293=DIRECTION('ref_axis',(1.,0.,0.));
#31294=DIRECTION('center_axis',(0.,0.,1.));
#31295=DIRECTION('ref_axis',(1.,0.,0.));
#31296=DIRECTION('center_axis',(0.,0.,-1.));
#31297=DIRECTION('ref_axis',(1.,0.,0.));
#31298=DIRECTION('',(0.707106781186547,0.707106781186548,0.));
#31299=DIRECTION('',(1.,4.61786466713945E-17,0.));
#31300=DIRECTION('',(0.707106781186546,-0.707106781186549,0.));
#31301=DIRECTION('center_axis',(0.,0.,-1.));
#31302=DIRECTION('ref_axis',(1.,0.,0.));
#31303=DIRECTION('center_axis',(0.,0.,1.));
#31304=DIRECTION('ref_axis',(1.,0.,0.));
#31305=DIRECTION('center_axis',(0.,0.,-1.));
#31306=DIRECTION('ref_axis',(1.,0.,0.));
#31307=DIRECTION('',(0.707106781186547,-0.707106781186547,0.));
#31308=DIRECTION('center_axis',(0.,0.,-1.));
#31309=DIRECTION('ref_axis',(1.,0.,0.));
#31310=DIRECTION('',(0.,-1.,0.));
#31311=DIRECTION('center_axis',(0.,0.,-1.));
#31312=DIRECTION('ref_axis',(1.,0.,0.));
#31313=DIRECTION('',(-0.707106781186552,-0.707106781186543,0.));
#31314=DIRECTION('center_axis',(0.,0.,-1.));
#31315=DIRECTION('ref_axis',(1.,0.,0.));
#31316=DIRECTION('center_axis',(0.,0.,1.));
#31317=DIRECTION('ref_axis',(1.,0.,0.));
#31318=DIRECTION('center_axis',(0.,0.,-1.));
#31319=DIRECTION('ref_axis',(1.,0.,0.));
#31320=DIRECTION('',(-0.707106781186552,-0.707106781186543,0.));
#31321=DIRECTION('center_axis',(0.,0.,1.));
#31322=DIRECTION('ref_axis',(1.,0.,0.));
#31323=DIRECTION('',(0.,-1.,0.));
#31324=DIRECTION('center_axis',(0.,0.,1.));
#31325=DIRECTION('ref_axis',(1.,0.,0.));
#31326=DIRECTION('',(0.707106781186546,-0.707106781186549,0.));
#31327=DIRECTION('center_axis',(-0.707106781186538,0.707106781186557,0.));
#31328=DIRECTION('ref_axis',(0.,0.,1.));
#31329=DIRECTION('',(0.,0.,-1.));
#31330=DIRECTION('',(-0.707106781186557,-0.707106781186538,0.));
#31331=DIRECTION('center_axis',(0.707106781186547,0.707106781186548,0.));
#31332=DIRECTION('ref_axis',(0.,0.,1.));
#31333=DIRECTION('',(0.,0.,1.));
#31334=DIRECTION('',(0.707106781186548,-0.707106781186547,0.));
#31335=DIRECTION('center_axis',(0.,0.,-1.));
#31336=DIRECTION('ref_axis',(-1.,0.,0.));
#31337=DIRECTION('',(-2.04085114820801E-16,-1.,0.));
#31338=DIRECTION('',(0.258819045102518,-0.965925826289069,0.));
#31339=DIRECTION('',(1.,-1.2823896663807E-16,0.));
#31340=DIRECTION('center_axis',(1.,-2.04085114820801E-16,0.));
#31341=DIRECTION('ref_axis',(2.04085114820801E-16,1.,0.));
#31342=DIRECTION('',(0.,0.,-1.));
#31343=DIRECTION('',(0.,-1.,0.));
#31344=DIRECTION('',(0.,0.,1.));
#31345=DIRECTION('center_axis',(0.,0.,1.));
#31346=DIRECTION('ref_axis',(1.,0.,0.));
#31347=DIRECTION('',(1.,1.2823896663807E-16,0.));
#31348=DIRECTION('',(-0.258819045102518,-0.965925826289069,0.));
#31349=DIRECTION('',(-2.04085114820801E-16,1.,0.));
#31350=DIRECTION('center_axis',(-1.,-2.04085114820801E-16,0.));
#31351=DIRECTION('ref_axis',(2.04085114820801E-16,-1.,0.));
#31352=DIRECTION('',(0.,0.,-1.));
#31353=DIRECTION('',(0.,1.,0.));
#31354=DIRECTION('',(0.,0.,-1.));
#31355=DIRECTION('center_axis',(-1.30104260698261E-15,1.,-1.73611473352215E-31));
#31356=DIRECTION('ref_axis',(-1.,-1.30104260698261E-15,0.));
#31357=DIRECTION('center_axis',(-0.965925826289069,-0.258819045102518,0.));
#31358=DIRECTION('ref_axis',(0.258819045102518,-0.965925826289069,0.));
#31359=DIRECTION('center_axis',(-0.965925826289069,-0.258819045102518,0.));
#31360=DIRECTION('ref_axis',(0.258819045102518,-0.965925826289069,0.));
#31361=DIRECTION('center_axis',(-0.965925826289069,-0.258819045102518,0.));
#31362=DIRECTION('ref_axis',(0.258819045102518,-0.965925826289069,0.));
#31363=DIRECTION('center_axis',(-1.2823896663807E-16,1.,0.));
#31364=DIRECTION('ref_axis',(-1.,-1.2823896663807E-16,0.));
#31365=DIRECTION('center_axis',(-1.2823896663807E-16,-1.,0.));
#31366=DIRECTION('ref_axis',(-1.,1.2823896663807E-16,0.));
#31367=DIRECTION('',(0.,0.,-1.));
#31368=DIRECTION('',(-1.,-1.2823896663807E-16,0.));
#31369=DIRECTION('',(0.,0.,1.));
#31370=DIRECTION('center_axis',(-1.,-2.04085114820801E-16,0.));
#31371=DIRECTION('ref_axis',(2.04085114820801E-16,-1.,0.));
#31372=DIRECTION('',(0.,0.,-1.));
#31373=DIRECTION('',(0.,1.,0.));
#31374=DIRECTION('',(2.04085114820801E-16,-1.,0.));
#31375=DIRECTION('center_axis',(-0.965925826289069,-0.258819045102518,0.));
#31376=DIRECTION('ref_axis',(0.258819045102518,-0.965925826289069,0.));
#31377=DIRECTION('center_axis',(-0.965925826289069,-0.258819045102518,0.));
#31378=DIRECTION('ref_axis',(0.258819045102518,-0.965925826289069,0.));
#31379=DIRECTION('',(0.258819045102518,-0.965925826289069,0.));
#31380=DIRECTION('',(0.,0.,1.));
#31381=DIRECTION('center_axis',(1.,-2.04085114820801E-16,0.));
#31382=DIRECTION('ref_axis',(2.04085114820801E-16,1.,0.));
#31383=DIRECTION('',(0.,0.,1.));
#31384=DIRECTION('',(0.,-1.,0.));
#31385=DIRECTION('',(2.04085114820801E-16,1.,0.));
#31386=DIRECTION('center_axis',(1.2823896663807E-16,1.,0.));
#31387=DIRECTION('ref_axis',(-1.,1.2823896663807E-16,0.));
#31388=DIRECTION('',(-1.,1.2823896663807E-16,0.));
#31389=DIRECTION('',(0.,0.,1.));
#31390=DIRECTION('center_axis',(-1.2823896663807E-16,-1.,0.));
#31391=DIRECTION('ref_axis',(-1.,1.2823896663807E-16,0.));
#31392=DIRECTION('center_axis',(0.965925826289069,-0.258819045102518,0.));
#31393=DIRECTION('ref_axis',(0.258819045102518,0.965925826289069,0.));
#31394=DIRECTION('center_axis',(0.965925826289069,-0.258819045102518,0.));
#31395=DIRECTION('ref_axis',(0.258819045102518,0.965925826289069,0.));
#31396=DIRECTION('',(0.258819045102518,0.965925826289069,0.));
#31397=DIRECTION('',(0.,0.,1.));
#31398=DIRECTION('center_axis',(0.965925826289069,-0.258819045102518,0.));
#31399=DIRECTION('ref_axis',(0.258819045102518,0.965925826289069,0.));
#31400=DIRECTION('center_axis',(0.965925826289069,-0.258819045102518,0.));
#31401=DIRECTION('ref_axis',(0.258819045102518,0.965925826289069,0.));
#31402=DIRECTION('center_axis',(0.965925826289069,-0.258819045102518,0.));
#31403=DIRECTION('ref_axis',(0.258819045102518,0.965925826289069,0.));
#31404=DIRECTION('center_axis',(0.,1.,0.));
#31405=DIRECTION('ref_axis',(0.,0.,1.));
#31406=DIRECTION('',(1.,0.,0.));
#31407=DIRECTION('',(0.,0.,-1.));
#31408=DIRECTION('',(0.,0.,-1.));
#31409=DIRECTION('center_axis',(-0.707106781186549,0.707106781186546,0.));
#31410=DIRECTION('ref_axis',(-0.707106781186546,-0.707106781186549,0.));
#31411=DIRECTION('',(0.707106781186546,0.707106781186549,0.));
#31412=DIRECTION('',(0.,0.,-1.));
#31413=DIRECTION('center_axis',(-1.,0.,0.));
#31414=DIRECTION('ref_axis',(0.,0.,1.));
#31415=DIRECTION('',(0.,1.,0.));
#31416=DIRECTION('',(0.,0.,-1.));
#31417=DIRECTION('center_axis',(-0.707106781186534,-0.707106781186561,0.));
#31418=DIRECTION('ref_axis',(0.707106781186561,-0.707106781186534,0.));
#31419=DIRECTION('',(-0.707106781186561,0.707106781186534,0.));
#31420=DIRECTION('',(0.,0.,-1.));
#31421=DIRECTION('center_axis',(1.95534159233113E-16,-1.,0.));
#31422=DIRECTION('ref_axis',(1.,1.95534159233113E-16,0.));
#31423=DIRECTION('',(-1.,-1.95534159233113E-16,0.));
#31424=DIRECTION('',(0.,0.,-1.));
#31425=DIRECTION('center_axis',(0.707106781186533,-0.707106781186562,0.));
#31426=DIRECTION('ref_axis',(0.707106781186562,0.707106781186533,0.));
#31427=DIRECTION('',(-0.707106781186562,-0.707106781186533,0.));
#31428=DIRECTION('',(0.,0.,-1.));
#31429=DIRECTION('center_axis',(1.,1.26352022694434E-16,0.));
#31430=DIRECTION('ref_axis',(-1.26352022694434E-16,1.,0.));
#31431=DIRECTION('',(1.26352022694434E-16,-1.,0.));
#31432=DIRECTION('',(0.,0.,-1.));
#31433=DIRECTION('center_axis',(0.707106781186548,0.707106781186547,0.));
#31434=DIRECTION('ref_axis',(-0.707106781186547,0.707106781186548,0.));
#31435=DIRECTION('',(0.707106781186547,-0.707106781186548,0.));
#31436=DIRECTION('',(0.,0.,-1.));
#31437=DIRECTION('center_axis',(0.,1.,0.));
#31438=DIRECTION('ref_axis',(0.,0.,1.));
#31439=DIRECTION('',(1.,0.,0.));
#31440=DIRECTION('',(0.,0.,-1.));
#31441=DIRECTION('center_axis',(-0.707106781186549,0.707106781186546,0.));
#31442=DIRECTION('ref_axis',(-0.707106781186546,-0.707106781186549,0.));
#31443=DIRECTION('',(0.707106781186546,0.707106781186549,0.));
#31444=DIRECTION('',(0.,0.,-1.));
#31445=DIRECTION('center_axis',(0.,0.,-1.));
#31446=DIRECTION('ref_axis',(-1.,0.,0.));
#31447=DIRECTION('center_axis',(0.,0.,1.));
#31448=DIRECTION('ref_axis',(1.,0.,0.));
#31449=DIRECTION('',(0.,0.,-1.));
#31450=DIRECTION('center_axis',(-1.,0.,0.));
#31451=DIRECTION('ref_axis',(0.,0.,1.));
#31452=DIRECTION('',(0.,1.,0.));
#31453=DIRECTION('',(0.,0.,-1.));
#31454=DIRECTION('center_axis',(0.,0.,-1.));
#31455=DIRECTION('ref_axis',(-1.,0.,0.));
#31456=DIRECTION('center_axis',(0.,0.,1.));
#31457=DIRECTION('ref_axis',(1.,0.,0.));
#31458=DIRECTION('',(0.,0.,-1.));
#31459=DIRECTION('center_axis',(-0.707106781186543,-0.707106781186552,0.));
#31460=DIRECTION('ref_axis',(0.707106781186553,-0.707106781186543,0.));
#31461=DIRECTION('',(-0.707106781186552,0.707106781186543,0.));
#31462=DIRECTION('',(0.,0.,-1.));
#31463=DIRECTION('center_axis',(0.,0.,-1.));
#31464=DIRECTION('ref_axis',(-1.,0.,0.));
#31465=DIRECTION('center_axis',(0.,0.,-1.));
#31466=DIRECTION('ref_axis',(1.,0.,0.));
#31467=DIRECTION('',(0.,0.,-1.));
#31468=DIRECTION('center_axis',(0.,0.,-1.));
#31469=DIRECTION('ref_axis',(-1.,0.,0.));
#31470=DIRECTION('center_axis',(0.,0.,1.));
#31471=DIRECTION('ref_axis',(1.,0.,0.));
#31472=DIRECTION('',(0.,0.,-1.));
#31473=DIRECTION('center_axis',(0.,0.,-1.));
#31474=DIRECTION('ref_axis',(-1.,0.,0.));
#31475=DIRECTION('center_axis',(0.,0.,-1.));
#31476=DIRECTION('ref_axis',(1.,0.,0.));
#31477=DIRECTION('',(0.,0.,-1.));
#31478=DIRECTION('center_axis',(-0.707106781186549,-0.707106781186546,0.));
#31479=DIRECTION('ref_axis',(0.707106781186546,-0.707106781186549,0.));
#31480=DIRECTION('',(-0.707106781186546,0.707106781186549,0.));
#31481=DIRECTION('',(0.,0.,-1.));
#31482=DIRECTION('center_axis',(0.,0.,-1.));
#31483=DIRECTION('ref_axis',(-1.,0.,0.));
#31484=DIRECTION('center_axis',(0.,0.,-1.));
#31485=DIRECTION('ref_axis',(1.,0.,0.));
#31486=DIRECTION('',(0.,0.,-1.));
#31487=DIRECTION('center_axis',(-1.,0.,0.));
#31488=DIRECTION('ref_axis',(0.,0.,1.));
#31489=DIRECTION('',(0.,1.,0.));
#31490=DIRECTION('',(0.,0.,-1.));
#31491=DIRECTION('center_axis',(0.,0.,-1.));
#31492=DIRECTION('ref_axis',(-1.,0.,0.));
#31493=DIRECTION('center_axis',(0.,0.,-1.));
#31494=DIRECTION('ref_axis',(1.,0.,0.));
#31495=DIRECTION('',(0.,0.,-1.));
#31496=DIRECTION('center_axis',(-0.70710678118655,0.707106781186545,0.));
#31497=DIRECTION('ref_axis',(-0.707106781186545,-0.70710678118655,0.));
#31498=DIRECTION('',(0.707106781186546,0.707106781186549,0.));
#31499=DIRECTION('',(0.,0.,-1.));
#31500=DIRECTION('center_axis',(0.,0.,-1.));
#31501=DIRECTION('ref_axis',(-1.,0.,0.));
#31502=DIRECTION('center_axis',(0.,0.,-1.));
#31503=DIRECTION('ref_axis',(1.,0.,0.));
#31504=DIRECTION('',(0.,0.,-1.));
#31505=DIRECTION('center_axis',(0.,0.,-1.));
#31506=DIRECTION('ref_axis',(-1.,0.,0.));
#31507=DIRECTION('center_axis',(0.,0.,1.));
#31508=DIRECTION('ref_axis',(1.,0.,0.));
#31509=DIRECTION('',(0.,0.,-1.));
#31510=DIRECTION('center_axis',(0.,0.,-1.));
#31511=DIRECTION('ref_axis',(-1.,0.,0.));
#31512=DIRECTION('center_axis',(0.,0.,-1.));
#31513=DIRECTION('ref_axis',(1.,0.,0.));
#31514=DIRECTION('',(0.,0.,-1.));
#31515=DIRECTION('center_axis',(-0.707106781186548,0.707106781186547,0.));
#31516=DIRECTION('ref_axis',(-0.707106781186547,-0.707106781186548,0.));
#31517=DIRECTION('',(0.707106781186547,0.707106781186548,0.));
#31518=DIRECTION('',(0.,0.,-1.));
#31519=DIRECTION('center_axis',(-4.61786466713945E-17,1.,0.));
#31520=DIRECTION('ref_axis',(-1.,-4.61786466713945E-17,0.));
#31521=DIRECTION('',(1.,4.61786466713945E-17,0.));
#31522=DIRECTION('',(0.,0.,-1.));
#31523=DIRECTION('center_axis',(0.707106781186549,0.707106781186546,0.));
#31524=DIRECTION('ref_axis',(-0.707106781186546,0.707106781186549,0.));
#31525=DIRECTION('',(0.707106781186546,-0.707106781186549,0.));
#31526=DIRECTION('',(0.,0.,-1.));
#31527=DIRECTION('center_axis',(0.,0.,-1.));
#31528=DIRECTION('ref_axis',(-1.,0.,0.));
#31529=DIRECTION('center_axis',(0.,0.,-1.));
#31530=DIRECTION('ref_axis',(1.,0.,0.));
#31531=DIRECTION('',(0.,0.,-1.));
#31532=DIRECTION('center_axis',(0.,0.,-1.));
#31533=DIRECTION('ref_axis',(-1.,0.,0.));
#31534=DIRECTION('center_axis',(0.,0.,1.));
#31535=DIRECTION('ref_axis',(1.,0.,0.));
#31536=DIRECTION('',(0.,0.,-1.));
#31537=DIRECTION('center_axis',(0.,0.,-1.));
#31538=DIRECTION('ref_axis',(-1.,0.,0.));
#31539=DIRECTION('center_axis',(0.,0.,-1.));
#31540=DIRECTION('ref_axis',(1.,0.,0.));
#31541=DIRECTION('',(0.,0.,-1.));
#31542=DIRECTION('center_axis',(0.707106781186548,0.707106781186548,0.));
#31543=DIRECTION('ref_axis',(-0.707106781186548,0.707106781186548,0.));
#31544=DIRECTION('',(0.707106781186547,-0.707106781186547,0.));
#31545=DIRECTION('',(0.,0.,-1.));
#31546=DIRECTION('center_axis',(0.,0.,-1.));
#31547=DIRECTION('ref_axis',(-1.,0.,0.));
#31548=DIRECTION('center_axis',(0.,0.,-1.));
#31549=DIRECTION('ref_axis',(1.,0.,0.));
#31550=DIRECTION('',(0.,0.,-1.));
#31551=DIRECTION('center_axis',(1.,0.,0.));
#31552=DIRECTION('ref_axis',(0.,0.,-1.));
#31553=DIRECTION('',(0.,-1.,0.));
#31554=DIRECTION('',(0.,0.,-1.));
#31555=DIRECTION('center_axis',(0.,0.,-1.));
#31556=DIRECTION('ref_axis',(-1.,0.,0.));
#31557=DIRECTION('center_axis',(0.,0.,-1.));
#31558=DIRECTION('ref_axis',(1.,0.,0.));
#31559=DIRECTION('',(0.,0.,-1.));
#31560=DIRECTION('center_axis',(0.707106781186543,-0.707106781186552,0.));
#31561=DIRECTION('ref_axis',(0.707106781186552,0.707106781186543,0.));
#31562=DIRECTION('',(-0.707106781186552,-0.707106781186543,0.));
#31563=DIRECTION('',(0.,0.,-1.));
#31564=DIRECTION('center_axis',(0.,0.,-1.));
#31565=DIRECTION('ref_axis',(-1.,0.,0.));
#31566=DIRECTION('center_axis',(0.,0.,-1.));
#31567=DIRECTION('ref_axis',(1.,0.,0.));
#31568=DIRECTION('',(0.,0.,-1.));
#31569=DIRECTION('center_axis',(0.,0.,-1.));
#31570=DIRECTION('ref_axis',(-1.,0.,0.));
#31571=DIRECTION('center_axis',(0.,0.,1.));
#31572=DIRECTION('ref_axis',(1.,0.,0.));
#31573=DIRECTION('',(0.,0.,-1.));
#31574=DIRECTION('center_axis',(0.,0.,-1.));
#31575=DIRECTION('ref_axis',(-1.,0.,0.));
#31576=DIRECTION('center_axis',(0.,0.,-1.));
#31577=DIRECTION('ref_axis',(1.,0.,0.));
#31578=DIRECTION('',(0.,0.,-1.));
#31579=DIRECTION('center_axis',(0.707106781186543,-0.707106781186552,0.));
#31580=DIRECTION('ref_axis',(0.707106781186552,0.707106781186543,0.));
#31581=DIRECTION('',(-0.707106781186552,-0.707106781186543,0.));
#31582=DIRECTION('',(0.,0.,-1.));
#31583=DIRECTION('center_axis',(0.,0.,-1.));
#31584=DIRECTION('ref_axis',(-1.,0.,0.));
#31585=DIRECTION('center_axis',(0.,0.,1.));
#31586=DIRECTION('ref_axis',(1.,0.,0.));
#31587=DIRECTION('',(0.,0.,-1.));
#31588=DIRECTION('center_axis',(1.,0.,0.));
#31589=DIRECTION('ref_axis',(0.,0.,-1.));
#31590=DIRECTION('',(0.,-1.,0.));
#31591=DIRECTION('',(0.,0.,-1.));
#31592=DIRECTION('center_axis',(0.,0.,-1.));
#31593=DIRECTION('ref_axis',(-1.,0.,0.));
#31594=DIRECTION('center_axis',(0.,0.,1.));
#31595=DIRECTION('ref_axis',(1.,0.,0.));
#31596=DIRECTION('',(0.,0.,-1.));
#31597=DIRECTION('center_axis',(0.707106781186549,0.707106781186546,0.));
#31598=DIRECTION('ref_axis',(-0.707106781186546,0.707106781186549,0.));
#31599=DIRECTION('',(0.707106781186546,-0.707106781186549,0.));
#31600=DIRECTION('center_axis',(-1.19636101791504E-15,1.,-1.04815936541451E-31));
#31601=DIRECTION('ref_axis',(-1.,-1.19636101791504E-15,0.));
#31602=DIRECTION('',(1.,1.19636101791504E-15,3.7386281809845E-17));
#31603=DIRECTION('',(-4.38061483832527E-16,-6.28895619248706E-31,-1.));
#31604=DIRECTION('',(-1.,-1.19636101791504E-15,0.));
#31605=DIRECTION('',(-8.76122967665054E-17,0.,1.));
#31606=DIRECTION('center_axis',(0.707106781186554,0.707106781186541,-3.09756245794624E-16));
#31607=DIRECTION('ref_axis',(4.38061483832527E-16,6.55212072256257E-31,
1.));
#31608=DIRECTION('',(-0.707106781186541,0.707106781186554,-2.64360933910924E-17));
#31609=DIRECTION('',(-4.38061483832527E-16,0.,-1.));
#31610=DIRECTION('',(0.707106781186541,-0.707106781186554,0.));
#31611=DIRECTION('center_axis',(0.,-1.,0.));
#31612=DIRECTION('ref_axis',(0.,0.,-1.));
#31613=DIRECTION('',(-1.,0.,0.));
#31614=DIRECTION('',(0.,0.,1.));
#31615=DIRECTION('',(1.,0.,0.));
#31616=DIRECTION('center_axis',(-0.707106781186533,-0.707106781186562,0.));
#31617=DIRECTION('ref_axis',(0.707106781186562,-0.707106781186533,0.));
#31618=DIRECTION('',(-0.707106781186562,0.707106781186533,0.));
#31619=DIRECTION('',(0.,0.,1.));
#31620=DIRECTION('',(0.707106781186562,-0.707106781186533,0.));
#31621=DIRECTION('center_axis',(-1.,1.26161707343768E-16,0.));
#31622=DIRECTION('ref_axis',(-1.26161707343768E-16,-1.,0.));
#31623=DIRECTION('',(1.26161707343768E-16,1.,0.));
#31624=DIRECTION('',(0.,0.,1.));
#31625=DIRECTION('',(-1.26161707343768E-16,-1.,0.));
#31626=DIRECTION('center_axis',(1.,1.26161707343768E-16,0.));
#31627=DIRECTION('ref_axis',(-1.26161707343768E-16,1.,0.));
#31628=DIRECTION('',(1.26161707343768E-16,-1.,0.));
#31629=DIRECTION('',(0.,0.,1.));
#31630=DIRECTION('',(-1.26161707343768E-16,1.,0.));
#31631=DIRECTION('',(0.,0.,1.));
#31632=DIRECTION('center_axis',(0.707106781186533,-0.707106781186562,0.));
#31633=DIRECTION('ref_axis',(0.707106781186562,0.707106781186533,0.));
#31634=DIRECTION('',(-0.707106781186562,-0.707106781186533,0.));
#31635=DIRECTION('',(0.,0.,1.));
#31636=DIRECTION('',(0.707106781186562,0.707106781186533,0.));
#31637=DIRECTION('center_axis',(0.,-1.,0.));
#31638=DIRECTION('ref_axis',(0.,0.,-1.));
#31639=DIRECTION('',(-1.,0.,0.));
#31640=DIRECTION('',(-8.76122967665054E-17,0.,1.));
#31641=DIRECTION('',(1.,0.,0.));
#31642=DIRECTION('center_axis',(-0.707106781186554,0.707106781186542,-6.19512491589247E-17));
#31643=DIRECTION('ref_axis',(8.76122967665054E-17,3.85000586821995E-33,
-1.));
#31644=DIRECTION('',(0.707106781186541,0.707106781186554,0.));
#31645=DIRECTION('',(-0.707106781186541,-0.707106781186554,-2.64360933910925E-17));
#31646=DIRECTION('center_axis',(1.,0.,0.));
#31647=DIRECTION('ref_axis',(0.,0.,-1.));
#31648=DIRECTION('',(0.,1.,0.));
#31649=DIRECTION('',(0.,0.,-1.));
#31650=DIRECTION('',(0.,1.,0.));
#31651=DIRECTION('',(0.,0.,1.));
#31652=DIRECTION('center_axis',(0.70710678118655,0.707106781186545,0.));
#31653=DIRECTION('ref_axis',(-0.707106781186545,0.70710678118655,0.));
#31654=DIRECTION('',(-0.707106781186545,0.70710678118655,0.));
#31655=DIRECTION('',(0.,0.,1.));
#31656=DIRECTION('',(-0.707106781186545,0.70710678118655,0.));
#31657=DIRECTION('center_axis',(0.,1.,0.));
#31658=DIRECTION('ref_axis',(0.,0.,1.));
#31659=DIRECTION('',(0.,0.,1.));
#31660=DIRECTION('',(-1.,0.,0.));
#31661=DIRECTION('',(-1.,0.,0.));
#31662=DIRECTION('center_axis',(0.707106781186549,-0.707106781186546,0.));
#31663=DIRECTION('ref_axis',(0.707106781186546,0.707106781186549,0.));
#31664=DIRECTION('',(0.,0.,1.));
#31665=DIRECTION('',(0.707106781186546,0.707106781186549,0.));
#31666=DIRECTION('',(0.707106781186546,0.707106781186549,0.));
#31667=DIRECTION('center_axis',(-1.62579519772897E-16,-1.,0.));
#31668=DIRECTION('ref_axis',(1.,-1.62579519772897E-16,0.));
#31669=DIRECTION('',(0.,0.,1.));
#31670=DIRECTION('',(1.,-1.62579519772897E-16,0.));
#31671=DIRECTION('',(1.,-1.62579519772897E-16,0.));
#31672=DIRECTION('center_axis',(-0.707106781186544,-0.707106781186551,0.));
#31673=DIRECTION('ref_axis',(0.707106781186551,-0.707106781186544,0.));
#31674=DIRECTION('',(0.,0.,1.));
#31675=DIRECTION('',(0.707106781186551,-0.707106781186544,0.));
#31676=DIRECTION('',(0.707106781186551,-0.707106781186544,0.));
#31677=DIRECTION('center_axis',(0.,1.,0.));
#31678=DIRECTION('ref_axis',(0.,0.,1.));
#31679=DIRECTION('',(-1.,0.,0.));
#31680=DIRECTION('',(0.,0.,1.));
#31681=DIRECTION('',(-1.,0.,0.));
#31682=DIRECTION('center_axis',(0.707106781186544,-0.707106781186551,0.));
#31683=DIRECTION('ref_axis',(0.707106781186551,0.707106781186544,0.));
#31684=DIRECTION('',(0.,0.,1.));
#31685=DIRECTION('',(0.707106781186551,0.707106781186544,0.));
#31686=DIRECTION('',(0.707106781186551,0.707106781186544,0.));
#31687=DIRECTION('center_axis',(1.62579519772897E-16,-1.,0.));
#31688=DIRECTION('ref_axis',(1.,1.62579519772897E-16,0.));
#31689=DIRECTION('',(0.,0.,1.));
#31690=DIRECTION('',(1.,1.62579519772897E-16,0.));
#31691=DIRECTION('',(1.,1.62579519772897E-16,0.));
#31692=DIRECTION('center_axis',(-0.707106781186549,-0.707106781186546,0.));
#31693=DIRECTION('ref_axis',(0.707106781186546,-0.707106781186549,0.));
#31694=DIRECTION('',(0.,0.,1.));
#31695=DIRECTION('',(0.707106781186546,-0.707106781186549,0.));
#31696=DIRECTION('',(0.707106781186546,-0.707106781186549,0.));
#31697=DIRECTION('center_axis',(0.,1.,0.));
#31698=DIRECTION('ref_axis',(0.,0.,1.));
#31699=DIRECTION('',(-1.,0.,0.));
#31700=DIRECTION('',(0.,0.,1.));
#31701=DIRECTION('',(-1.,0.,0.));
#31702=DIRECTION('center_axis',(-0.70710678118655,0.707106781186545,0.));
#31703=DIRECTION('ref_axis',(-0.707106781186545,-0.70710678118655,0.));
#31704=DIRECTION('',(-0.707106781186545,-0.70710678118655,0.));
#31705=DIRECTION('',(0.,0.,1.));
#31706=DIRECTION('',(-0.707106781186545,-0.70710678118655,0.));
#31707=DIRECTION('center_axis',(-1.,0.,0.));
#31708=DIRECTION('ref_axis',(0.,0.,1.));
#31709=DIRECTION('',(0.,-1.,0.));
#31710=DIRECTION('',(0.,0.,1.));
#31711=DIRECTION('',(0.,-1.,0.));
#31712=DIRECTION('center_axis',(-0.707106781186546,-0.707106781186549,0.));
#31713=DIRECTION('ref_axis',(0.707106781186549,-0.707106781186546,0.));
#31714=DIRECTION('',(0.707106781186549,-0.707106781186546,0.));
#31715=DIRECTION('',(0.,0.,1.));
#31716=DIRECTION('',(0.707106781186549,-0.707106781186546,0.));
#31717=DIRECTION('center_axis',(-1.,0.,0.));
#31718=DIRECTION('ref_axis',(0.,0.,1.));
#31719=DIRECTION('',(0.,-1.,0.));
#31720=DIRECTION('',(0.,0.,1.));
#31721=DIRECTION('',(0.,-1.,0.));
#31722=DIRECTION('center_axis',(1.2823896663807E-16,1.,0.));
#31723=DIRECTION('ref_axis',(-1.,1.2823896663807E-16,0.));
#31724=DIRECTION('center_axis',(-1.2823896663807E-16,-1.,0.));
#31725=DIRECTION('ref_axis',(-1.,1.2823896663807E-16,2.52323414687535E-15));
#31726=DIRECTION('',(1.,-1.2823896663807E-16,0.));
#31727=DIRECTION('',(0.,0.,-1.));
#31728=DIRECTION('center_axis',(1.,-2.04085114820801E-16,0.));
#31729=DIRECTION('ref_axis',(2.04085114820801E-16,1.,0.));
#31730=DIRECTION('',(0.,0.,1.));
#31731=DIRECTION('',(0.,1.,0.));
#31732=DIRECTION('',(-2.04085114820801E-16,-1.,0.));
#31733=DIRECTION('center_axis',(-0.965925826289069,-0.258819045102518,0.));
#31734=DIRECTION('ref_axis',(0.258819045102518,-0.965925826289069,0.));
#31735=DIRECTION('center_axis',(-0.965925826289069,-0.258819045102518,0.));
#31736=DIRECTION('ref_axis',(0.258819045102518,-0.965925826289069,0.));
#31737=DIRECTION('',(0.258819045102518,-0.965925826289069,0.));
#31738=DIRECTION('',(0.,0.,1.));
#31739=DIRECTION('center_axis',(0.965925826289069,-0.258819045102518,0.));
#31740=DIRECTION('ref_axis',(0.258819045102518,0.965925826289069,0.));
#31741=DIRECTION('center_axis',(0.965925826289069,-0.258819045102518,0.));
#31742=DIRECTION('ref_axis',(0.258819045102518,0.965925826289069,0.));
#31743=DIRECTION('',(0.258819045102518,0.965925826289069,0.));
#31744=DIRECTION('',(0.,0.,-1.));
#31745=DIRECTION('center_axis',(-1.,-2.04085114820801E-16,0.));
#31746=DIRECTION('ref_axis',(2.04085114820801E-16,-1.,0.));
#31747=DIRECTION('',(0.,0.,-1.));
#31748=DIRECTION('',(0.,-1.,0.));
#31749=DIRECTION('',(-2.04085114820801E-16,1.,0.));
#31750=DIRECTION('center_axis',(-1.2823896663807E-16,1.,0.));
#31751=DIRECTION('ref_axis',(-1.,-1.2823896663807E-16,0.));
#31752=DIRECTION('',(1.,1.2823896663807E-16,0.));
#31753=DIRECTION('center_axis',(-1.2823896663807E-16,-1.,0.));
#31754=DIRECTION('ref_axis',(-1.,1.2823896663807E-16,-2.52323414687536E-15));
#31755=DIRECTION('center_axis',(-0.61566147532566,-0.788010753606721,0.));
#31756=DIRECTION('ref_axis',(0.78801075360672,-0.61566147532566,0.));
#31757=DIRECTION('center_axis',(-0.615661475325663,-0.788010753606718,3.86575390646386E-15));
#31758=DIRECTION('ref_axis',(0.788010753606718,-0.615661475325663,-6.5758767605984E-13));
#31759=DIRECTION('',(0.78801075360672,-0.61566147532566,0.));
#31760=DIRECTION('',(0.,0.,1.));
#31761=DIRECTION('center_axis',(0.707106781186548,0.707106781186547,0.));
#31762=DIRECTION('ref_axis',(-0.707106781186547,0.707106781186548,0.));
#31763=DIRECTION('',(0.707106781186547,-0.707106781186548,0.));
#31764=DIRECTION('',(-0.707106781186547,0.707106781186548,0.));
#31765=DIRECTION('',(0.,0.,1.));
#31766=DIRECTION('center_axis',(-0.707106781186548,0.707106781186547,0.));
#31767=DIRECTION('ref_axis',(-0.707106781186547,-0.707106781186548,0.));
#31768=DIRECTION('',(0.707106781186547,0.707106781186548,0.));
#31769=DIRECTION('',(0.,0.,1.));
#31770=DIRECTION('',(-0.707106781186547,-0.707106781186548,0.));
#31771=DIRECTION('center_axis',(0.,0.,1.));
#31772=DIRECTION('ref_axis',(1.,0.,0.));
#31773=DIRECTION('',(1.,0.,0.));
#31774=DIRECTION('',(1.,-4.33680868994201E-15,0.));
#31775=DIRECTION('',(0.78801075360672,0.61566147532566,0.));
#31776=DIRECTION('center_axis',(0.61566147532566,-0.788010753606721,0.));
#31777=DIRECTION('ref_axis',(0.78801075360672,0.61566147532566,0.));
#31778=DIRECTION('center_axis',(0.615661475325666,-0.788010753606716,-4.56861825309369E-15));
#31779=DIRECTION('ref_axis',(0.788010753606716,0.615661475325665,-3.955354877202E-13));
#31780=DIRECTION('',(0.,0.,1.));
#31781=DIRECTION('center_axis',(3.7386281809845E-17,4.26676715361993E-32,
-1.));
#31782=DIRECTION('ref_axis',(-1.,4.36567830323557E-65,-3.7386281809845E-17));
#31783=DIRECTION('',(1.,0.,0.));
#31784=DIRECTION('',(0.707106781186546,0.707106781186549,0.));
#31785=DIRECTION('center_axis',(0.,0.,1.));
#31786=DIRECTION('ref_axis',(1.,0.,0.));
#31787=DIRECTION('',(0.,1.,0.));
#31788=DIRECTION('center_axis',(0.,0.,1.));
#31789=DIRECTION('ref_axis',(1.,0.,0.));
#31790=DIRECTION('',(-0.707106781186549,0.707106781186546,0.));
#31791=DIRECTION('center_axis',(0.,0.,-1.));
#31792=DIRECTION('ref_axis',(1.,0.,0.));
#31793=DIRECTION('center_axis',(0.,0.,1.));
#31794=DIRECTION('ref_axis',(1.,0.,0.));
#31795=DIRECTION('center_axis',(0.,0.,-1.));
#31796=DIRECTION('ref_axis',(1.,0.,0.));
#31797=DIRECTION('',(-0.707106781186548,0.707106781186547,0.));
#31798=DIRECTION('center_axis',(0.,0.,-1.));
#31799=DIRECTION('ref_axis',(1.,0.,0.));
#31800=DIRECTION('',(0.,1.,0.));
#31801=DIRECTION('center_axis',(0.,0.,-1.));
#31802=DIRECTION('ref_axis',(1.,0.,0.));
#31803=DIRECTION('',(0.707106781186545,0.70710678118655,0.));
#31804=DIRECTION('center_axis',(0.,0.,-1.));
#31805=DIRECTION('ref_axis',(1.,0.,0.));
#31806=DIRECTION('center_axis',(0.,0.,1.));
#31807=DIRECTION('ref_axis',(1.,0.,0.));
#31808=DIRECTION('center_axis',(0.,0.,-1.));
#31809=DIRECTION('ref_axis',(1.,0.,0.));
#31810=DIRECTION('',(0.707106781186546,0.707106781186549,0.));
#31811=DIRECTION('',(1.,1.22464679914735E-16,0.));
#31812=DIRECTION('',(0.707106781186546,-0.707106781186549,0.));
#31813=DIRECTION('center_axis',(0.,0.,-1.));
#31814=DIRECTION('ref_axis',(1.,0.,0.));
#31815=DIRECTION('center_axis',(0.,0.,1.));
#31816=DIRECTION('ref_axis',(1.,0.,0.));
#31817=DIRECTION('center_axis',(0.,0.,-1.));
#31818=DIRECTION('ref_axis',(1.,0.,0.));
#31819=DIRECTION('',(0.707106781186545,-0.70710678118655,0.));
#31820=DIRECTION('center_axis',(0.,0.,-1.));
#31821=DIRECTION('ref_axis',(1.,0.,0.));
#31822=DIRECTION('',(0.,-1.,0.));
#31823=DIRECTION('center_axis',(0.,0.,-1.));
#31824=DIRECTION('ref_axis',(1.,0.,0.));
#31825=DIRECTION('',(-0.707106781186548,-0.707106781186547,0.));
#31826=DIRECTION('center_axis',(0.,0.,-1.));
#31827=DIRECTION('ref_axis',(1.,0.,0.));
#31828=DIRECTION('center_axis',(0.,0.,1.));
#31829=DIRECTION('ref_axis',(1.,0.,0.));
#31830=DIRECTION('center_axis',(0.,0.,-1.));
#31831=DIRECTION('ref_axis',(1.,0.,0.));
#31832=DIRECTION('',(-0.707106781186549,-0.707106781186546,0.));
#31833=DIRECTION('center_axis',(0.,0.,1.));
#31834=DIRECTION('ref_axis',(1.,0.,0.));
#31835=DIRECTION('',(0.,-1.,0.));
#31836=DIRECTION('center_axis',(0.,0.,1.));
#31837=DIRECTION('ref_axis',(1.,0.,0.));
#31838=DIRECTION('',(0.707106781186546,-0.707106781186549,0.));
#31839=DIRECTION('',(1.,-3.50803534070133E-16,0.));
#31840=DIRECTION('center_axis',(0.,0.,-1.));
#31841=DIRECTION('ref_axis',(-1.,0.,0.));
#31842=DIRECTION('',(1.,-4.33680868994201E-15,0.));
#31843=DIRECTION('',(-0.707106781186547,-0.707106781186548,0.));
#31844=DIRECTION('',(-1.26161707343768E-16,-1.,0.));
#31845=DIRECTION('',(0.707106781186562,-0.707106781186533,0.));
#31846=DIRECTION('',(1.,0.,0.));
#31847=DIRECTION('',(-0.707106781186548,0.707106781186547,0.));
#31848=DIRECTION('',(1.,1.19636101791504E-15,0.));
#31849=DIRECTION('',(-0.707106781186541,-0.707106781186554,0.));
#31850=DIRECTION('',(1.,0.,0.));
#31851=DIRECTION('',(0.707106781186562,0.707106781186533,0.));
#31852=DIRECTION('',(-1.26161707343768E-16,1.,0.));
#31853=DIRECTION('',(-0.707106781186547,0.707106781186548,0.));
#31854=DIRECTION('',(1.,0.,0.));
#31855=DIRECTION('center_axis',(-0.707106781186554,0.707106781186542,1.85853747476774E-16));
#31856=DIRECTION('ref_axis',(-2.62836890299516E-16,1.6519124519235E-33,
-1.));
#31857=DIRECTION('',(0.707106781186541,0.707106781186554,0.));
#31858=DIRECTION('',(2.62836890299516E-16,0.,1.));
#31859=DIRECTION('',(2.62836890299516E-16,0.,1.));
#31860=DIRECTION('center_axis',(-0.707106781186533,-0.707106781186562,0.));
#31861=DIRECTION('ref_axis',(0.707106781186562,-0.707106781186533,0.));
#31862=DIRECTION('',(-0.707106781186562,0.707106781186533,0.));
#31863=DIRECTION('',(0.,0.,1.));
#31864=DIRECTION('',(0.,0.,1.));
#31865=DIRECTION('center_axis',(-1.,1.26161707343768E-16,0.));
#31866=DIRECTION('ref_axis',(-1.26161707343768E-16,-1.,0.));
#31867=DIRECTION('',(1.26161707343768E-16,1.,0.));
#31868=DIRECTION('',(0.,0.,1.));
#31869=DIRECTION('center_axis',(-0.707106781186548,0.707106781186547,0.));
#31870=DIRECTION('ref_axis',(-0.707106781186547,-0.707106781186548,0.));
#31871=DIRECTION('',(0.707106781186547,0.707106781186548,0.));
#31872=DIRECTION('',(0.,0.,1.));
#31873=DIRECTION('center_axis',(0.,-1.,0.));
#31874=DIRECTION('ref_axis',(0.,0.,-1.));
#31875=DIRECTION('',(-1.,0.,0.));
#31876=DIRECTION('',(2.62836890299516E-16,0.,-1.));
#31877=DIRECTION('center_axis',(0.,0.,1.));
#31878=DIRECTION('ref_axis',(1.,0.,0.));
#31879=DIRECTION('',(0.,0.,1.));
#31880=DIRECTION('center_axis',(0.,0.,1.));
#31881=DIRECTION('ref_axis',(1.,0.,0.));
#31882=DIRECTION('',(0.,0.,-1.));
#31883=DIRECTION('center_axis',(0.,0.,1.));
#31884=DIRECTION('ref_axis',(1.,0.,0.));
#31885=DIRECTION('',(0.,0.,1.));
#31886=DIRECTION('center_axis',(0.,0.,1.));
#31887=DIRECTION('ref_axis',(1.,0.,0.));
#31888=DIRECTION('',(0.,0.,-1.));
#31889=DIRECTION('center_axis',(-1.,0.,0.));
#31890=DIRECTION('ref_axis',(0.,0.,1.));
#31891=DIRECTION('',(0.,-1.,0.));
#31892=DIRECTION('center_axis',(-0.707106781186549,-0.707106781186546,0.));
#31893=DIRECTION('ref_axis',(0.707106781186546,-0.707106781186549,0.));
#31894=DIRECTION('',(0.707106781186546,-0.707106781186549,0.));
#31895=DIRECTION('',(0.,0.,1.));
#31896=DIRECTION('center_axis',(-6.49101394191508E-16,-1.,0.));
#31897=DIRECTION('ref_axis',(1.,-6.49101394191508E-16,0.));
#31898=DIRECTION('',(1.,-3.50803534070133E-16,0.));
#31899=DIRECTION('center_axis',(0.,0.,1.));
#31900=DIRECTION('ref_axis',(1.,0.,0.));
#31901=DIRECTION('center_axis',(0.,0.,-1.));
#31902=DIRECTION('ref_axis',(1.,0.,0.));
#31903=DIRECTION('',(0.,0.,-1.));
#31904=DIRECTION('',(0.,0.,1.));
#31905=DIRECTION('center_axis',(0.,0.,1.));
#31906=DIRECTION('ref_axis',(1.,0.,0.));
#31907=DIRECTION('center_axis',(0.,0.,-1.));
#31908=DIRECTION('ref_axis',(1.,0.,0.));
#31909=DIRECTION('',(0.,0.,-1.));
#31910=DIRECTION('',(0.,0.,1.));
#31911=DIRECTION('center_axis',(0.,0.,1.));
#31912=DIRECTION('ref_axis',(1.,0.,0.));
#31913=DIRECTION('center_axis',(0.,0.,1.));
#31914=DIRECTION('ref_axis',(1.,0.,0.));
#31915=DIRECTION('center_axis',(0.,0.,-1.));
#31916=DIRECTION('ref_axis',(-1.,0.,0.));
#31917=DIRECTION('center_axis',(0.,0.,-1.));
#31918=DIRECTION('ref_axis',(1.,0.,0.));
#31919=DIRECTION('',(0.,0.,-1.));
#31920=DIRECTION('',(0.,0.,1.));
#31921=DIRECTION('center_axis',(0.,0.,-1.));
#31922=DIRECTION('ref_axis',(-1.,0.,0.));
#31923=DIRECTION('center_axis',(0.,0.,-1.));
#31924=DIRECTION('ref_axis',(1.,0.,0.));
#31925=DIRECTION('',(0.,0.,-1.));
#31926=DIRECTION('',(0.,0.,1.));
#31927=DIRECTION('center_axis',(-1.,0.,0.));
#31928=DIRECTION('ref_axis',(0.,0.,1.));
#31929=DIRECTION('',(0.,-1.,0.));
#31930=DIRECTION('center_axis',(-0.707106781186546,0.707106781186549,0.));
#31931=DIRECTION('ref_axis',(-0.707106781186549,-0.707106781186546,0.));
#31932=DIRECTION('',(-0.707106781186548,-0.707106781186547,0.));
#31933=DIRECTION('center_axis',(0.,0.,1.));
#31934=DIRECTION('ref_axis',(1.,0.,0.));
#31935=DIRECTION('center_axis',(0.,0.,-1.));
#31936=DIRECTION('ref_axis',(1.,0.,0.));
#31937=DIRECTION('',(0.,0.,-1.));
#31938=DIRECTION('',(0.,0.,1.));
#31939=DIRECTION('center_axis',(0.,0.,1.));
#31940=DIRECTION('ref_axis',(1.,0.,0.));
#31941=DIRECTION('center_axis',(0.,0.,-1.));
#31942=DIRECTION('ref_axis',(1.,0.,0.));
#31943=DIRECTION('',(0.,0.,-1.));
#31944=DIRECTION('',(0.,0.,1.));
#31945=DIRECTION('center_axis',(0.,0.,1.));
#31946=DIRECTION('ref_axis',(1.,0.,0.));
#31947=DIRECTION('center_axis',(0.,0.,1.));
#31948=DIRECTION('ref_axis',(1.,0.,0.));
#31949=DIRECTION('center_axis',(1.22464679914735E-16,-1.,0.));
#31950=DIRECTION('ref_axis',(1.,1.22464679914735E-16,0.));
#31951=DIRECTION('',(0.,0.,1.));
#31952=DIRECTION('',(1.,1.22464679914735E-16,0.));
#31953=DIRECTION('',(0.,0.,1.));
#31954=DIRECTION('center_axis',(-0.707106781186549,-0.707106781186546,0.));
#31955=DIRECTION('ref_axis',(0.707106781186546,-0.707106781186549,0.));
#31956=DIRECTION('',(0.707106781186546,-0.707106781186549,0.));
#31957=DIRECTION('center_axis',(0.,0.,1.));
#31958=DIRECTION('ref_axis',(1.,0.,0.));
#31959=DIRECTION('center_axis',(0.,0.,-1.));
#31960=DIRECTION('ref_axis',(1.,0.,0.));
#31961=DIRECTION('',(0.,0.,-1.));
#31962=DIRECTION('',(0.,0.,1.));
#31963=DIRECTION('center_axis',(0.,0.,1.));
#31964=DIRECTION('ref_axis',(1.,0.,0.));
#31965=DIRECTION('center_axis',(0.,0.,-1.));
#31966=DIRECTION('ref_axis',(1.,0.,0.));
#31967=DIRECTION('',(0.,0.,-1.));
#31968=DIRECTION('',(0.,0.,1.));
#31969=DIRECTION('center_axis',(0.,0.,1.));
#31970=DIRECTION('ref_axis',(1.,0.,0.));
#31971=DIRECTION('center_axis',(0.,0.,1.));
#31972=DIRECTION('ref_axis',(1.,0.,0.));
#31973=DIRECTION('center_axis',(0.,0.,-1.));
#31974=DIRECTION('ref_axis',(-1.,0.,0.));
#31975=DIRECTION('center_axis',(0.,0.,-1.));
#31976=DIRECTION('ref_axis',(1.,0.,0.));
#31977=DIRECTION('',(0.,0.,-1.));
#31978=DIRECTION('',(0.,0.,1.));
#31979=DIRECTION('center_axis',(0.,0.,-1.));
#31980=DIRECTION('ref_axis',(-1.,0.,0.));
#31981=DIRECTION('center_axis',(0.,0.,-1.));
#31982=DIRECTION('ref_axis',(1.,0.,0.));
#31983=DIRECTION('',(0.,0.,-1.));
#31984=DIRECTION('',(0.,0.,1.));
#31985=DIRECTION('center_axis',(1.,0.,0.));
#31986=DIRECTION('ref_axis',(0.,0.,-1.));
#31987=DIRECTION('',(0.,1.,0.));
#31988=DIRECTION('center_axis',(0.707106781186549,-0.707106781186546,0.));
#31989=DIRECTION('ref_axis',(0.707106781186546,0.707106781186549,0.));
#31990=DIRECTION('',(0.707106781186545,0.70710678118655,0.));
#31991=DIRECTION('center_axis',(0.707106781186549,-0.707106781186546,0.));
#31992=DIRECTION('ref_axis',(0.707106781186546,0.707106781186549,0.));
#31993=DIRECTION('',(0.707106781186546,0.707106781186549,0.));
#31994=DIRECTION('center_axis',(0.,0.,1.));
#31995=DIRECTION('ref_axis',(1.,0.,0.));
#31996=DIRECTION('center_axis',(0.,0.,-1.));
#31997=DIRECTION('ref_axis',(1.,0.,0.));
#31998=DIRECTION('',(0.,0.,-1.));
#31999=DIRECTION('',(0.,0.,1.));
#32000=DIRECTION('center_axis',(0.,0.,1.));
#32001=DIRECTION('ref_axis',(1.,0.,0.));
#32002=DIRECTION('center_axis',(0.,0.,-1.));
#32003=DIRECTION('ref_axis',(1.,0.,0.));
#32004=DIRECTION('',(0.,0.,-1.));
#32005=DIRECTION('',(0.,0.,1.));
#32006=DIRECTION('center_axis',(0.,0.,1.));
#32007=DIRECTION('ref_axis',(1.,0.,0.));
#32008=DIRECTION('center_axis',(0.,0.,1.));
#32009=DIRECTION('ref_axis',(1.,0.,0.));
#32010=DIRECTION('center_axis',(0.,0.,1.));
#32011=DIRECTION('ref_axis',(1.,0.,0.));
#32012=DIRECTION('',(0.,0.,1.));
#32013=DIRECTION('center_axis',(0.,0.,1.));
#32014=DIRECTION('ref_axis',(1.,0.,0.));
#32015=DIRECTION('',(0.,0.,-1.));
#32016=DIRECTION('center_axis',(0.,0.,1.));
#32017=DIRECTION('ref_axis',(1.,0.,0.));
#32018=DIRECTION('',(0.,0.,1.));
#32019=DIRECTION('center_axis',(0.,0.,1.));
#32020=DIRECTION('ref_axis',(1.,0.,0.));
#32021=DIRECTION('',(0.,0.,-1.));
#32022=DIRECTION('center_axis',(0.707106781186548,0.707106781186547,0.));
#32023=DIRECTION('ref_axis',(-0.707106781186547,0.707106781186548,0.));
#32024=DIRECTION('',(0.707106781186547,-0.707106781186548,0.));
#32025=DIRECTION('',(0.,0.,1.));
#32026=DIRECTION('',(0.,0.,1.));
#32027=DIRECTION('center_axis',(1.,1.26161707343768E-16,0.));
#32028=DIRECTION('ref_axis',(-1.26161707343768E-16,1.,0.));
#32029=DIRECTION('',(1.26161707343768E-16,-1.,0.));
#32030=DIRECTION('',(0.,0.,1.));
#32031=DIRECTION('center_axis',(0.707106781186533,-0.707106781186562,0.));
#32032=DIRECTION('ref_axis',(0.707106781186562,0.707106781186533,0.));
#32033=DIRECTION('',(-0.707106781186562,-0.707106781186533,0.));
#32034=DIRECTION('',(0.,0.,1.));
#32035=DIRECTION('center_axis',(0.,-1.,0.));
#32036=DIRECTION('ref_axis',(0.,0.,-1.));
#32037=DIRECTION('',(-1.,0.,0.));
#32038=DIRECTION('center_axis',(0.,-1.,0.));
#32039=DIRECTION('ref_axis',(0.,0.,-1.));
#32040=DIRECTION('',(1.,0.,0.));
#32041=DIRECTION('',(0.,0.,1.));
#32042=DIRECTION('center_axis',(0.707106781186549,-0.707106781186546,0.));
#32043=DIRECTION('ref_axis',(0.707106781186546,0.707106781186549,0.));
#32044=DIRECTION('',(0.707106781186546,0.707106781186549,0.));
#32045=DIRECTION('center_axis',(1.,0.,0.));
#32046=DIRECTION('ref_axis',(0.,0.,-1.));
#32047=DIRECTION('',(0.,1.,0.));
#32048=DIRECTION('center_axis',(0.707106781186546,0.707106781186549,0.));
#32049=DIRECTION('ref_axis',(-0.707106781186549,0.707106781186546,0.));
#32050=DIRECTION('',(-0.707106781186549,0.707106781186546,0.));
#32051=DIRECTION('center_axis',(0.707106781186546,0.707106781186549,0.));
#32052=DIRECTION('ref_axis',(-0.707106781186549,0.707106781186546,0.));
#32053=DIRECTION('',(-0.707106781186548,0.707106781186547,0.));
#32054=DIRECTION('center_axis',(-0.707106781186549,-0.707106781186546,0.));
#32055=DIRECTION('ref_axis',(0.707106781186546,-0.707106781186549,0.));
#32056=DIRECTION('',(0.707106781186545,-0.70710678118655,0.));
#32057=DIRECTION('center_axis',(-0.707106781186546,0.707106781186549,0.));
#32058=DIRECTION('ref_axis',(-0.707106781186549,-0.707106781186546,0.));
#32059=DIRECTION('',(-0.707106781186549,-0.707106781186546,0.));
#32060=DIRECTION('center_axis',(0.707106781186547,0.707106781186548,1.85853747476773E-16));
#32061=DIRECTION('ref_axis',(-2.62836890299516E-16,-6.09040047468605E-31,
1.));
#32062=DIRECTION('',(0.707106781186548,-0.707106781186547,0.));
#32063=DIRECTION('',(2.62836890299516E-16,6.28895619248706E-31,-1.));
#32064=DIRECTION('center_axis',(-1.19636101791504E-15,1.,3.14447809624353E-31));
#32065=DIRECTION('ref_axis',(-1.,-1.19636101791504E-15,0.));
#32066=DIRECTION('',(-1.,-1.19636101791504E-15,0.));
#32067=DIRECTION('center_axis',(0.,0.,1.));
#32068=DIRECTION('ref_axis',(1.,0.,0.));
#32069=DIRECTION('center_axis',(1.,1.73472347597681E-16,0.));
#32070=DIRECTION('ref_axis',(-1.73472347597681E-16,1.,0.));
#32071=DIRECTION('',(-1.73472347597681E-16,1.,0.));
#32072=DIRECTION('',(0.,0.,1.));
#32073=DIRECTION('center_axis',(0.,0.,1.));
#32074=DIRECTION('ref_axis',(1.,0.,0.));
#32075=DIRECTION('center_axis',(0.,0.,1.));
#32076=DIRECTION('ref_axis',(1.,0.,0.));
#32077=DIRECTION('',(0.,0.,1.));
#32078=DIRECTION('center_axis',(-1.,1.73472347597681E-16,0.));
#32079=DIRECTION('ref_axis',(-1.73472347597681E-16,-1.,0.));
#32080=DIRECTION('',(-1.73472347597681E-16,-1.,0.));
#32081=DIRECTION('center_axis',(0.,0.,1.));
#32082=DIRECTION('ref_axis',(1.,0.,0.));
#32083=DIRECTION('center_axis',(0.,-1.,0.));
#32084=DIRECTION('ref_axis',(0.,0.,-1.));
#32085=DIRECTION('center_axis',(0.,-1.,0.));
#32086=DIRECTION('ref_axis',(0.,0.,-1.));
#32087=DIRECTION('center_axis',(0.,-1.,0.));
#32088=DIRECTION('ref_axis',(0.,0.,-1.));
#32089=DIRECTION('center_axis',(0.,-1.,0.));
#32090=DIRECTION('ref_axis',(0.,0.,-1.));
#32091=DIRECTION('axis',(0.,0.,1.));
#32092=DIRECTION('refdir',(1.,0.,0.));
#32093=DIRECTION('center_axis',(-6.99485272571294E-17,-0.923879532511288,
0.382683432365087));
#32094=DIRECTION('ref_axis',(0.,-0.382683432365087,-0.923879532511288));
#32095=DIRECTION('center_axis',(0.,0.923879532511288,-0.382683432365087));
#32096=DIRECTION('ref_axis',(0.,0.382683432365087,0.923879532511288));
#32097=DIRECTION('center_axis',(1.,-1.77588086089071E-17,1.39910753728411E-16));
#32098=DIRECTION('ref_axis',(-1.22464679914735E-16,0.382683432365087,0.923879532511288));
#32099=DIRECTION('center_axis',(-6.99485272571294E-17,-0.923879532511288,
0.382683432365087));
#32100=DIRECTION('ref_axis',(6.87413134363318E-33,-0.382683432365087,-0.923879532511288));
#32101=DIRECTION('center_axis',(-1.,1.77588086089071E-17,-1.39910753728411E-16));
#32102=DIRECTION('ref_axis',(-1.22464679914735E-16,0.382683432365087,0.923879532511288));
#32103=DIRECTION('center_axis',(-6.99485272571294E-17,-0.923879532511288,
0.382683432365087));
#32104=DIRECTION('ref_axis',(1.30371071656723E-32,-0.382683432365087,-0.923879532511288));
#32105=DIRECTION('center_axis',(-6.99485272571294E-17,-0.923879532511288,
0.382683432365087));
#32106=DIRECTION('ref_axis',(7.11155521594025E-34,-0.382683432365087,-0.923879532511288));
#32107=DIRECTION('',(1.0961176199419E-16,0.722104291896042,-0.691784208858019));
#32108=DIRECTION('center_axis',(-6.99485272571294E-17,-0.923879532511288,
0.382683432365087));
#32109=DIRECTION('ref_axis',(7.11155521594025E-34,-0.382683432365087,-0.923879532511288));
#32110=DIRECTION('center_axis',(-0.5,-0.33141357403559,-0.800103145191267));
#32111=DIRECTION('ref_axis',(-0.866025403784439,0.191341716182545,0.461939766255643));
#32112=DIRECTION('center_axis',(-6.99485272571294E-17,-0.923879532511288,
0.382683432365087));
#32113=DIRECTION('ref_axis',(-4.26190864642653E-32,-0.382683432365087,-0.923879532511288));
#32114=DIRECTION('center_axis',(0.,-0.923879532511288,0.382683432365087));
#32115=DIRECTION('ref_axis',(0.,-0.382683432365087,-0.923879532511288));
#32116=DIRECTION('center_axis',(0.,-0.923879532511288,0.382683432365087));
#32117=DIRECTION('ref_axis',(0.,-0.382683432365087,-0.923879532511288));
#32118=DIRECTION('center_axis',(0.,0.923879532511288,-0.382683432365087));
#32119=DIRECTION('ref_axis',(0.,0.382683432365087,0.923879532511288));
#32120=DIRECTION('center_axis',(0.,0.923879532511288,-0.382683432365087));
#32121=DIRECTION('ref_axis',(0.,0.382683432365087,0.923879532511288));
#32122=DIRECTION('center_axis',(0.,-0.923879532511288,0.382683432365087));
#32123=DIRECTION('ref_axis',(0.,-0.382683432365087,-0.923879532511288));
#32124=DIRECTION('center_axis',(0.,-0.923879532511288,0.382683432365087));
#32125=DIRECTION('ref_axis',(0.,-0.382683432365087,-0.923879532511288));
#32126=DIRECTION('',(0.,0.923879532511288,-0.382683432365087));
#32127=DIRECTION('center_axis',(0.,-0.923879532511288,0.382683432365087));
#32128=DIRECTION('ref_axis',(0.,-0.382683432365087,-0.923879532511288));
#32129=DIRECTION('center_axis',(0.,0.,-1.));
#32130=DIRECTION('ref_axis',(-1.,0.,0.));
#32131=DIRECTION('center_axis',(0.,0.,-1.));
#32132=DIRECTION('ref_axis',(-1.,0.,0.));
#32133=DIRECTION('center_axis',(0.,0.,-1.));
#32134=DIRECTION('ref_axis',(-1.,0.,0.));
#32135=DIRECTION('center_axis',(0.,0.,-1.));
#32136=DIRECTION('ref_axis',(-1.,0.,0.));
#32137=DIRECTION('',(0.,0.,1.));
#32138=DIRECTION('center_axis',(0.,0.,-1.));
#32139=DIRECTION('ref_axis',(-1.,0.,0.));
#32140=DIRECTION('center_axis',(0.,0.,-1.));
#32141=DIRECTION('ref_axis',(-1.,0.,0.));
#32142=DIRECTION('center_axis',(0.,0.,-1.));
#32143=DIRECTION('ref_axis',(-1.,0.,0.));
#32144=DIRECTION('center_axis',(0.,0.,-1.));
#32145=DIRECTION('ref_axis',(-1.,0.,0.));
#32146=DIRECTION('center_axis',(0.,0.,-1.));
#32147=DIRECTION('ref_axis',(-1.,0.,0.));
#32148=DIRECTION('center_axis',(0.,0.,-1.));
#32149=DIRECTION('ref_axis',(-1.,0.,0.));
#32150=DIRECTION('center_axis',(6.12323399573677E-17,0.,1.));
#32151=DIRECTION('ref_axis',(1.,0.,0.));
#32152=DIRECTION('center_axis',(1.22464679914735E-16,-1.,0.));
#32153=DIRECTION('ref_axis',(-1.,-1.22464679914735E-16,0.));
#32154=DIRECTION('center_axis',(0.,-0.923879532511288,0.382683432365087));
#32155=DIRECTION('ref_axis',(0.,-0.382683432365087,-0.923879532511288));
#32156=DIRECTION('center_axis',(0.,-0.923879532511288,0.382683432365087));
#32157=DIRECTION('ref_axis',(0.,-0.382683432365087,-0.923879532511288));
#32158=DIRECTION('center_axis',(0.,-0.923879532511288,0.382683432365087));
#32159=DIRECTION('ref_axis',(0.,-0.382683432365087,-0.923879532511288));
#32160=DIRECTION('center_axis',(0.,-0.923879532511288,0.382683432365087));
#32161=DIRECTION('ref_axis',(0.,-0.382683432365087,-0.923879532511288));
#32162=DIRECTION('center_axis',(0.,-0.923879532511288,0.382683432365087));
#32163=DIRECTION('ref_axis',(0.,-0.382683432365087,-0.923879532511288));
#32164=DIRECTION('center_axis',(0.,-0.923879532511288,0.382683432365087));
#32165=DIRECTION('ref_axis',(0.,-0.382683432365087,-0.923879532511288));
#32166=DIRECTION('center_axis',(0.,0.923879532511288,-0.382683432365087));
#32167=DIRECTION('ref_axis',(0.,0.382683432365087,0.923879532511288));
#32168=DIRECTION('center_axis',(0.,0.923879532511288,-0.382683432365087));
#32169=DIRECTION('ref_axis',(0.,0.382683432365087,0.923879532511288));
#32170=DIRECTION('center_axis',(0.,0.923879532511288,-0.382683432365087));
#32171=DIRECTION('ref_axis',(0.,0.382683432365087,0.923879532511288));
#32172=DIRECTION('center_axis',(0.,0.923879532511288,-0.382683432365087));
#32173=DIRECTION('ref_axis',(0.,0.382683432365087,0.923879532511288));
#32174=DIRECTION('center_axis',(0.,0.923879532511288,-0.382683432365087));
#32175=DIRECTION('ref_axis',(0.,0.382683432365087,0.923879532511288));
#32176=DIRECTION('center_axis',(0.,-0.923879532511288,0.382683432365087));
#32177=DIRECTION('ref_axis',(0.,-0.382683432365087,-0.923879532511288));
#32178=DIRECTION('center_axis',(0.,0.,1.));
#32179=DIRECTION('ref_axis',(1.,0.,0.));
#32180=DIRECTION('',(3.56799717200074E-15,-1.,0.));
#32181=DIRECTION('',(-0.866025403784438,-0.500000000000001,0.));
#32182=DIRECTION('center_axis',(0.,0.,1.));
#32183=DIRECTION('ref_axis',(1.,0.,0.));
#32184=DIRECTION('',(-0.866025403784438,-0.500000000000001,0.));
#32185=DIRECTION('',(-0.866025403784441,0.499999999999995,0.));
#32186=DIRECTION('center_axis',(0.,0.,1.));
#32187=DIRECTION('ref_axis',(1.,0.,0.));
#32188=DIRECTION('',(-0.866025403784441,0.499999999999995,0.));
#32189=DIRECTION('',(-1.05162021911601E-14,1.,0.));
#32190=DIRECTION('center_axis',(0.,0.,1.));
#32191=DIRECTION('ref_axis',(1.,0.,0.));
#32192=DIRECTION('',(-1.05162021911601E-14,1.,0.));
#32193=DIRECTION('',(0.866025403784434,0.500000000000007,0.));
#32194=DIRECTION('center_axis',(0.,0.,1.));
#32195=DIRECTION('ref_axis',(1.,0.,0.));
#32196=DIRECTION('',(0.866025403784434,0.500000000000007,0.));
#32197=DIRECTION('',(0.866025403784441,-0.499999999999995,0.));
#32198=DIRECTION('center_axis',(0.,0.,1.));
#32199=DIRECTION('ref_axis',(1.,0.,0.));
#32200=DIRECTION('',(0.866025403784441,-0.499999999999995,0.));
#32201=DIRECTION('',(3.56799717200074E-15,-1.,0.));
#32202=DIRECTION('center_axis',(0.499999999999995,0.866025403784442,0.));
#32203=DIRECTION('ref_axis',(-0.866025403784441,0.499999999999995,0.));
#32204=DIRECTION('',(-0.866025403784441,0.499999999999995,0.));
#32205=DIRECTION('',(0.,0.,1.));
#32206=DIRECTION('',(0.,0.,1.));
#32207=DIRECTION('center_axis',(1.,1.05162021911601E-14,0.));
#32208=DIRECTION('ref_axis',(-1.05162021911601E-14,1.,0.));
#32209=DIRECTION('',(-1.05162021911601E-14,1.,0.));
#32210=DIRECTION('',(0.,0.,1.));
#32211=DIRECTION('center_axis',(0.500000000000007,-0.866025403784435,0.));
#32212=DIRECTION('ref_axis',(0.866025403784435,0.500000000000007,0.));
#32213=DIRECTION('',(0.866025403784434,0.500000000000007,0.));
#32214=DIRECTION('',(0.,0.,1.));
#32215=DIRECTION('center_axis',(-0.499999999999995,-0.866025403784441,0.));
#32216=DIRECTION('ref_axis',(0.866025403784442,-0.499999999999995,0.));
#32217=DIRECTION('',(0.866025403784441,-0.499999999999995,0.));
#32218=DIRECTION('',(0.,0.,1.));
#32219=DIRECTION('center_axis',(-1.,-3.56799717200074E-15,0.));
#32220=DIRECTION('ref_axis',(3.56799717200074E-15,-1.,0.));
#32221=DIRECTION('',(3.56799717200074E-15,-1.,0.));
#32222=DIRECTION('',(0.,0.,1.));
#32223=DIRECTION('center_axis',(-0.500000000000001,0.866025403784438,0.));
#32224=DIRECTION('ref_axis',(-0.866025403784438,-0.500000000000001,0.));
#32225=DIRECTION('',(-0.866025403784438,-0.500000000000001,0.));
#32226=DIRECTION('center_axis',(0.,0.,1.));
#32227=DIRECTION('ref_axis',(1.,0.,0.));
#32228=DIRECTION('center_axis',(0.,0.923879532511288,-0.382683432365087));
#32229=DIRECTION('ref_axis',(0.,0.382683432365087,0.923879532511288));
#32230=DIRECTION('center_axis',(0.,0.923879532511288,-0.382683432365087));
#32231=DIRECTION('ref_axis',(0.,0.382683432365087,0.923879532511288));
#32232=DIRECTION('center_axis',(0.,0.923879532511288,-0.382683432365087));
#32233=DIRECTION('ref_axis',(1.22464679914735E-16,-0.382683432365087,-0.923879532511288));
#32234=DIRECTION('center_axis',(0.,0.923879532511288,-0.382683432365087));
#32235=DIRECTION('ref_axis',(0.,0.382683432365087,0.923879532511288));
#32236=DIRECTION('center_axis',(0.,0.923879532511288,-0.382683432365087));
#32237=DIRECTION('ref_axis',(0.,0.382683432365087,0.923879532511288));
#32238=DIRECTION('center_axis',(0.,-0.923879532511288,0.382683432365087));
#32239=DIRECTION('ref_axis',(0.,-0.382683432365087,-0.923879532511288));
#32240=DIRECTION('center_axis',(0.,-0.923879532511288,0.382683432365087));
#32241=DIRECTION('ref_axis',(0.,-0.382683432365087,-0.923879532511288));
#32242=DIRECTION('center_axis',(0.,-0.923879532511288,0.382683432365087));
#32243=DIRECTION('ref_axis',(-7.6571373978539E-16,0.382683432365087,0.923879532511288));
#32244=DIRECTION('center_axis',(0.,-0.923879532511288,0.382683432365087));
#32245=DIRECTION('ref_axis',(0.,-0.382683432365087,-0.923879532511288));
#32246=DIRECTION('center_axis',(0.,-0.923879532511288,0.382683432365087));
#32247=DIRECTION('ref_axis',(0.,-0.382683432365087,-0.923879532511288));
#32248=DIRECTION('center_axis',(-0.5,-0.331413574035589,-0.800103145191266));
#32249=DIRECTION('ref_axis',(-0.84802901144343,6.89411318440465E-18,0.529949804934655));
#32250=DIRECTION('',(0.,0.923879532511288,-0.382683432365087));
#32251=DIRECTION('',(0.,0.923879532511288,-0.382683432365087));
#32252=DIRECTION('center_axis',(-1.,4.14906208744436E-17,1.00167219626363E-16));
#32253=DIRECTION('ref_axis',(1.00167219626363E-16,0.,1.));
#32254=DIRECTION('',(0.,0.923879532511288,-0.382683432365087));
#32255=DIRECTION('center_axis',(-0.5,0.331413574035589,0.800103145191267));
#32256=DIRECTION('ref_axis',(0.848029011443431,-1.03411697766071E-17,0.529949804934654));
#32257=DIRECTION('',(0.,0.923879532511288,-0.382683432365087));
#32258=DIRECTION('center_axis',(0.5,0.331413574035589,0.800103145191267));
#32259=DIRECTION('ref_axis',(0.84802901144343,-3.44705659220234E-18,-0.529949804934655));
#32260=DIRECTION('',(0.,0.923879532511288,-0.382683432365087));
#32261=DIRECTION('center_axis',(1.,0.,0.));
#32262=DIRECTION('ref_axis',(0.,0.,-1.));
#32263=DIRECTION('',(0.,0.923879532511288,-0.382683432365087));
#32264=DIRECTION('center_axis',(0.499999999999999,-0.33141357403559,-0.800103145191267));
#32265=DIRECTION('ref_axis',(-0.848029011443431,5.08102344929861E-18,-0.529949804934654));
#32266=DIRECTION('center_axis',(-6.99485272571294E-17,-0.923879532511288,
0.382683432365087));
#32267=DIRECTION('ref_axis',(-2.37033238942555E-33,-0.382683432365087,-0.923879532511288));
#32268=DIRECTION('',(-1.51929083932157E-64,2.73691106313441E-48,1.));
#32269=DIRECTION('',(1.,-1.23259516440783E-32,1.51929083932157E-64));
#32270=DIRECTION('',(-1.51929083932157E-64,2.73691106313441E-48,1.));
#32271=DIRECTION('',(1.,-1.23259516440783E-32,1.51929083932157E-64));
#32272=DIRECTION('',(5.9178164074168E-18,2.46519032881566E-32,-1.));
#32273=DIRECTION('',(-1.38777878078087E-17,1.,2.45697770877689E-32));
#32274=DIRECTION('',(-1.51929083932157E-64,2.73691106313441E-48,1.));
#32275=DIRECTION('',(1.,-1.23259516440783E-32,1.51929083932157E-64));
#32276=DIRECTION('',(4.16333634234434E-17,-4.16333634234433E-17,-1.));
#32277=DIRECTION('',(-5.55111512312523E-17,1.,-4.16333634234433E-17));
#32278=DIRECTION('',(-1.51929083932157E-64,2.73691106313441E-48,1.));
#32279=DIRECTION('',(1.,-1.23259516440783E-32,1.51929083932157E-64));
#32280=DIRECTION('',(-1.51929083932157E-64,2.73691106313441E-48,1.));
#32281=DIRECTION('',(1.,-1.23259516440783E-32,1.51929083932157E-64));
#32282=DIRECTION('',(5.9178164074168E-18,2.46519032881566E-32,-1.));
#32283=DIRECTION('',(-1.38777878078092E-17,1.,2.45697770877689E-32));
#32284=DIRECTION('',(-1.51929083932157E-64,2.73691106313441E-48,1.));
#32285=DIRECTION('',(1.,-1.23259516440783E-32,1.51929083932157E-64));
#32286=DIRECTION('',(4.16333634234434E-17,-4.16333634234433E-17,-1.));
#32287=DIRECTION('',(-5.55111512312523E-17,1.,-4.16333634234433E-17));
#32288=DIRECTION('axis',(0.,0.,1.));
#32289=DIRECTION('refdir',(1.,0.,0.));
#32290=DIRECTION('axis',(0.,0.,1.));
#32291=DIRECTION('refdir',(1.,0.,0.));
#32292=DIRECTION('center_axis',(-1.,0.,0.));
#32293=DIRECTION('ref_axis',(0.,0.,1.));
#32294=DIRECTION('center_axis',(-1.,0.,0.));
#32295=DIRECTION('ref_axis',(0.,0.,1.));
#32296=DIRECTION('',(1.,0.,0.));
#32297=DIRECTION('center_axis',(-1.,0.,0.));
#32298=DIRECTION('ref_axis',(0.,0.,1.));
#32299=DIRECTION('',(-1.,0.,0.));
#32300=DIRECTION('',(1.,0.,0.));
#32301=DIRECTION('center_axis',(-1.,0.,0.));
#32302=DIRECTION('ref_axis',(0.,0.,1.));
#32303=DIRECTION('center_axis',(-1.,0.,0.));
#32304=DIRECTION('ref_axis',(0.,0.,1.));
#32305=DIRECTION('center_axis',(-1.,0.,0.));
#32306=DIRECTION('ref_axis',(0.,0.,1.));
#32307=DIRECTION('center_axis',(0.,1.,-1.22464679914735E-16));
#32308=DIRECTION('ref_axis',(0.,-1.22464679914735E-16,-1.));
#32309=DIRECTION('center_axis',(-1.,0.,0.));
#32310=DIRECTION('ref_axis',(0.,0.,1.));
#32311=DIRECTION('center_axis',(-1.,0.,0.));
#32312=DIRECTION('ref_axis',(0.,0.,1.));
#32313=DIRECTION('',(0.707106781186571,8.65956056235465E-17,0.707106781186524));
#32314=DIRECTION('center_axis',(-1.,0.,0.));
#32315=DIRECTION('ref_axis',(0.,0.,1.));
#32316=DIRECTION('center_axis',(-1.,0.,0.));
#32317=DIRECTION('ref_axis',(0.,0.,1.));
#32318=DIRECTION('center_axis',(-1.,0.,0.));
#32319=DIRECTION('ref_axis',(0.,0.,1.));
#32320=DIRECTION('',(1.,0.,0.));
#32321=DIRECTION('center_axis',(-1.,0.,0.));
#32322=DIRECTION('ref_axis',(0.,0.,1.));
#32323=DIRECTION('center_axis',(-1.,0.,0.));
#32324=DIRECTION('ref_axis',(0.,0.,1.));
#32325=DIRECTION('center_axis',(0.,1.,-1.22464679914735E-16));
#32326=DIRECTION('ref_axis',(0.,-1.22464679914735E-16,-1.));
#32327=DIRECTION('center_axis',(-1.,0.,0.));
#32328=DIRECTION('ref_axis',(0.,0.,1.));
#32329=DIRECTION('center_axis',(-1.,0.,0.));
#32330=DIRECTION('ref_axis',(0.,0.,1.));
#32331=DIRECTION('',(0.707106781186548,8.65956056235492E-17,0.707106781186547));
#32332=DIRECTION('center_axis',(-1.,0.,0.));
#32333=DIRECTION('ref_axis',(0.,0.,1.));
#32334=DIRECTION('center_axis',(-1.,0.,0.));
#32335=DIRECTION('ref_axis',(0.,0.,1.));
#32336=DIRECTION('center_axis',(-1.,0.,0.));
#32337=DIRECTION('ref_axis',(0.,0.,1.));
#32338=DIRECTION('center_axis',(-1.,0.,0.));
#32339=DIRECTION('ref_axis',(0.,0.,1.));
#32340=DIRECTION('',(1.,0.,0.));
#32341=DIRECTION('center_axis',(1.,0.,0.));
#32342=DIRECTION('ref_axis',(0.,0.,-1.));
#32343=DIRECTION('',(-0.707106781186594,8.65956056235436E-17,-0.707106781186501));
#32344=DIRECTION('center_axis',(-1.,0.,0.));
#32345=DIRECTION('ref_axis',(0.,0.,1.));
#32346=DIRECTION('center_axis',(-1.,0.,0.));
#32347=DIRECTION('ref_axis',(0.,0.,1.));
#32348=DIRECTION('center_axis',(-1.,0.,0.));
#32349=DIRECTION('ref_axis',(0.,0.,1.));
#32350=DIRECTION('center_axis',(0.,1.,-1.22464679914735E-16));
#32351=DIRECTION('ref_axis',(0.,-1.22464679914735E-16,-1.));
#32352=DIRECTION('center_axis',(-1.,0.,0.));
#32353=DIRECTION('ref_axis',(0.,0.,1.));
#32354=DIRECTION('center_axis',(-1.,0.,0.));
#32355=DIRECTION('ref_axis',(0.,0.,1.));
#32356=DIRECTION('center_axis',(-1.,0.,0.));
#32357=DIRECTION('ref_axis',(0.,0.,1.));
#32358=DIRECTION('',(1.,0.,0.));
#32359=DIRECTION('center_axis',(-1.,0.,0.));
#32360=DIRECTION('ref_axis',(0.,0.,1.));
#32361=DIRECTION('center_axis',(-1.,0.,0.));
#32362=DIRECTION('ref_axis',(0.,0.,1.));
#32363=DIRECTION('',(1.,0.,0.));
#32364=DIRECTION('center_axis',(-1.,0.,0.));
#32365=DIRECTION('ref_axis',(0.,0.,1.));
#32366=DIRECTION('center_axis',(-1.,0.,0.));
#32367=DIRECTION('ref_axis',(0.,0.,1.));
#32368=DIRECTION('center_axis',(-1.,0.,0.));
#32369=DIRECTION('ref_axis',(0.,0.,1.));
#32370=DIRECTION('center_axis',(-1.,0.,0.));
#32371=DIRECTION('ref_axis',(0.,0.,1.));
#32372=DIRECTION('',(1.,0.,0.));
#32373=DIRECTION('center_axis',(-1.,0.,0.));
#32374=DIRECTION('ref_axis',(0.,0.,1.));
#32375=DIRECTION('center_axis',(1.,0.,0.));
#32376=DIRECTION('ref_axis',(0.,0.,-1.));
#32377=DIRECTION('',(-0.707106781186547,8.65956056235493E-17,-0.707106781186547));
#32378=DIRECTION('center_axis',(-1.,0.,0.));
#32379=DIRECTION('ref_axis',(0.,0.,1.));
#32380=DIRECTION('center_axis',(-1.,0.,0.));
#32381=DIRECTION('ref_axis',(0.,0.,1.));
#32382=DIRECTION('center_axis',(1.,0.,0.));
#32383=DIRECTION('ref_axis',(0.,0.,-1.));
#32384=DIRECTION('center_axis',(1.,0.,0.));
#32385=DIRECTION('ref_axis',(0.,0.,-1.));
#32386=DIRECTION('center_axis',(-1.,0.,0.));
#32387=DIRECTION('ref_axis',(0.,0.,1.));
#32388=DIRECTION('center_axis',(-1.,0.,0.));
#32389=DIRECTION('ref_axis',(0.,0.,1.));
#32390=DIRECTION('center_axis',(-1.,0.,0.));
#32391=DIRECTION('ref_axis',(0.,-3.21624529935327E-16,-1.));
#32392=DIRECTION('center_axis',(-1.,0.,0.));
#32393=DIRECTION('ref_axis',(0.,0.,1.));
#32394=DIRECTION('center_axis',(-1.,0.,0.));
#32395=DIRECTION('ref_axis',(0.,0.,1.));
#32396=DIRECTION('',(0.,1.73472347597681E-16,1.));
#32397=DIRECTION('',(0.,1.,-2.16840434497101E-16));
#32398=DIRECTION('',(0.,-3.46944695195362E-16,1.));
#32399=DIRECTION('center_axis',(1.,0.,0.));
#32400=DIRECTION('ref_axis',(0.,0.,-1.));
#32401=DIRECTION('center_axis',(0.,1.,-1.73472347597681E-16));
#32402=DIRECTION('ref_axis',(0.,1.73472347597681E-16,1.));
#32403=DIRECTION('',(0.,-1.73472347597681E-16,-1.));
#32404=DIRECTION('',(1.,0.,0.));
#32405=DIRECTION('center_axis',(0.,-1.,-3.46944695195362E-16));
#32406=DIRECTION('ref_axis',(0.,3.46944695195362E-16,-1.));
#32407=DIRECTION('',(1.,0.,0.));
#32408=DIRECTION('',(0.,-3.46944695195362E-16,1.));
#32409=DIRECTION('center_axis',(0.,-2.16840434497101E-16,-1.));
#32410=DIRECTION('ref_axis',(0.,1.,-2.16840434497101E-16));
#32411=DIRECTION('center_axis',(0.,2.16840434497101E-16,1.));
#32412=DIRECTION('ref_axis',(0.,1.,-2.16840434497101E-16));
#32413=DIRECTION('center_axis',(0.,-1.73472347597681E-16,-1.));
#32414=DIRECTION('ref_axis',(0.,1.,-1.73472347597681E-16));
#32415=DIRECTION('axis',(0.,0.,1.));
#32416=DIRECTION('refdir',(1.,0.,0.));
#32417=DIRECTION('center_axis',(0.,-0.923879532511287,-0.382683432365091));
#32418=DIRECTION('ref_axis',(0.,0.382683432365091,-0.923879532511286));
#32419=DIRECTION('',(0.,-0.923879532511286,-0.382683432365091));
#32420=DIRECTION('center_axis',(1.,0.,0.));
#32421=DIRECTION('ref_axis',(0.,0.,-1.));
#32422=DIRECTION('center_axis',(1.,0.,0.));
#32423=DIRECTION('ref_axis',(0.,0.,-1.));
#32424=DIRECTION('',(1.,0.,0.));
#32425=DIRECTION('center_axis',(1.,0.,0.));
#32426=DIRECTION('ref_axis',(0.,0.,-1.));
#32427=DIRECTION('center_axis',(1.,0.,0.));
#32428=DIRECTION('ref_axis',(0.,0.,-1.));
#32429=DIRECTION('center_axis',(1.,0.,0.));
#32430=DIRECTION('ref_axis',(0.,0.,-1.));
#32431=DIRECTION('',(1.,0.,0.));
#32432=DIRECTION('center_axis',(1.,0.,0.));
#32433=DIRECTION('ref_axis',(0.,0.,-1.));
#32434=DIRECTION('center_axis',(1.,0.,0.));
#32435=DIRECTION('ref_axis',(0.,0.,-1.));
#32436=DIRECTION('center_axis',(1.,0.,0.));
#32437=DIRECTION('ref_axis',(0.,0.,-1.));
#32438=DIRECTION('',(1.,0.,0.));
#32439=DIRECTION('center_axis',(1.,0.,0.));
#32440=DIRECTION('ref_axis',(0.,0.,-1.));
#32441=DIRECTION('center_axis',(1.,0.,0.));
#32442=DIRECTION('ref_axis',(0.,0.,-1.));
#32443=DIRECTION('center_axis',(1.,0.,0.));
#32444=DIRECTION('ref_axis',(0.,0.,-1.));
#32445=DIRECTION('',(1.,0.,0.));
#32446=DIRECTION('center_axis',(1.,0.,0.));
#32447=DIRECTION('ref_axis',(0.,0.,-1.));
#32448=DIRECTION('center_axis',(1.,0.,0.));
#32449=DIRECTION('ref_axis',(0.,0.,-1.));
#32450=DIRECTION('center_axis',(1.,0.,0.));
#32451=DIRECTION('ref_axis',(0.,0.,-1.));
#32452=DIRECTION('',(1.,0.,0.));
#32453=DIRECTION('center_axis',(1.,0.,0.));
#32454=DIRECTION('ref_axis',(0.,0.,-1.));
#32455=DIRECTION('center_axis',(1.,0.,0.));
#32456=DIRECTION('ref_axis',(0.,0.,-1.));
#32457=DIRECTION('center_axis',(1.,0.,0.));
#32458=DIRECTION('ref_axis',(0.,0.,-1.));
#32459=DIRECTION('',(1.,0.,0.));
#32460=DIRECTION('center_axis',(1.,0.,0.));
#32461=DIRECTION('ref_axis',(0.,0.,-1.));
#32462=DIRECTION('center_axis',(-1.,0.,0.));
#32463=DIRECTION('ref_axis',(0.,0.,1.));
#32464=DIRECTION('center_axis',(-1.,0.,0.));
#32465=DIRECTION('ref_axis',(0.,0.,1.));
#32466=DIRECTION('',(1.,0.,0.));
#32467=DIRECTION('center_axis',(-1.,0.,0.));
#32468=DIRECTION('ref_axis',(0.,0.,1.));
#32469=DIRECTION('center_axis',(-1.,0.,0.));
#32470=DIRECTION('ref_axis',(0.,0.,1.));
#32471=DIRECTION('center_axis',(-1.,0.,0.));
#32472=DIRECTION('ref_axis',(0.,0.,1.));
#32473=DIRECTION('',(-1.,0.,0.));
#32474=DIRECTION('center_axis',(-1.,0.,0.));
#32475=DIRECTION('ref_axis',(0.,0.,1.));
#32476=DIRECTION('center_axis',(-1.,0.,0.));
#32477=DIRECTION('ref_axis',(0.,0.,1.));
#32478=DIRECTION('center_axis',(-1.,0.,0.));
#32479=DIRECTION('ref_axis',(0.,0.,1.));
#32480=DIRECTION('',(1.,0.,0.));
#32481=DIRECTION('center_axis',(-1.,0.,0.));
#32482=DIRECTION('ref_axis',(0.,0.,1.));
#32483=DIRECTION('center_axis',(-1.,0.,0.));
#32484=DIRECTION('ref_axis',(0.,0.,1.));
#32485=DIRECTION('center_axis',(-1.,0.,0.));
#32486=DIRECTION('ref_axis',(0.,0.,1.));
#32487=DIRECTION('',(-1.,0.,0.));
#32488=DIRECTION('center_axis',(-1.,0.,0.));
#32489=DIRECTION('ref_axis',(0.,0.,1.));
#32490=DIRECTION('center_axis',(-1.,0.,0.));
#32491=DIRECTION('ref_axis',(0.,0.,1.));
#32492=DIRECTION('center_axis',(-1.,0.,0.));
#32493=DIRECTION('ref_axis',(0.,0.,1.));
#32494=DIRECTION('',(1.,0.,0.));
#32495=DIRECTION('center_axis',(-1.,0.,0.));
#32496=DIRECTION('ref_axis',(0.,0.,1.));
#32497=DIRECTION('center_axis',(-1.,0.,0.));
#32498=DIRECTION('ref_axis',(0.,0.,1.));
#32499=DIRECTION('center_axis',(-1.,0.,0.));
#32500=DIRECTION('ref_axis',(0.,0.,1.));
#32501=DIRECTION('',(-1.,0.,0.));
#32502=DIRECTION('center_axis',(-1.,0.,0.));
#32503=DIRECTION('ref_axis',(0.,0.,1.));
#32504=DIRECTION('center_axis',(-1.,0.,0.));
#32505=DIRECTION('ref_axis',(0.,0.,1.));
#32506=DIRECTION('center_axis',(-1.,0.,0.));
#32507=DIRECTION('ref_axis',(0.,0.,1.));
#32508=DIRECTION('center_axis',(0.,-1.,1.22464679914735E-16));
#32509=DIRECTION('ref_axis',(0.,-1.22464679914735E-16,-1.));
#32510=DIRECTION('center_axis',(-1.,0.,0.));
#32511=DIRECTION('ref_axis',(0.,0.,1.));
#32512=DIRECTION('',(0.,-1.,1.19636101791504E-16));
#32513=DIRECTION('center_axis',(-1.,0.,0.));
#32514=DIRECTION('ref_axis',(0.,0.,1.));
#32515=DIRECTION('',(0.,1.,1.19636101791504E-16));
#32516=DIRECTION('center_axis',(-1.,0.,0.));
#32517=DIRECTION('ref_axis',(0.,0.,1.));
#32518=DIRECTION('center_axis',(-1.,0.,0.));
#32519=DIRECTION('ref_axis',(0.,0.,1.));
#32520=DIRECTION('center_axis',(-1.,0.,0.));
#32521=DIRECTION('ref_axis',(0.,0.,1.));
#32522=DIRECTION('center_axis',(-1.,0.,0.));
#32523=DIRECTION('ref_axis',(0.,0.,1.));
#32524=DIRECTION('center_axis',(-1.,0.,0.));
#32525=DIRECTION('ref_axis',(0.,0.,1.));
#32526=DIRECTION('center_axis',(-1.,0.,0.));
#32527=DIRECTION('ref_axis',(0.,0.,1.));
#32528=DIRECTION('',(1.,0.,0.));
#32529=DIRECTION('center_axis',(-1.,0.,0.));
#32530=DIRECTION('ref_axis',(0.,0.,1.));
#32531=DIRECTION('',(-1.,0.,0.));
#32532=DIRECTION('center_axis',(-1.,0.,0.));
#32533=DIRECTION('ref_axis',(0.,0.,1.));
#32534=DIRECTION('',(-1.,0.,0.));
#32535=DIRECTION('',(1.,0.,0.));
#32536=DIRECTION('center_axis',(-1.,0.,0.));
#32537=DIRECTION('ref_axis',(0.,0.,1.));
#32538=DIRECTION('center_axis',(-1.,0.,0.));
#32539=DIRECTION('ref_axis',(0.,0.,1.));
#32540=DIRECTION('center_axis',(-1.,0.,0.));
#32541=DIRECTION('ref_axis',(0.,0.,1.));
#32542=DIRECTION('center_axis',(-1.,0.,0.));
#32543=DIRECTION('ref_axis',(0.,0.,1.));
#32544=DIRECTION('center_axis',(-1.,0.,0.));
#32545=DIRECTION('ref_axis',(0.,0.,1.));
#32546=DIRECTION('center_axis',(1.,0.,0.));
#32547=DIRECTION('ref_axis',(0.,0.,-1.));
#32548=DIRECTION('',(0.,-1.,1.19636101791504E-16));
#32549=DIRECTION('',(0.,1.,1.19636101791504E-16));
#32550=DIRECTION('center_axis',(1.,0.,0.));
#32551=DIRECTION('ref_axis',(0.,0.,-1.));
#32552=DIRECTION('center_axis',(1.,0.,0.));
#32553=DIRECTION('ref_axis',(0.,0.,-1.));
#32554=DIRECTION('center_axis',(1.,0.,0.));
#32555=DIRECTION('ref_axis',(0.,0.,-1.));
#32556=DIRECTION('center_axis',(-1.,0.,0.));
#32557=DIRECTION('ref_axis',(0.,0.,1.));
#32558=DIRECTION('center_axis',(-1.,0.,0.));
#32559=DIRECTION('ref_axis',(0.,0.,1.));
#32560=DIRECTION('center_axis',(0.,1.19636101791504E-16,-1.));
#32561=DIRECTION('ref_axis',(0.,1.,1.19636101791504E-16));
#32562=DIRECTION('center_axis',(0.,1.19636101791504E-16,1.));
#32563=DIRECTION('ref_axis',(0.,-1.,1.19636101791504E-16));
#32564=DIRECTION('',(-1.11022302462516E-16,-2.26524128016684E-16,1.));
#32565=DIRECTION('',(1.,-1.71458653683646E-16,1.11022302462516E-16));
#32566=DIRECTION('',(-1.11022302462516E-16,-2.26524128016684E-16,1.));
#32567=DIRECTION('',(1.,-1.71458653683646E-16,1.11022302462516E-16));
#32568=DIRECTION('axis',(0.,0.,1.));
#32569=DIRECTION('refdir',(1.,0.,0.));
#32570=DIRECTION('axis',(0.,0.,1.));
#32571=DIRECTION('refdir',(1.,0.,0.));
#32572=DIRECTION('center_axis',(1.,1.73472347597681E-16,0.));
#32573=DIRECTION('ref_axis',(-1.73472347597681E-16,1.,0.));
#32574=DIRECTION('center_axis',(1.,1.73472347597681E-16,0.));
#32575=DIRECTION('ref_axis',(-1.73472347597681E-16,1.,0.));
#32576=DIRECTION('',(1.,1.73472347597681E-16,0.));
#32577=DIRECTION('center_axis',(1.,1.73472347597681E-16,0.));
#32578=DIRECTION('ref_axis',(-1.73472347597681E-16,1.,0.));
#32579=DIRECTION('center_axis',(1.,1.73472347597681E-16,0.));
#32580=DIRECTION('ref_axis',(-1.73472347597681E-16,1.,0.));
#32581=DIRECTION('center_axis',(1.,1.73472347597681E-16,0.));
#32582=DIRECTION('ref_axis',(-1.73472347597681E-16,1.,0.));
#32583=DIRECTION('',(1.,1.73472347597681E-16,0.));
#32584=DIRECTION('center_axis',(1.,1.73472347597681E-16,0.));
#32585=DIRECTION('ref_axis',(-1.73472347597681E-16,1.,0.));
#32586=DIRECTION('center_axis',(1.,1.73472347597681E-16,0.));
#32587=DIRECTION('ref_axis',(-1.73472347597681E-16,1.,0.));
#32588=DIRECTION('center_axis',(1.,1.73472347597681E-16,0.));
#32589=DIRECTION('ref_axis',(-1.73472347597681E-16,1.,0.));
#32590=DIRECTION('',(1.,1.73472347597681E-16,0.));
#32591=DIRECTION('center_axis',(1.,1.73472347597681E-16,0.));
#32592=DIRECTION('ref_axis',(-1.73472347597681E-16,1.,0.));
#32593=DIRECTION('center_axis',(0.,1.,0.));
#32594=DIRECTION('ref_axis',(0.,0.,1.));
#32595=DIRECTION('center_axis',(0.,1.,0.));
#32596=DIRECTION('ref_axis',(0.,0.,1.));
#32597=DIRECTION('',(0.,1.,0.));
#32598=DIRECTION('center_axis',(0.,1.,0.));
#32599=DIRECTION('ref_axis',(0.,0.,1.));
#32600=DIRECTION('center_axis',(0.,1.,0.));
#32601=DIRECTION('ref_axis',(0.,0.,1.));
#32602=DIRECTION('center_axis',(0.,1.,0.));
#32603=DIRECTION('ref_axis',(0.,0.,1.));
#32604=DIRECTION('',(0.,1.,0.));
#32605=DIRECTION('center_axis',(0.,1.,0.));
#32606=DIRECTION('ref_axis',(0.,0.,1.));
#32607=DIRECTION('center_axis',(0.,1.,0.));
#32608=DIRECTION('ref_axis',(0.,0.,1.));
#32609=DIRECTION('center_axis',(0.,1.,0.));
#32610=DIRECTION('ref_axis',(0.,0.,1.));
#32611=DIRECTION('',(0.,1.,0.));
#32612=DIRECTION('center_axis',(0.,1.,0.));
#32613=DIRECTION('ref_axis',(0.,0.,1.));
#32614=DIRECTION('center_axis',(0.,1.,0.));
#32615=DIRECTION('ref_axis',(0.,0.,1.));
#32616=DIRECTION('center_axis',(0.,1.,0.));
#32617=DIRECTION('ref_axis',(0.,0.,1.));
#32618=DIRECTION('',(0.,1.,0.));
#32619=DIRECTION('center_axis',(0.,1.,0.));
#32620=DIRECTION('ref_axis',(0.,0.,1.));
#32621=DIRECTION('center_axis',(0.,-1.,-4.78544407166016E-16));
#32622=DIRECTION('ref_axis',(0.,4.78544407166016E-16,-1.));
#32623=DIRECTION('',(0.,-4.78544407166016E-16,1.));
#32624=DIRECTION('',(-1.,0.,0.));
#32625=DIRECTION('',(0.,-4.78544407166016E-16,1.));
#32626=DIRECTION('',(-1.,0.,0.));
#32627=DIRECTION('center_axis',(0.,-0.707106781186528,-0.707106781186567));
#32628=DIRECTION('ref_axis',(0.,0.707106781186567,-0.707106781186528));
#32629=DIRECTION('',(0.,-0.707106781186567,0.707106781186528));
#32630=DIRECTION('',(-1.,0.,0.));
#32631=DIRECTION('',(0.,-0.707106781186567,0.707106781186528));
#32632=DIRECTION('center_axis',(0.,3.70074341541719E-16,-1.));
#32633=DIRECTION('ref_axis',(0.,1.,3.70074341541719E-16));
#32634=DIRECTION('',(0.,-1.,-3.70074341541719E-16));
#32635=DIRECTION('',(-1.,0.,0.));
#32636=DIRECTION('',(0.,-1.,-3.70074341541719E-16));
#32637=DIRECTION('center_axis',(0.,1.,3.11362923006336E-16));
#32638=DIRECTION('ref_axis',(0.,-3.11362923006336E-16,1.));
#32639=DIRECTION('',(0.,3.11362923006336E-16,-1.));
#32640=DIRECTION('',(-1.,0.,0.));
#32641=DIRECTION('',(0.,3.11362923006336E-16,-1.));
#32642=DIRECTION('center_axis',(0.,-5.55111512312579E-16,1.));
#32643=DIRECTION('ref_axis',(0.,-1.,-5.55111512312579E-16));
#32644=DIRECTION('',(0.,1.,5.55111512312579E-16));
#32645=DIRECTION('',(-1.,0.,0.));
#32646=DIRECTION('',(0.,1.,5.55111512312579E-16));
#32647=DIRECTION('center_axis',(0.,-0.707106781186538,0.707106781186557));
#32648=DIRECTION('ref_axis',(0.,-0.707106781186557,-0.707106781186538));
#32649=DIRECTION('',(0.,0.707106781186557,0.707106781186538));
#32650=DIRECTION('',(-1.,0.,0.));
#32651=DIRECTION('',(0.,0.707106781186557,0.707106781186538));
#32652=DIRECTION('center_axis',(0.,-1.,-4.78544407166016E-16));
#32653=DIRECTION('ref_axis',(0.,4.78544407166016E-16,-1.));
#32654=DIRECTION('',(0.,-4.78544407166016E-16,1.));
#32655=DIRECTION('',(-1.,0.,0.));
#32656=DIRECTION('',(0.,-4.78544407166016E-16,1.));
#32657=DIRECTION('center_axis',(0.,0.,1.));
#32658=DIRECTION('ref_axis',(1.,0.,0.));
#32659=DIRECTION('',(0.,1.,0.));
#32660=DIRECTION('',(-1.,0.,0.));
#32661=DIRECTION('',(0.,1.,0.));
#32662=DIRECTION('center_axis',(0.,-0.707106781186548,0.707106781186548));
#32663=DIRECTION('ref_axis',(0.,-0.707106781186548,-0.707106781186548));
#32664=DIRECTION('',(0.,0.707106781186547,0.707106781186547));
#32665=DIRECTION('',(-1.,0.,0.));
#32666=DIRECTION('',(0.,0.707106781186547,0.707106781186547));
#32667=DIRECTION('center_axis',(0.,-1.,1.77920356510442E-16));
#32668=DIRECTION('ref_axis',(0.,-1.77920356510442E-16,-1.));
#32669=DIRECTION('',(0.,1.77920356510442E-16,1.));
#32670=DIRECTION('',(-1.,0.,0.));
#32671=DIRECTION('',(0.,1.77920356510442E-16,1.));
#32672=DIRECTION('center_axis',(0.,-0.707106781186548,-0.707106781186548));
#32673=DIRECTION('ref_axis',(0.,0.707106781186548,-0.707106781186548));
#32674=DIRECTION('',(0.,-0.707106781186547,0.707106781186547));
#32675=DIRECTION('',(-1.,0.,0.));
#32676=DIRECTION('',(0.,-0.707106781186547,0.707106781186547));
#32677=DIRECTION('center_axis',(0.,3.65204942310907E-16,-1.));
#32678=DIRECTION('ref_axis',(0.,1.,3.65204942310907E-16));
#32679=DIRECTION('',(0.,-1.,-3.65204942310907E-16));
#32680=DIRECTION('',(0.,-1.,-3.65204942310907E-16));
#32681=DIRECTION('center_axis',(1.,0.,0.));
#32682=DIRECTION('ref_axis',(0.,0.,-1.));
#32683=DIRECTION('center_axis',(1.,0.,0.));
#32684=DIRECTION('ref_axis',(0.,0.,-1.));
#32685=DIRECTION('center_axis',(0.,-1.,0.));
#32686=DIRECTION('ref_axis',(0.,0.,-1.));
#32687=DIRECTION('center_axis',(0.,-1.,0.));
#32688=DIRECTION('ref_axis',(0.,0.,-1.));
#32689=DIRECTION('center_axis',(1.,1.73472347597681E-16,0.));
#32690=DIRECTION('ref_axis',(-1.73472347597681E-16,1.,0.));
#32691=DIRECTION('center_axis',(-1.,-1.73472347597681E-16,0.));
#32692=DIRECTION('ref_axis',(1.73472347597681E-16,-1.,0.));
#32693=DIRECTION('axis',(0.,0.,1.));
#32694=DIRECTION('refdir',(1.,0.,0.));
#32695=DIRECTION('center_axis',(-1.,0.,0.));
#32696=DIRECTION('ref_axis',(0.,0.,1.));
#32697=DIRECTION('center_axis',(1.,0.,0.));
#32698=DIRECTION('ref_axis',(0.,0.,-1.));
#32699=DIRECTION('',(-1.,0.,0.));
#32700=DIRECTION('center_axis',(1.,0.,0.));
#32701=DIRECTION('ref_axis',(0.,0.,-1.));
#32702=DIRECTION('center_axis',(-1.,0.,0.));
#32703=DIRECTION('ref_axis',(0.,0.,1.));
#32704=DIRECTION('center_axis',(1.,0.,0.));
#32705=DIRECTION('ref_axis',(0.,0.,-1.));
#32706=DIRECTION('',(-1.,0.,0.));
#32707=DIRECTION('center_axis',(1.,0.,0.));
#32708=DIRECTION('ref_axis',(0.,0.,-1.));
#32709=DIRECTION('center_axis',(-1.,0.,0.));
#32710=DIRECTION('ref_axis',(0.,1.,6.12323399573677E-17));
#32711=DIRECTION('center_axis',(-1.,0.,0.));
#32712=DIRECTION('ref_axis',(0.,0.,-1.));
#32713=DIRECTION('',(-1.,0.,0.));
#32714=DIRECTION('center_axis',(-1.,0.,0.));
#32715=DIRECTION('ref_axis',(0.,0.,-1.));
#32716=DIRECTION('',(-1.,0.,0.));
#32717=DIRECTION('center_axis',(-1.,0.,0.));
#32718=DIRECTION('ref_axis',(0.,1.,6.12323399573676E-17));
#32719=DIRECTION('center_axis',(1.,0.,0.));
#32720=DIRECTION('ref_axis',(0.,0.,-1.));
#32721=DIRECTION('',(-1.,0.,0.));
#32722=DIRECTION('center_axis',(1.,0.,0.));
#32723=DIRECTION('ref_axis',(0.,0.,-1.));
#32724=DIRECTION('',(-1.,0.,0.));
#32725=DIRECTION('center_axis',(1.,0.,0.));
#32726=DIRECTION('ref_axis',(0.,0.,-1.));
#32727=DIRECTION('',(0.,0.,-1.));
#32728=DIRECTION('center_axis',(1.,0.,0.));
#32729=DIRECTION('ref_axis',(0.,0.,-1.));
#32730=DIRECTION('',(0.,1.,0.));
#32731=DIRECTION('center_axis',(-1.,0.,0.));
#32732=DIRECTION('ref_axis',(0.,0.,-1.));
#32733=DIRECTION('center_axis',(-1.,0.,0.));
#32734=DIRECTION('ref_axis',(0.,0.,-1.));
#32735=DIRECTION('',(0.,-1.,0.));
#32736=DIRECTION('center_axis',(1.,0.,0.));
#32737=DIRECTION('ref_axis',(0.,0.,-1.));
#32738=DIRECTION('',(0.,0.,-1.));
#32739=DIRECTION('',(0.,1.,-1.23292219708887E-16));
#32740=DIRECTION('',(0.,-1.,-1.23292219708887E-16));
#32741=DIRECTION('center_axis',(1.,0.,0.));
#32742=DIRECTION('ref_axis',(0.,0.,-1.));
#32743=DIRECTION('',(0.,0.,-1.));
#32744=DIRECTION('',(0.,-1.,-1.23292219708887E-16));
#32745=DIRECTION('',(0.,1.,-1.23292219708887E-16));
#32746=DIRECTION('',(0.,0.,-1.));
#32747=DIRECTION('center_axis',(1.,0.,0.));
#32748=DIRECTION('ref_axis',(0.,0.,-1.));
#32749=DIRECTION('',(0.,-1.,0.));
#32750=DIRECTION('center_axis',(-1.,0.,0.));
#32751=DIRECTION('ref_axis',(0.,0.,-1.));
#32752=DIRECTION('center_axis',(-1.,0.,0.));
#32753=DIRECTION('ref_axis',(0.,0.,-1.));
#32754=DIRECTION('',(0.,1.,0.));
#32755=DIRECTION('center_axis',(1.,0.,0.));
#32756=DIRECTION('ref_axis',(0.,0.,-1.));
#32757=DIRECTION('center_axis',(0.,1.,0.));
#32758=DIRECTION('ref_axis',(0.,0.,1.));
#32759=DIRECTION('',(-1.,0.,0.));
#32760=DIRECTION('',(-1.,0.,0.));
#32761=DIRECTION('center_axis',(-1.,0.,0.));
#32762=DIRECTION('ref_axis',(0.,0.,1.));
#32763=DIRECTION('',(-1.,0.,0.));
#32764=DIRECTION('center_axis',(0.,0.,1.));
#32765=DIRECTION('ref_axis',(1.,0.,0.));
#32766=DIRECTION('',(-1.,0.,0.));
#32767=DIRECTION('center_axis',(-1.,0.,0.));
#32768=DIRECTION('ref_axis',(0.,0.,1.));
#32769=DIRECTION('center_axis',(-1.,0.,0.));
#32770=DIRECTION('ref_axis',(0.,0.,1.));
#32771=DIRECTION('',(-1.,0.,0.));
#32772=DIRECTION('center_axis',(0.,0.,-1.));
#32773=DIRECTION('ref_axis',(-1.,0.,0.));
#32774=DIRECTION('',(-1.,0.,0.));
#32775=DIRECTION('center_axis',(-1.,0.,0.));
#32776=DIRECTION('ref_axis',(0.,0.,1.));
#32777=DIRECTION('',(-1.,0.,0.));
#32778=DIRECTION('center_axis',(0.,1.,0.));
#32779=DIRECTION('ref_axis',(0.,0.,1.));
#32780=DIRECTION('',(-1.,0.,0.));
#32781=DIRECTION('center_axis',(0.,1.23292219708887E-16,1.));
#32782=DIRECTION('ref_axis',(0.,-1.,1.23292219708887E-16));
#32783=DIRECTION('center_axis',(0.,1.23292219708887E-16,-1.));
#32784=DIRECTION('ref_axis',(0.,1.,1.23292219708887E-16));
#32785=DIRECTION('',(0.,-4.04204547078273E-32,1.));
#32786=DIRECTION('',(1.,0.,0.));
#32787=DIRECTION('',(1.21430643318377E-16,1.09063073495803E-16,-1.));
#32788=DIRECTION('',(-1.,-6.54590493145538E-16,-1.21430643318377E-16));
#32789=DIRECTION('axis',(0.,0.,1.));
#32790=DIRECTION('refdir',(1.,0.,0.));
#32791=DIRECTION('axis',(0.,0.,1.));
#32792=DIRECTION('refdir',(1.,0.,0.));
#32793=DIRECTION('center_axis',(1.,0.,0.));
#32794=DIRECTION('ref_axis',(0.,0.,-1.));
#32795=DIRECTION('center_axis',(1.,0.,0.));
#32796=DIRECTION('ref_axis',(0.,0.,-1.));
#32797=DIRECTION('',(1.,0.,0.));
#32798=DIRECTION('center_axis',(1.,0.,0.));
#32799=DIRECTION('ref_axis',(0.,0.,-1.));
#32800=DIRECTION('center_axis',(1.,0.,0.));
#32801=DIRECTION('ref_axis',(0.,0.,-1.));
#32802=DIRECTION('center_axis',(1.,0.,0.));
#32803=DIRECTION('ref_axis',(0.,0.,-1.));
#32804=DIRECTION('',(1.,0.,0.));
#32805=DIRECTION('center_axis',(1.,0.,0.));
#32806=DIRECTION('ref_axis',(0.,0.,-1.));
#32807=DIRECTION('center_axis',(1.,0.,0.));
#32808=DIRECTION('ref_axis',(0.,0.,-1.));
#32809=DIRECTION('center_axis',(1.,0.,0.));
#32810=DIRECTION('ref_axis',(0.,0.,-1.));
#32811=DIRECTION('',(1.,0.,0.));
#32812=DIRECTION('center_axis',(1.,0.,0.));
#32813=DIRECTION('ref_axis',(0.,0.,-1.));
#32814=DIRECTION('center_axis',(1.,0.,0.));
#32815=DIRECTION('ref_axis',(0.,0.,-1.));
#32816=DIRECTION('center_axis',(1.,0.,0.));
#32817=DIRECTION('ref_axis',(0.,0.,-1.));
#32818=DIRECTION('',(1.,0.,0.));
#32819=DIRECTION('center_axis',(1.,0.,0.));
#32820=DIRECTION('ref_axis',(0.,0.,-1.));
#32821=DIRECTION('center_axis',(1.,0.,0.));
#32822=DIRECTION('ref_axis',(0.,0.,-1.));
#32823=DIRECTION('center_axis',(1.,0.,0.));
#32824=DIRECTION('ref_axis',(0.,0.,-1.));
#32825=DIRECTION('',(1.,0.,0.));
#32826=DIRECTION('center_axis',(1.,0.,0.));
#32827=DIRECTION('ref_axis',(0.,0.,-1.));
#32828=DIRECTION('center_axis',(-1.,0.,0.));
#32829=DIRECTION('ref_axis',(0.,0.,1.));
#32830=DIRECTION('center_axis',(1.,0.,0.));
#32831=DIRECTION('ref_axis',(0.,0.,-1.));
#32832=DIRECTION('',(1.,0.,0.));
#32833=DIRECTION('center_axis',(1.,0.,0.));
#32834=DIRECTION('ref_axis',(0.,0.,-1.));
#32835=DIRECTION('center_axis',(-1.,0.,0.));
#32836=DIRECTION('ref_axis',(0.,0.,1.));
#32837=DIRECTION('center_axis',(1.,0.,0.));
#32838=DIRECTION('ref_axis',(0.,0.,-1.));
#32839=DIRECTION('',(1.,0.,0.));
#32840=DIRECTION('center_axis',(1.,0.,0.));
#32841=DIRECTION('ref_axis',(0.,0.,-1.));
#32842=DIRECTION('center_axis',(-1.,0.,0.));
#32843=DIRECTION('ref_axis',(0.,0.,1.));
#32844=DIRECTION('center_axis',(1.,0.,0.));
#32845=DIRECTION('ref_axis',(0.,0.,-1.));
#32846=DIRECTION('',(1.,0.,0.));
#32847=DIRECTION('center_axis',(1.,0.,0.));
#32848=DIRECTION('ref_axis',(0.,0.,-1.));
#32849=DIRECTION('center_axis',(-1.,0.,0.));
#32850=DIRECTION('ref_axis',(0.,0.,1.));
#32851=DIRECTION('center_axis',(1.,0.,0.));
#32852=DIRECTION('ref_axis',(0.,0.,-1.));
#32853=DIRECTION('',(1.,0.,0.));
#32854=DIRECTION('center_axis',(1.,0.,0.));
#32855=DIRECTION('ref_axis',(0.,0.,-1.));
#32856=DIRECTION('center_axis',(-1.,0.,0.));
#32857=DIRECTION('ref_axis',(0.,0.,1.));
#32858=DIRECTION('center_axis',(1.,0.,0.));
#32859=DIRECTION('ref_axis',(0.,0.,-1.));
#32860=DIRECTION('',(-1.,0.,0.));
#32861=DIRECTION('center_axis',(-1.,0.,0.));
#32862=DIRECTION('ref_axis',(0.,0.,-1.));
#32863=DIRECTION('center_axis',(-1.,0.,0.));
#32864=DIRECTION('ref_axis',(0.,0.,1.));
#32865=DIRECTION('center_axis',(1.,0.,0.));
#32866=DIRECTION('ref_axis',(0.,0.,-1.));
#32867=DIRECTION('',(-1.,0.,0.));
#32868=DIRECTION('center_axis',(-1.,0.,0.));
#32869=DIRECTION('ref_axis',(0.,0.,-1.));
#32870=DIRECTION('center_axis',(-1.,0.,0.));
#32871=DIRECTION('ref_axis',(0.,0.,1.));
#32872=DIRECTION('center_axis',(1.,0.,0.));
#32873=DIRECTION('ref_axis',(0.,0.,-1.));
#32874=DIRECTION('',(-1.,0.,0.));
#32875=DIRECTION('center_axis',(-1.,0.,0.));
#32876=DIRECTION('ref_axis',(0.,0.,-1.));
#32877=DIRECTION('center_axis',(-1.,0.,0.));
#32878=DIRECTION('ref_axis',(0.,0.,1.));
#32879=DIRECTION('center_axis',(1.,0.,0.));
#32880=DIRECTION('ref_axis',(0.,0.,-1.));
#32881=DIRECTION('',(-1.,0.,0.));
#32882=DIRECTION('center_axis',(-1.,0.,0.));
#32883=DIRECTION('ref_axis',(0.,0.,-1.));
#32884=DIRECTION('center_axis',(0.,1.,0.));
#32885=DIRECTION('ref_axis',(0.,0.,1.));
#32886=DIRECTION('center_axis',(0.,1.,0.));
#32887=DIRECTION('ref_axis',(0.,0.,1.));
#32888=DIRECTION('',(0.,1.,0.));
#32889=DIRECTION('center_axis',(0.,1.,0.));
#32890=DIRECTION('ref_axis',(0.,0.,1.));
#32891=DIRECTION('center_axis',(0.,1.,0.));
#32892=DIRECTION('ref_axis',(0.,0.,1.));
#32893=DIRECTION('center_axis',(0.,1.,0.));
#32894=DIRECTION('ref_axis',(0.,0.,1.));
#32895=DIRECTION('',(0.,1.,0.));
#32896=DIRECTION('center_axis',(0.,1.,0.));
#32897=DIRECTION('ref_axis',(0.,0.,1.));
#32898=DIRECTION('center_axis',(0.,1.,0.));
#32899=DIRECTION('ref_axis',(0.,0.,1.));
#32900=DIRECTION('center_axis',(0.,1.,0.));
#32901=DIRECTION('ref_axis',(0.,0.,1.));
#32902=DIRECTION('',(0.,1.,0.));
#32903=DIRECTION('center_axis',(0.,1.,0.));
#32904=DIRECTION('ref_axis',(0.,0.,1.));
#32905=DIRECTION('center_axis',(0.,1.,0.));
#32906=DIRECTION('ref_axis',(0.,0.,1.));
#32907=DIRECTION('center_axis',(0.,1.,0.));
#32908=DIRECTION('ref_axis',(0.,0.,1.));
#32909=DIRECTION('',(0.,1.,0.));
#32910=DIRECTION('center_axis',(0.,1.,0.));
#32911=DIRECTION('ref_axis',(0.,0.,1.));
#32912=DIRECTION('center_axis',(0.,1.,0.));
#32913=DIRECTION('ref_axis',(0.,0.,1.));
#32914=DIRECTION('center_axis',(0.,1.,0.));
#32915=DIRECTION('ref_axis',(0.,0.,1.));
#32916=DIRECTION('',(0.,1.,0.));
#32917=DIRECTION('center_axis',(0.,1.,0.));
#32918=DIRECTION('ref_axis',(0.,0.,1.));
#32919=DIRECTION('center_axis',(0.,1.,0.));
#32920=DIRECTION('ref_axis',(0.,0.,1.));
#32921=DIRECTION('center_axis',(0.,1.,0.));
#32922=DIRECTION('ref_axis',(0.,0.,1.));
#32923=DIRECTION('',(0.,1.,0.));
#32924=DIRECTION('center_axis',(0.,1.,0.));
#32925=DIRECTION('ref_axis',(0.,0.,1.));
#32926=DIRECTION('center_axis',(0.,1.,0.));
#32927=DIRECTION('ref_axis',(0.,0.,1.));
#32928=DIRECTION('center_axis',(0.,1.,0.));
#32929=DIRECTION('ref_axis',(0.,0.,1.));
#32930=DIRECTION('',(0.,1.,0.));
#32931=DIRECTION('center_axis',(0.,1.,0.));
#32932=DIRECTION('ref_axis',(0.,0.,1.));
#32933=DIRECTION('center_axis',(0.,1.,0.));
#32934=DIRECTION('ref_axis',(0.,0.,1.));
#32935=DIRECTION('center_axis',(0.,1.,0.));
#32936=DIRECTION('ref_axis',(0.,0.,1.));
#32937=DIRECTION('',(0.,1.,0.));
#32938=DIRECTION('center_axis',(0.,1.,0.));
#32939=DIRECTION('ref_axis',(0.,0.,1.));
#32940=DIRECTION('center_axis',(1.,0.,0.));
#32941=DIRECTION('ref_axis',(0.,0.,-1.));
#32942=DIRECTION('center_axis',(1.,0.,0.));
#32943=DIRECTION('ref_axis',(0.,0.,-1.));
#32944=DIRECTION('center_axis',(1.,0.,0.));
#32945=DIRECTION('ref_axis',(0.,0.,-1.));
#32946=DIRECTION('center_axis',(1.,0.,0.));
#32947=DIRECTION('ref_axis',(0.,0.,-1.));
#32948=DIRECTION('center_axis',(1.,0.,0.));
#32949=DIRECTION('ref_axis',(0.,0.,-1.));
#32950=DIRECTION('',(0.,-4.78544407166016E-16,1.));
#32951=DIRECTION('',(0.,-0.707106781186562,0.707106781186533));
#32952=DIRECTION('',(0.,-1.,-3.70074341541719E-16));
#32953=DIRECTION('',(0.,2.19514413070285E-16,-1.));
#32954=DIRECTION('',(0.,1.,1.8503717077086E-16));
#32955=DIRECTION('',(0.,0.707106781186552,0.707106781186543));
#32956=DIRECTION('',(0.,-4.78544407166016E-16,1.));
#32957=DIRECTION('',(0.,1.,7.30409884621814E-16));
#32958=DIRECTION('',(0.,0.707106781186547,0.707106781186547));
#32959=DIRECTION('',(0.,1.77920356510442E-16,1.));
#32960=DIRECTION('',(0.,-0.707106781186543,0.707106781186552));
#32961=DIRECTION('',(0.,-1.,-7.30409884621814E-16));
#32962=DIRECTION('',(0.,-0.707106781186549,0.707106781186546));
#32963=DIRECTION('',(0.,0.,1.));
#32964=DIRECTION('',(0.,0.707106781186546,0.707106781186549));
#32965=DIRECTION('',(0.,1.,0.));
#32966=DIRECTION('',(0.,0.707106781186549,-0.707106781186546));
#32967=DIRECTION('',(0.,0.,-1.));
#32968=DIRECTION('',(0.,-0.707106781186547,-0.707106781186548));
#32969=DIRECTION('',(0.,-1.,0.));
#32970=DIRECTION('center_axis',(0.,-1.,-4.78544407166016E-16));
#32971=DIRECTION('ref_axis',(0.,4.78544407166016E-16,-1.));
#32972=DIRECTION('',(0.,-4.78544407166016E-16,1.));
#32973=DIRECTION('',(-1.,0.,0.));
#32974=DIRECTION('',(-1.,0.,0.));
#32975=DIRECTION('center_axis',(0.,-0.707106781186533,-0.707106781186562));
#32976=DIRECTION('ref_axis',(0.,0.707106781186562,-0.707106781186533));
#32977=DIRECTION('',(0.,-0.707106781186562,0.707106781186533));
#32978=DIRECTION('',(-1.,0.,0.));
#32979=DIRECTION('center_axis',(0.,3.70074341541719E-16,-1.));
#32980=DIRECTION('ref_axis',(0.,1.,3.70074341541719E-16));
#32981=DIRECTION('',(0.,-1.,-3.70074341541719E-16));
#32982=DIRECTION('',(-1.,0.,0.));
#32983=DIRECTION('center_axis',(0.,1.,2.19514413070285E-16));
#32984=DIRECTION('ref_axis',(0.,-2.19514413070285E-16,1.));
#32985=DIRECTION('',(0.,2.19514413070285E-16,-1.));
#32986=DIRECTION('',(-1.,0.,0.));
#32987=DIRECTION('center_axis',(0.,-1.8503717077086E-16,1.));
#32988=DIRECTION('ref_axis',(0.,-1.,-1.8503717077086E-16));
#32989=DIRECTION('',(0.,1.,1.8503717077086E-16));
#32990=DIRECTION('',(-1.,0.,0.));
#32991=DIRECTION('center_axis',(0.,-0.707106781186543,0.707106781186552));
#32992=DIRECTION('ref_axis',(0.,-0.707106781186553,-0.707106781186543));
#32993=DIRECTION('',(0.,0.707106781186552,0.707106781186543));
#32994=DIRECTION('',(-1.,0.,0.));
#32995=DIRECTION('center_axis',(0.,-1.,-4.78544407166016E-16));
#32996=DIRECTION('ref_axis',(0.,4.78544407166016E-16,-1.));
#32997=DIRECTION('',(0.,-4.78544407166016E-16,1.));
#32998=DIRECTION('',(-1.,0.,0.));
#32999=DIRECTION('center_axis',(0.,-7.30409884621814E-16,1.));
#33000=DIRECTION('ref_axis',(0.,-1.,-7.30409884621815E-16));
#33001=DIRECTION('',(0.,1.,7.30409884621814E-16));
#33002=DIRECTION('',(-1.,0.,0.));
#33003=DIRECTION('center_axis',(0.,-0.707106781186548,0.707106781186548));
#33004=DIRECTION('ref_axis',(0.,-0.707106781186548,-0.707106781186548));
#33005=DIRECTION('',(0.,0.707106781186547,0.707106781186547));
#33006=DIRECTION('',(-1.,0.,0.));
#33007=DIRECTION('center_axis',(0.,-1.,1.77920356510442E-16));
#33008=DIRECTION('ref_axis',(0.,-1.77920356510442E-16,-1.));
#33009=DIRECTION('',(0.,1.77920356510442E-16,1.));
#33010=DIRECTION('',(-1.,0.,0.));
#33011=DIRECTION('center_axis',(0.,-0.707106781186552,-0.707106781186543));
#33012=DIRECTION('ref_axis',(0.,0.707106781186543,-0.707106781186553));
#33013=DIRECTION('',(0.,-0.707106781186543,0.707106781186552));
#33014=DIRECTION('',(-1.,0.,0.));
#33015=DIRECTION('center_axis',(0.,7.30409884621814E-16,-1.));
#33016=DIRECTION('ref_axis',(0.,1.,7.30409884621814E-16));
#33017=DIRECTION('',(0.,-1.,-7.30409884621814E-16));
#33018=DIRECTION('center_axis',(1.,0.,0.));
#33019=DIRECTION('ref_axis',(0.,0.,-1.));
#33020=DIRECTION('center_axis',(0.,-1.,0.));
#33021=DIRECTION('ref_axis',(0.,0.,-1.));
#33022=DIRECTION('center_axis',(0.,-1.,0.));
#33023=DIRECTION('ref_axis',(0.,0.,-1.));
#33024=DIRECTION('center_axis',(0.,-1.,0.));
#33025=DIRECTION('ref_axis',(0.,0.,-1.));
#33026=DIRECTION('center_axis',(0.,-1.,0.));
#33027=DIRECTION('ref_axis',(0.,0.,-1.));
#33028=DIRECTION('center_axis',(-1.,0.,0.));
#33029=DIRECTION('ref_axis',(0.,0.,1.));
#33030=DIRECTION('',(0.,0.,1.));
#33031=DIRECTION('',(0.,-0.707106781186549,0.707106781186546));
#33032=DIRECTION('',(0.,-1.,0.));
#33033=DIRECTION('',(0.,-0.707106781186547,-0.707106781186548));
#33034=DIRECTION('',(0.,0.,-1.));
#33035=DIRECTION('',(0.,0.707106781186549,-0.707106781186546));
#33036=DIRECTION('',(0.,1.,0.));
#33037=DIRECTION('',(0.,0.707106781186546,0.707106781186549));
#33038=DIRECTION('center_axis',(0.,-1.,0.));
#33039=DIRECTION('ref_axis',(0.,0.,-1.));
#33040=DIRECTION('',(-1.,0.,0.));
#33041=DIRECTION('',(-1.,0.,0.));
#33042=DIRECTION('center_axis',(0.,-0.707106781186546,-0.707106781186549));
#33043=DIRECTION('ref_axis',(0.,0.707106781186549,-0.707106781186546));
#33044=DIRECTION('',(-1.,0.,0.));
#33045=DIRECTION('center_axis',(0.,0.,-1.));
#33046=DIRECTION('ref_axis',(-1.,0.,0.));
#33047=DIRECTION('',(-1.,0.,0.));
#33048=DIRECTION('center_axis',(0.,0.707106781186548,-0.707106781186547));
#33049=DIRECTION('ref_axis',(0.,0.707106781186547,0.707106781186548));
#33050=DIRECTION('',(-1.,0.,0.));
#33051=DIRECTION('center_axis',(0.,1.,0.));
#33052=DIRECTION('ref_axis',(0.,0.,1.));
#33053=DIRECTION('',(-1.,0.,0.));
#33054=DIRECTION('center_axis',(0.,0.707106781186546,0.707106781186549));
#33055=DIRECTION('ref_axis',(0.,-0.707106781186549,0.707106781186546));
#33056=DIRECTION('',(-1.,0.,0.));
#33057=DIRECTION('center_axis',(0.,0.,1.));
#33058=DIRECTION('ref_axis',(1.,0.,0.));
#33059=DIRECTION('',(-1.,0.,0.));
#33060=DIRECTION('center_axis',(0.,-0.707106781186549,0.707106781186546));
#33061=DIRECTION('ref_axis',(0.,-0.707106781186546,-0.707106781186549));
#33062=DIRECTION('center_axis',(1.,0.,0.));
#33063=DIRECTION('ref_axis',(0.,0.,-1.));
#33064=DIRECTION('',(0.,0.500000000000004,-0.866025403784436));
#33065=DIRECTION('',(0.,-0.500000000000004,-0.866025403784436));
#33066=DIRECTION('',(0.,-1.,0.));
#33067=DIRECTION('',(0.,-0.500000000000008,0.866025403784434));
#33068=DIRECTION('',(0.,0.500000000000004,0.866025403784437));
#33069=DIRECTION('',(0.,1.,0.));
#33070=DIRECTION('center_axis',(1.,0.,0.));
#33071=DIRECTION('ref_axis',(0.,0.,-1.));
#33072=DIRECTION('',(0.,0.499999999999999,-0.866025403784439));
#33073=DIRECTION('',(0.,-0.5,-0.866025403784438));
#33074=DIRECTION('',(0.,-1.,0.));
#33075=DIRECTION('',(0.,-0.500000000000001,0.866025403784438));
#33076=DIRECTION('',(0.,0.500000000000001,0.866025403784438));
#33077=DIRECTION('',(0.,1.,0.));
#33078=DIRECTION('center_axis',(1.,0.,0.));
#33079=DIRECTION('ref_axis',(0.,0.,-1.));
#33080=DIRECTION('',(0.,0.5,-0.866025403784439));
#33081=DIRECTION('',(0.,-0.5,-0.866025403784439));
#33082=DIRECTION('',(0.,-1.,0.));
#33083=DIRECTION('',(0.,-0.5,0.866025403784438));
#33084=DIRECTION('',(0.,0.5,0.866025403784438));
#33085=DIRECTION('',(0.,1.,1.00154306582478E-15));
#33086=DIRECTION('center_axis',(1.,0.,0.));
#33087=DIRECTION('ref_axis',(0.,0.,-1.));
#33088=DIRECTION('',(0.,0.500000000000001,-0.866025403784438));
#33089=DIRECTION('',(0.,-0.5,-0.866025403784439));
#33090=DIRECTION('',(0.,-1.,0.));
#33091=DIRECTION('',(0.,-0.5,0.866025403784439));
#33092=DIRECTION('',(0.,0.499999999999999,0.866025403784439));
#33093=DIRECTION('',(0.,1.,-1.00154306582477E-15));
#33094=DIRECTION('center_axis',(0.,-0.866025403784436,-0.500000000000004));
#33095=DIRECTION('ref_axis',(0.,0.500000000000004,-0.866025403784436));
#33096=DIRECTION('',(1.,0.,0.));
#33097=DIRECTION('',(0.,0.500000000000004,-0.866025403784436));
#33098=DIRECTION('',(1.,0.,0.));
#33099=DIRECTION('center_axis',(0.,-0.866025403784436,0.500000000000004));
#33100=DIRECTION('ref_axis',(0.,-0.500000000000004,-0.866025403784436));
#33101=DIRECTION('',(0.,-0.500000000000004,-0.866025403784436));
#33102=DIRECTION('',(1.,0.,0.));
#33103=DIRECTION('center_axis',(0.,0.,1.));
#33104=DIRECTION('ref_axis',(1.,0.,0.));
#33105=DIRECTION('',(0.,-1.,0.));
#33106=DIRECTION('',(1.,0.,0.));
#33107=DIRECTION('center_axis',(0.,0.866025403784434,0.500000000000008));
#33108=DIRECTION('ref_axis',(0.,-0.500000000000007,0.866025403784434));
#33109=DIRECTION('',(0.,-0.500000000000008,0.866025403784434));
#33110=DIRECTION('',(1.,0.,0.));
#33111=DIRECTION('center_axis',(0.,0.866025403784437,-0.500000000000004));
#33112=DIRECTION('ref_axis',(0.,0.500000000000004,0.866025403784437));
#33113=DIRECTION('',(0.,0.500000000000004,0.866025403784437));
#33114=DIRECTION('',(1.,0.,0.));
#33115=DIRECTION('center_axis',(0.,0.,-1.));
#33116=DIRECTION('ref_axis',(-1.,0.,0.));
#33117=DIRECTION('',(0.,1.,0.));
#33118=DIRECTION('center_axis',(1.,0.,0.));
#33119=DIRECTION('ref_axis',(0.,0.,-1.));
#33120=DIRECTION('center_axis',(0.,-0.866025403784439,-0.499999999999999));
#33121=DIRECTION('ref_axis',(0.,0.499999999999999,-0.866025403784439));
#33122=DIRECTION('',(1.,0.,0.));
#33123=DIRECTION('',(0.,0.499999999999999,-0.866025403784439));
#33124=DIRECTION('',(1.,0.,0.));
#33125=DIRECTION('center_axis',(0.,-0.866025403784438,0.5));
#33126=DIRECTION('ref_axis',(0.,-0.5,-0.866025403784438));
#33127=DIRECTION('',(0.,-0.5,-0.866025403784438));
#33128=DIRECTION('',(1.,0.,0.));
#33129=DIRECTION('center_axis',(0.,0.,1.));
#33130=DIRECTION('ref_axis',(1.,0.,0.));
#33131=DIRECTION('',(0.,-1.,0.));
#33132=DIRECTION('',(1.,0.,0.));
#33133=DIRECTION('center_axis',(0.,0.866025403784438,0.500000000000001));
#33134=DIRECTION('ref_axis',(0.,-0.500000000000001,0.866025403784438));
#33135=DIRECTION('',(0.,-0.500000000000001,0.866025403784438));
#33136=DIRECTION('',(1.,0.,0.));
#33137=DIRECTION('center_axis',(0.,0.866025403784438,-0.500000000000001));
#33138=DIRECTION('ref_axis',(0.,0.500000000000001,0.866025403784438));
#33139=DIRECTION('',(0.,0.500000000000001,0.866025403784438));
#33140=DIRECTION('',(1.,0.,0.));
#33141=DIRECTION('center_axis',(0.,0.,-1.));
#33142=DIRECTION('ref_axis',(-1.,0.,0.));
#33143=DIRECTION('',(0.,1.,0.));
#33144=DIRECTION('center_axis',(1.,0.,0.));
#33145=DIRECTION('ref_axis',(0.,0.,-1.));
#33146=DIRECTION('center_axis',(0.,-0.866025403784438,-0.500000000000001));
#33147=DIRECTION('ref_axis',(0.,0.500000000000001,-0.866025403784438));
#33148=DIRECTION('',(1.,0.,0.));
#33149=DIRECTION('',(0.,0.500000000000001,-0.866025403784438));
#33150=DIRECTION('',(1.,0.,0.));
#33151=DIRECTION('center_axis',(0.,-0.866025403784439,0.5));
#33152=DIRECTION('ref_axis',(0.,-0.5,-0.866025403784439));
#33153=DIRECTION('',(0.,-0.5,-0.866025403784439));
#33154=DIRECTION('',(1.,0.,0.));
#33155=DIRECTION('center_axis',(0.,0.,1.));
#33156=DIRECTION('ref_axis',(1.,0.,0.));
#33157=DIRECTION('',(0.,-1.,0.));
#33158=DIRECTION('',(1.,0.,0.));
#33159=DIRECTION('center_axis',(0.,0.866025403784439,0.5));
#33160=DIRECTION('ref_axis',(0.,-0.5,0.866025403784439));
#33161=DIRECTION('',(0.,-0.5,0.866025403784439));
#33162=DIRECTION('',(1.,0.,0.));
#33163=DIRECTION('center_axis',(0.,0.866025403784439,-0.499999999999999));
#33164=DIRECTION('ref_axis',(0.,0.499999999999999,0.866025403784439));
#33165=DIRECTION('',(0.,0.499999999999999,0.866025403784439));
#33166=DIRECTION('',(1.,0.,0.));
#33167=DIRECTION('center_axis',(0.,-1.00154306582477E-15,-1.));
#33168=DIRECTION('ref_axis',(0.,1.,-1.00154306582477E-15));
#33169=DIRECTION('',(0.,1.,-1.00154306582477E-15));
#33170=DIRECTION('center_axis',(1.,0.,0.));
#33171=DIRECTION('ref_axis',(0.,0.,-1.));
#33172=DIRECTION('center_axis',(0.,-0.866025403784439,-0.5));
#33173=DIRECTION('ref_axis',(0.,0.5,-0.866025403784439));
#33174=DIRECTION('',(1.,0.,0.));
#33175=DIRECTION('',(0.,0.5,-0.866025403784439));
#33176=DIRECTION('',(1.,0.,0.));
#33177=DIRECTION('center_axis',(0.,-0.866025403784439,0.5));
#33178=DIRECTION('ref_axis',(0.,-0.5,-0.866025403784439));
#33179=DIRECTION('',(0.,-0.5,-0.866025403784439));
#33180=DIRECTION('',(1.,0.,0.));
#33181=DIRECTION('center_axis',(0.,0.,1.));
#33182=DIRECTION('ref_axis',(1.,0.,0.));
#33183=DIRECTION('',(0.,-1.,0.));
#33184=DIRECTION('',(1.,0.,0.));
#33185=DIRECTION('center_axis',(0.,0.866025403784438,0.5));
#33186=DIRECTION('ref_axis',(0.,-0.5,0.866025403784438));
#33187=DIRECTION('',(0.,-0.5,0.866025403784438));
#33188=DIRECTION('',(1.,0.,0.));
#33189=DIRECTION('center_axis',(0.,0.866025403784438,-0.5));
#33190=DIRECTION('ref_axis',(0.,0.5,0.866025403784438));
#33191=DIRECTION('',(0.,0.5,0.866025403784438));
#33192=DIRECTION('',(1.,0.,0.));
#33193=DIRECTION('center_axis',(0.,1.00154306582478E-15,-1.));
#33194=DIRECTION('ref_axis',(0.,1.,1.00154306582478E-15));
#33195=DIRECTION('',(0.,1.,1.00154306582478E-15));
#33196=DIRECTION('center_axis',(1.,0.,0.));
#33197=DIRECTION('ref_axis',(0.,0.,-1.));
#33198=DIRECTION('center_axis',(1.,0.,0.));
#33199=DIRECTION('ref_axis',(0.,0.,-1.));
#33200=DIRECTION('center_axis',(1.,0.,0.));
#33201=DIRECTION('ref_axis',(0.,0.,-1.));
#33202=DIRECTION('center_axis',(-1.,0.,0.));
#33203=DIRECTION('ref_axis',(0.,0.,1.));
#33204=DIRECTION('center_axis',(-1.,0.,0.));
#33205=DIRECTION('ref_axis',(0.,0.,1.));
#33206=DIRECTION('axis',(0.,0.,1.));
#33207=DIRECTION('refdir',(1.,0.,0.));
#33208=DIRECTION('center_axis',(-2.66880534765663E-16,1.,0.));
#33209=DIRECTION('ref_axis',(-1.,-2.66880534765663E-16,0.));
#33210=DIRECTION('',(0.85716730070211,0.515038074910058,-1.04972719113862E-16));
#33211=DIRECTION('center_axis',(2.66880534765663E-16,-1.,0.));
#33212=DIRECTION('ref_axis',(1.,2.66880534765663E-16,0.));
#33213=DIRECTION('center_axis',(2.66880534765663E-16,-1.,0.));
#33214=DIRECTION('ref_axis',(1.,2.66880534765663E-16,0.));
#33215=DIRECTION('center_axis',(2.66880534765663E-16,-1.,0.));
#33216=DIRECTION('ref_axis',(1.,2.66880534765663E-16,0.));
#33217=DIRECTION('center_axis',(2.66880534765663E-16,-1.,0.));
#33218=DIRECTION('ref_axis',(1.,2.66880534765663E-16,0.));
#33219=DIRECTION('center_axis',(2.66880534765663E-16,-1.,0.));
#33220=DIRECTION('ref_axis',(1.,2.66880534765663E-16,0.));
#33221=DIRECTION('center_axis',(2.66880534765663E-16,-1.,0.));
#33222=DIRECTION('ref_axis',(1.,2.66880534765663E-16,0.));
#33223=DIRECTION('center_axis',(2.66880534765663E-16,-1.,0.));
#33224=DIRECTION('ref_axis',(1.,2.66880534765663E-16,0.));
#33225=DIRECTION('',(2.66880534765663E-16,-1.,0.));
#33226=DIRECTION('center_axis',(2.66880534765663E-16,-1.,0.));
#33227=DIRECTION('ref_axis',(1.,2.66880534765663E-16,0.));
#33228=DIRECTION('center_axis',(2.66880534765663E-16,-1.,0.));
#33229=DIRECTION('ref_axis',(1.,2.66880534765663E-16,0.));
#33230=DIRECTION('',(0.707106781186543,0.707106781186552,8.65956056235488E-17));
#33231=DIRECTION('center_axis',(-2.66880534765663E-16,1.,0.));
#33232=DIRECTION('ref_axis',(-1.,-2.66880534765663E-16,0.));
#33233=DIRECTION('center_axis',(2.66880534765663E-16,-1.,0.));
#33234=DIRECTION('ref_axis',(1.,2.66880534765663E-16,0.));
#33235=DIRECTION('',(-0.707106781186542,-0.707106781186553,8.65956056235487E-17));
#33236=DIRECTION('center_axis',(2.66880534765663E-16,-1.,0.));
#33237=DIRECTION('ref_axis',(1.,2.66880534765663E-16,0.));
#33238=DIRECTION('center_axis',(2.66880534765663E-16,-1.,0.));
#33239=DIRECTION('ref_axis',(1.,2.66880534765663E-16,0.));
#33240=DIRECTION('center_axis',(2.66880534765663E-16,-1.,0.));
#33241=DIRECTION('ref_axis',(1.,2.66880534765663E-16,0.));
#33242=DIRECTION('',(2.66880534765663E-16,-1.,0.));
#33243=DIRECTION('center_axis',(1.,0.,0.));
#33244=DIRECTION('ref_axis',(0.,0.,-1.));
#33245=DIRECTION('center_axis',(-1.,0.,0.));
#33246=DIRECTION('ref_axis',(0.,0.,1.));
#33247=DIRECTION('',(0.707106781186546,-8.65956056235495E-17,0.707106781186549));
#33248=DIRECTION('center_axis',(-1.,0.,0.));
#33249=DIRECTION('ref_axis',(0.,0.,1.));
#33250=DIRECTION('center_axis',(-1.,0.,0.));
#33251=DIRECTION('ref_axis',(0.,0.,1.));
#33252=DIRECTION('center_axis',(-1.,0.,0.));
#33253=DIRECTION('ref_axis',(0.,0.,1.));
#33254=DIRECTION('center_axis',(-1.,0.,0.));
#33255=DIRECTION('ref_axis',(0.,0.,1.));
#33256=DIRECTION('',(-0.707106781186548,-8.65956056235493E-17,-0.707106781186547));
#33257=DIRECTION('center_axis',(-1.,0.,0.));
#33258=DIRECTION('ref_axis',(0.,0.,1.));
#33259=DIRECTION('center_axis',(-1.,0.,0.));
#33260=DIRECTION('ref_axis',(0.,0.,1.));
#33261=DIRECTION('center_axis',(-1.,0.,0.));
#33262=DIRECTION('ref_axis',(0.,0.,1.));
#33263=DIRECTION('',(-1.,0.,0.));
#33264=DIRECTION('center_axis',(-1.,0.,0.));
#33265=DIRECTION('ref_axis',(0.,0.,1.));
#33266=DIRECTION('',(1.,0.,0.));
#33267=DIRECTION('center_axis',(-1.,0.,0.));
#33268=DIRECTION('ref_axis',(0.,0.,1.));
#33269=DIRECTION('center_axis',(-1.,0.,0.));
#33270=DIRECTION('ref_axis',(0.,0.,1.));
#33271=DIRECTION('',(1.,0.,0.));
#33272=DIRECTION('center_axis',(-1.,0.,0.));
#33273=DIRECTION('ref_axis',(0.,0.,1.));
#33274=DIRECTION('center_axis',(-1.,0.,0.));
#33275=DIRECTION('ref_axis',(0.,0.,1.));
#33276=DIRECTION('',(-1.,0.,0.));
#33277=DIRECTION('center_axis',(-1.,0.,0.));
#33278=DIRECTION('ref_axis',(0.,0.,1.));
#33279=DIRECTION('center_axis',(1.,0.,-1.50231459873716E-15));
#33280=DIRECTION('ref_axis',(-1.50231459873716E-15,0.,-1.));
#33281=DIRECTION('center_axis',(0.500000000000006,-1.56587054853355E-13,
0.866025403784435));
#33282=DIRECTION('ref_axis',(-0.0401154877944071,0.998926588987072,0.0231606876769527));
#33283=DIRECTION('center_axis',(-0.500000000000001,-6.71087377942918E-14,
0.866025403784438));
#33284=DIRECTION('ref_axis',(0.0200049178614522,0.999733166574198,0.0115498447125027));
#33285=DIRECTION('center_axis',(-1.,0.,7.51157299368581E-16));
#33286=DIRECTION('ref_axis',(7.51157299368581E-16,0.,1.));
#33287=DIRECTION('center_axis',(-0.500000000000002,-5.59239481618774E-14,
-0.866025403784438));
#33288=DIRECTION('ref_axis',(0.0401154877945203,0.99892658898707,-0.0231606876768818));
#33289=DIRECTION('center_axis',(0.499999999999995,1.4540226522103E-13,-0.866025403784442));
#33290=DIRECTION('ref_axis',(-0.0200049178616206,0.999733166574197,-0.0115498447123624));
#33291=DIRECTION('center_axis',(-1.,0.,0.));
#33292=DIRECTION('ref_axis',(0.,0.,1.));
#33293=DIRECTION('center_axis',(-1.,0.,0.));
#33294=DIRECTION('ref_axis',(0.,0.,1.));
#33295=DIRECTION('',(-1.,0.,0.));
#33296=DIRECTION('center_axis',(-1.,0.,0.));
#33297=DIRECTION('ref_axis',(0.,0.,1.));
#33298=DIRECTION('',(1.,0.,0.));
#33299=DIRECTION('center_axis',(-1.,0.,0.));
#33300=DIRECTION('ref_axis',(0.,0.,1.));
#33301=DIRECTION('center_axis',(-1.,0.,0.));
#33302=DIRECTION('ref_axis',(0.,0.,1.));
#33303=DIRECTION('',(-1.,0.,0.));
#33304=DIRECTION('center_axis',(-1.,0.,0.));
#33305=DIRECTION('ref_axis',(0.,0.,1.));
#33306=DIRECTION('',(1.,0.,0.));
#33307=DIRECTION('center_axis',(-1.,0.,0.));
#33308=DIRECTION('ref_axis',(0.,-3.21624529935327E-16,-1.));
#33309=DIRECTION('center_axis',(-1.,0.,0.));
#33310=DIRECTION('ref_axis',(0.,0.,1.));
#33311=DIRECTION('',(-1.,0.,0.));
#33312=DIRECTION('center_axis',(-1.,0.,0.));
#33313=DIRECTION('ref_axis',(0.,0.,1.));
#33314=DIRECTION('',(1.,0.,0.));
#33315=DIRECTION('center_axis',(1.,0.,0.));
#33316=DIRECTION('ref_axis',(0.,0.,-1.));
#33317=DIRECTION('center_axis',(1.,0.,0.));
#33318=DIRECTION('ref_axis',(0.,0.,-1.));
#33319=DIRECTION('',(0.,0.707106781186548,0.707106781186547));
#33320=DIRECTION('',(0.,0.707106781186547,-0.707106781186547));
#33321=DIRECTION('',(0.,-0.707106781186547,-0.707106781186548));
#33322=DIRECTION('',(0.,-0.707106781186548,0.707106781186547));
#33323=DIRECTION('center_axis',(-1.,0.,0.));
#33324=DIRECTION('ref_axis',(0.,0.,1.));
#33325=DIRECTION('',(0.,-0.707106781186548,-0.707106781186547));
#33326=DIRECTION('',(0.,0.707106781186548,-0.707106781186547));
#33327=DIRECTION('',(0.,0.707106781186547,0.707106781186548));
#33328=DIRECTION('',(0.,-0.707106781186547,0.707106781186547));
#33329=DIRECTION('center_axis',(0.,-0.707106781186548,-0.707106781186548));
#33330=DIRECTION('ref_axis',(0.,0.707106781186548,-0.707106781186548));
#33331=DIRECTION('center_axis',(0.,-0.707106781186548,0.707106781186547));
#33332=DIRECTION('ref_axis',(0.,-0.707106781186547,-0.707106781186548));
#33333=DIRECTION('center_axis',(0.,0.707106781186547,0.707106781186548));
#33334=DIRECTION('ref_axis',(0.,-0.707106781186548,0.707106781186547));
#33335=DIRECTION('center_axis',(0.,0.707106781186547,-0.707106781186548));
#33336=DIRECTION('ref_axis',(0.,0.707106781186548,0.707106781186547));
#33337=DIRECTION('center_axis',(2.66880534765663E-16,-1.,0.));
#33338=DIRECTION('ref_axis',(1.,2.66880534765663E-16,0.));
#33339=DIRECTION('center_axis',(0.500000000000001,0.,0.866025403784438));
#33340=DIRECTION('ref_axis',(0.866025403784438,0.,-0.500000000000001));
#33341=DIRECTION('',(0.,1.,0.));
#33342=DIRECTION('',(0.866025403784438,0.,-0.500000000000001));
#33343=DIRECTION('',(0.866025403784438,0.,-0.500000000000001));
#33344=DIRECTION('',(0.,1.,0.));
#33345=DIRECTION('center_axis',(-0.499999999999999,0.,0.866025403784439));
#33346=DIRECTION('ref_axis',(0.866025403784439,0.,0.499999999999999));
#33347=DIRECTION('',(0.866025403784439,0.,0.499999999999999));
#33348=DIRECTION('',(0.866025403784439,0.,0.499999999999999));
#33349=DIRECTION('',(0.,1.,0.));
#33350=DIRECTION('center_axis',(-1.,0.,7.51157299368581E-16));
#33351=DIRECTION('ref_axis',(7.51157299368581E-16,0.,1.));
#33352=DIRECTION('',(7.51157299368581E-16,0.,1.));
#33353=DIRECTION('',(7.51157299368581E-16,0.,1.));
#33354=DIRECTION('',(0.,1.,0.));
#33355=DIRECTION('center_axis',(-0.500000000000001,0.,-0.866025403784438));
#33356=DIRECTION('ref_axis',(-0.866025403784438,0.,0.500000000000001));
#33357=DIRECTION('',(-0.866025403784438,0.,0.500000000000001));
#33358=DIRECTION('',(-0.866025403784438,0.,0.500000000000001));
#33359=DIRECTION('',(0.,1.,0.));
#33360=DIRECTION('center_axis',(0.499999999999999,0.,-0.866025403784439));
#33361=DIRECTION('ref_axis',(-0.866025403784439,0.,-0.499999999999999));
#33362=DIRECTION('',(-0.866025403784439,0.,-0.499999999999999));
#33363=DIRECTION('',(-0.866025403784439,0.,-0.499999999999999));
#33364=DIRECTION('',(0.,1.,0.));
#33365=DIRECTION('center_axis',(1.,0.,-1.50231459873716E-15));
#33366=DIRECTION('ref_axis',(-1.50231459873716E-15,0.,-1.));
#33367=DIRECTION('',(-1.50231459873716E-15,0.,-1.));
#33368=DIRECTION('',(-1.50231459873716E-15,0.,-1.));
#33369=DIRECTION('center_axis',(0.,1.,0.));
#33370=DIRECTION('ref_axis',(0.,0.,1.));
#33371=DIRECTION('center_axis',(0.,1.,0.));
#33372=DIRECTION('ref_axis',(0.,0.,1.));
#33373=DIRECTION('center_axis',(0.,1.,0.));
#33374=DIRECTION('ref_axis',(0.,0.,1.));
#33375=DIRECTION('center_axis',(0.,1.,0.));
#33376=DIRECTION('ref_axis',(0.,0.,1.));
#33377=DIRECTION('center_axis',(0.,1.,0.));
#33378=DIRECTION('ref_axis',(0.,0.,1.));
#33379=DIRECTION('center_axis',(0.,1.,0.));
#33380=DIRECTION('ref_axis',(0.,0.,1.));
#33381=DIRECTION('axis',(0.,0.,1.));
#33382=DIRECTION('refdir',(1.,0.,0.));
#33383=DIRECTION('center_axis',(-1.,0.,0.));
#33384=DIRECTION('ref_axis',(0.,0.,1.));
#33385=DIRECTION('center_axis',(-1.,0.,0.));
#33386=DIRECTION('ref_axis',(0.,0.,1.));
#33387=DIRECTION('',(1.,0.,0.));
#33388=DIRECTION('center_axis',(-1.,0.,0.));
#33389=DIRECTION('ref_axis',(0.,0.,1.));
#33390=DIRECTION('center_axis',(-1.,0.,0.));
#33391=DIRECTION('ref_axis',(0.,0.,1.));
#33392=DIRECTION('center_axis',(-1.,0.,0.));
#33393=DIRECTION('ref_axis',(0.,0.,1.));
#33394=DIRECTION('',(-1.,0.,0.));
#33395=DIRECTION('center_axis',(-1.,0.,0.));
#33396=DIRECTION('ref_axis',(0.,0.,1.));
#33397=DIRECTION('center_axis',(1.,0.,0.));
#33398=DIRECTION('ref_axis',(0.,0.,-1.));
#33399=DIRECTION('center_axis',(-1.,0.,0.));
#33400=DIRECTION('ref_axis',(0.,0.,1.));
#33401=DIRECTION('',(-2.69880267346701E-79,7.549645381998E-32,1.));
#33402=DIRECTION('',(1.,3.69778549322349E-32,-2.79169691725339E-63));
#33403=DIRECTION('',(-1.11342479587336E-17,-1.38777878078145E-16,-1.));
#33404=DIRECTION('',(-1.,-2.66648173365583E-16,1.11342479587337E-17));
#33405=DIRECTION('',(-2.69880267346701E-79,7.549645381998E-32,1.));
#33406=DIRECTION('',(1.,3.69778549322349E-32,-2.79169691725339E-63));
#33407=DIRECTION('',(-2.69880267346701E-79,7.549645381998E-32,1.));
#33408=DIRECTION('',(1.,3.69778549322349E-32,-2.79169691725339E-63));
#33409=DIRECTION('axis',(0.,0.,1.));
#33410=DIRECTION('refdir',(1.,0.,0.));
#33411=DIRECTION('center_axis',(0.,0.,1.));
#33412=DIRECTION('ref_axis',(1.,0.,0.));
#33413=DIRECTION('center_axis',(0.,0.,1.));
#33414=DIRECTION('ref_axis',(1.,0.,0.));
#33415=DIRECTION('',(0.,0.,1.));
#33416=DIRECTION('center_axis',(0.,0.,1.));
#33417=DIRECTION('ref_axis',(1.,0.,0.));
#33418=DIRECTION('center_axis',(0.,0.,1.));
#33419=DIRECTION('ref_axis',(1.,0.,0.));
#33420=DIRECTION('center_axis',(0.,0.,1.));
#33421=DIRECTION('ref_axis',(1.,0.,0.));
#33422=DIRECTION('',(0.,0.,1.));
#33423=DIRECTION('center_axis',(0.,0.,1.));
#33424=DIRECTION('ref_axis',(1.,0.,0.));
#33425=DIRECTION('center_axis',(0.,0.,1.));
#33426=DIRECTION('ref_axis',(1.,0.,0.));
#33427=DIRECTION('center_axis',(0.,0.,1.));
#33428=DIRECTION('ref_axis',(1.,0.,0.));
#33429=DIRECTION('',(0.,0.,1.));
#33430=DIRECTION('center_axis',(0.,0.,1.));
#33431=DIRECTION('ref_axis',(1.,0.,0.));
#33432=DIRECTION('center_axis',(0.,0.,1.));
#33433=DIRECTION('ref_axis',(1.,0.,0.));
#33434=DIRECTION('center_axis',(0.,0.,1.));
#33435=DIRECTION('ref_axis',(1.,0.,0.));
#33436=DIRECTION('',(0.,0.,1.));
#33437=DIRECTION('center_axis',(0.,0.,1.));
#33438=DIRECTION('ref_axis',(1.,0.,0.));
#33439=DIRECTION('center_axis',(0.,0.,1.));
#33440=DIRECTION('ref_axis',(1.,0.,0.));
#33441=DIRECTION('center_axis',(0.,0.,1.));
#33442=DIRECTION('ref_axis',(1.,0.,0.));
#33443=DIRECTION('',(0.,0.,1.));
#33444=DIRECTION('center_axis',(0.,0.,1.));
#33445=DIRECTION('ref_axis',(1.,0.,0.));
#33446=DIRECTION('center_axis',(0.,0.,1.));
#33447=DIRECTION('ref_axis',(1.,0.,0.));
#33448=DIRECTION('center_axis',(0.,0.,1.));
#33449=DIRECTION('ref_axis',(1.,0.,0.));
#33450=DIRECTION('',(0.,0.,1.));
#33451=DIRECTION('center_axis',(0.,0.,1.));
#33452=DIRECTION('ref_axis',(1.,0.,0.));
#33453=DIRECTION('center_axis',(0.,0.,1.));
#33454=DIRECTION('ref_axis',(1.,0.,0.));
#33455=DIRECTION('',(-3.46944695195362E-16,1.,0.));
#33456=DIRECTION('',(-1.,6.93889390390723E-16,0.));
#33457=DIRECTION('',(-2.31296463463574E-16,1.,0.));
#33458=DIRECTION('',(-1.,0.,0.));
#33459=DIRECTION('center_axis',(-1.,-2.31296463463574E-16,0.));
#33460=DIRECTION('ref_axis',(2.31296463463574E-16,-1.,0.));
#33461=DIRECTION('',(0.,0.,1.));
#33462=DIRECTION('',(-3.46944695195361E-16,1.,0.));
#33463=DIRECTION('',(0.,0.,-1.));
#33464=DIRECTION('',(-2.31296463463574E-16,1.,0.));
#33465=DIRECTION('',(0.,0.,-1.));
#33466=DIRECTION('center_axis',(0.,-1.,0.));
#33467=DIRECTION('ref_axis',(0.,0.,-1.));
#33468=DIRECTION('',(-1.,0.,0.));
#33469=DIRECTION('',(0.,0.,1.));
#33470=DIRECTION('',(-1.,0.,0.));
#33471=DIRECTION('',(0.,0.,-1.));
#33472=DIRECTION('center_axis',(1.,0.,0.));
#33473=DIRECTION('ref_axis',(0.,0.,-1.));
#33474=DIRECTION('',(0.,-1.,0.));
#33475=DIRECTION('',(0.,0.,1.));
#33476=DIRECTION('',(4.95635278850516E-16,-1.,0.));
#33477=DIRECTION('',(0.,-1.,0.));
#33478=DIRECTION('',(0.,0.,-1.));
#33479=DIRECTION('center_axis',(0.,1.,0.));
#33480=DIRECTION('ref_axis',(0.,0.,1.));
#33481=DIRECTION('',(1.,0.,0.));
#33482=DIRECTION('',(0.,0.,1.));
#33483=DIRECTION('',(1.,0.,0.));
#33484=DIRECTION('',(1.,0.,0.));
#33485=DIRECTION('center_axis',(0.,0.,1.));
#33486=DIRECTION('ref_axis',(1.,0.,0.));
#33487=DIRECTION('',(1.73472347597681E-15,-1.,0.));
#33488=DIRECTION('',(1.,6.48494757374508E-17,0.));
#33489=DIRECTION('center_axis',(0.,0.,1.));
#33490=DIRECTION('ref_axis',(1.,0.,0.));
#33491=DIRECTION('center_axis',(1.,3.46944695195362E-16,0.));
#33492=DIRECTION('ref_axis',(-3.46944695195362E-16,1.,0.));
#33493=DIRECTION('',(-3.46944695195362E-16,1.,0.));
#33494=DIRECTION('',(0.,0.,1.));
#33495=DIRECTION('center_axis',(6.93889390390723E-16,1.,0.));
#33496=DIRECTION('ref_axis',(-1.,6.93889390390723E-16,0.));
#33497=DIRECTION('',(-1.,6.93889390390723E-16,0.));
#33498=DIRECTION('center_axis',(-1.,-1.73472347597681E-15,0.));
#33499=DIRECTION('ref_axis',(1.73472347597681E-15,-1.,0.));
#33500=DIRECTION('',(1.73472347597681E-15,-1.,0.));
#33501=DIRECTION('',(0.,0.,1.));
#33502=DIRECTION('center_axis',(6.48494757374508E-17,-1.,0.));
#33503=DIRECTION('ref_axis',(1.,6.48494757374508E-17,0.));
#33504=DIRECTION('',(1.,6.48494757374508E-17,0.));
#33505=DIRECTION('center_axis',(0.,0.,1.));
#33506=DIRECTION('ref_axis',(1.,0.,0.));
#33507=DIRECTION('axis',(0.,0.,1.));
#33508=DIRECTION('refdir',(1.,0.,0.));
#33509=DIRECTION('axis',(0.,0.,1.));
#33510=DIRECTION('refdir',(1.,0.,0.));
#33511=DIRECTION('axis',(0.,0.,1.));
#33512=DIRECTION('refdir',(1.,0.,0.));
#33513=DIRECTION('center_axis',(-1.,0.,0.));
#33514=DIRECTION('ref_axis',(0.,0.,1.));
#33515=DIRECTION('center_axis',(-1.,0.,0.));
#33516=DIRECTION('ref_axis',(0.,0.923879532525282,-0.382683432331302));
#33517=DIRECTION('center_axis',(1.,0.,0.));
#33518=DIRECTION('ref_axis',(0.,-0.923879532525282,0.382683432331302));
#33519=DIRECTION('',(-1.,0.,0.));
#33520=DIRECTION('center_axis',(-1.,0.,0.));
#33521=DIRECTION('ref_axis',(0.,-0.923879532525282,0.382683432331302));
#33522=DIRECTION('center_axis',(-1.,0.,0.));
#33523=DIRECTION('ref_axis',(0.,0.,1.));
#33524=DIRECTION('center_axis',(-1.,0.,0.));
#33525=DIRECTION('ref_axis',(0.,0.382683432398878,-0.923879532497291));
#33526=DIRECTION('center_axis',(1.,0.,0.));
#33527=DIRECTION('ref_axis',(0.,-0.382683432398878,0.923879532497291));
#33528=DIRECTION('center_axis',(-1.,0.,0.));
#33529=DIRECTION('ref_axis',(0.,-0.382683432398878,0.923879532497291));
#33530=DIRECTION('',(-1.,0.,0.));
#33531=DIRECTION('center_axis',(-0.914213393717196,0.0442003138869465,0.402815346033865));
#33532=DIRECTION('ref_axis',(-0.263860958992393,0.689505825675568,-0.674506568299426));
#33533=DIRECTION('center_axis',(0.,-0.988888328046728,0.148660265884823));
#33534=DIRECTION('ref_axis',(1.,0.,0.));
#33535=DIRECTION('center_axis',(0.,-0.362081724527015,0.932146353725391));
#33536=DIRECTION('ref_axis',(1.,0.,0.));
#33537=DIRECTION('center_axis',(0.99999999999897,-1.32776773271782E-6,-5.45065136955466E-7));
#33538=DIRECTION('ref_axis',(1.43483054990958E-6,0.915158915916019,0.403093238119119));
#33539=DIRECTION('center_axis',(4.59701721133854E-17,0.403096564446046,
-0.915157450787456));
#33540=DIRECTION('ref_axis',(-0.0114743075678194,0.915097204111032,0.403070027779307));
#33541=DIRECTION('center_axis',(1.,-5.02651426597364E-10,-2.14769807745443E-10));
#33542=DIRECTION('ref_axis',(5.46578186166822E-10,0.915157853095838,0.403095651076784));
#33543=DIRECTION('center_axis',(3.99680239858264E-14,0.988888328046729,
-0.148660265884822));
#33544=DIRECTION('ref_axis',(0.797368987123014,0.089715294026903,0.596786280331648));
#33545=DIRECTION('center_axis',(-0.946369376470755,-0.140097818247825,0.291131593271074));
#33546=DIRECTION('ref_axis',(-0.0114718087515988,0.915097062809347,0.40307041970563));
#33547=DIRECTION('center_axis',(0.946369839460991,-0.140099137680288,0.291129453301823));
#33548=DIRECTION('ref_axis',(0.01147414714799,0.915097223790106,0.40306998766823));
#33549=DIRECTION('center_axis',(5.69602678185428E-6,-0.988889644020132,
0.148651511654917));
#33550=DIRECTION('ref_axis',(-0.999999999968588,-4.81341389039569E-6,6.29722243877274E-6));
#33551=DIRECTION('center_axis',(-0.946369839460985,0.1400991376803,-0.291129453301837));
#33552=DIRECTION('ref_axis',(-0.149612220002691,0.608622425476191,0.779227134302538));
#33553=DIRECTION('center_axis',(-4.95681495424892E-17,0.403096527878055,
-0.915157466894445));
#33554=DIRECTION('ref_axis',(-0.999999999986845,-4.69420780203386E-6,-2.06764292981134E-6));
#33555=DIRECTION('center_axis',(5.69064726501455E-6,-0.594138082881513,
-0.804363063819751));
#33556=DIRECTION('ref_axis',(-0.271605533892207,0.774125062247253,-0.571804881021329));
#33557=DIRECTION('center_axis',(-0.946369839249996,-0.106794560471235,0.304924661534112));
#33558=DIRECTION('ref_axis',(-0.149612220115205,0.981357835021728,-0.120635746085756));
#33559=DIRECTION('center_axis',(0.946369839249992,0.106794560471264,-0.304924661534114));
#33560=DIRECTION('ref_axis',(-0.271594468689797,0.774133377076023,-0.571798879916688));
#33561=DIRECTION('center_axis',(2.16840404869328E-18,-0.362081762350744,
0.93214633903319));
#33562=DIRECTION('ref_axis',(0.0114792119266392,0.932084921473315,0.362057905390321));
#33563=DIRECTION('center_axis',(1.,1.42364623010903E-9,-3.43713428943404E-9));
#33564=DIRECTION('ref_axis',(8.26276396146569E-11,0.915158418800611,0.403094366741047));
#33565=DIRECTION('center_axis',(0.999999999985404,-4.99170952627699E-6,
-2.06763424365629E-6));
#33566=DIRECTION('ref_axis',(5.40165508683492E-6,0.915152953201646,0.403106775206182));
#33567=DIRECTION('center_axis',(-0.946369788026362,0.106794703559617,-0.304924770398459));
#33568=DIRECTION('ref_axis',(-0.0114740731618296,0.932084948692918,0.362057998206362));
#33569=DIRECTION('center_axis',(0.,0.362081724527009,-0.932146353725394));
#33570=DIRECTION('ref_axis',(0.703038340194793,0.662897694664692,0.257495123496325));
#33571=DIRECTION('center_axis',(8.39574346860379E-6,-0.594120071126927,
-0.804376367761788));
#33572=DIRECTION('ref_axis',(0.999999999695544,2.3652778284159E-5,-7.03258707988771E-6));
#33573=DIRECTION('center_axis',(0.914210471289562,-0.316088169069029,0.253589202370894));
#33574=DIRECTION('ref_axis',(-0.277774690008402,-0.944426060401927,-0.17578577310019));
#33575=DIRECTION('center_axis',(0.,-0.594130960497972,0.804368324698181));
#33576=DIRECTION('ref_axis',(1.,0.,0.));
#33577=DIRECTION('center_axis',(0.,0.403096565020755,0.915157450534316));
#33578=DIRECTION('ref_axis',(1.,0.,0.));
#33579=DIRECTION('center_axis',(0.99999999999897,-1.32419981462018E-6,5.53416423203211E-7));
#33580=DIRECTION('ref_axis',(1.43473013400941E-6,0.932145037436602,-0.362085113171279));
#33581=DIRECTION('center_axis',(-3.66026653431106E-16,-0.362081725112371,
-0.932146353498017));
#33582=DIRECTION('ref_axis',(-0.0114743075678202,0.932084988407572,-0.36205788853593));
#33583=DIRECTION('center_axis',(1.,-5.07454201753425E-10,2.03628947473516E-10));
#33584=DIRECTION('ref_axis',(5.46751918028468E-10,0.932145992118772,-0.362082655448878));
#33585=DIRECTION('center_axis',(5.32906986477686E-15,0.59413096049796,-0.804368324698189));
#33586=DIRECTION('ref_axis',(0.797368987123025,0.485429918524157,0.358553332959033));
#33587=DIRECTION('center_axis',(-0.946369376471585,0.106797006503074,0.304925241130946));
#33588=DIRECTION('ref_axis',(-0.0114718087598166,0.932085165620904,-0.362057511499527));
#33589=DIRECTION('center_axis',(0.946369839460996,0.10679456034074,0.304924660924952));
#33590=DIRECTION('ref_axis',(0.0114741471479901,0.932084973959935,-0.362057930814027));
#33591=DIRECTION('center_axis',(-0.914215241706711,-0.316082336098155,-0.253579274858719));
#33592=DIRECTION('ref_axis',(0.277774402486775,-0.94442900415313,0.175770411154555));
#33593=DIRECTION('center_axis',(5.69660925919776E-6,-0.594138082100489,
0.804363064396608));
#33594=DIRECTION('ref_axis',(-0.999999999968596,1.04716010024955E-6,7.85561549530932E-6));
#33595=DIRECTION('center_axis',(-0.946369839460982,-0.106794560340743,-0.304924660924994));
#33596=DIRECTION('ref_axis',(-0.149612220002695,0.981357834986306,0.120635746513443));
#33597=DIRECTION('center_axis',(2.5539691584425E-16,-0.362081762359287,
-0.932146339029872));
#33598=DIRECTION('ref_axis',(-0.999999999986845,-4.78135051973835E-6,1.85726183743932E-6));
#33599=DIRECTION('center_axis',(5.691173724172E-6,-0.988889644483067,-0.148651508575471));
#33600=DIRECTION('ref_axis',(-0.27160553388917,0.143061970992072,-0.951716190057016));
#33601=DIRECTION('center_axis',(-0.946369839249997,0.140099138018724,0.291129453824832));
#33602=DIRECTION('ref_axis',(-0.149612220115206,0.6086224258037,-0.779227134025131));
#33603=DIRECTION('center_axis',(0.946369839249986,-0.140099138018723,-0.291129453824869));
#33604=DIRECTION('ref_axis',(-0.271594468689809,0.143072095009363,-0.951717825937253));
#33605=DIRECTION('center_axis',(-4.62303743181407E-16,0.403096527886377,
0.915157466890779));
#33606=DIRECTION('ref_axis',(0.0114792119266392,0.915097168699214,-0.403069968531799));
#33607=DIRECTION('center_axis',(1.,-1.42372070955575E-9,-3.43716518285929E-9));
#33608=DIRECTION('ref_axis',(8.25724334042756E-11,0.932145483973677,-0.362083963615458));
#33609=DIRECTION('center_axis',(0.999999999985404,-4.99170901781618E-6,
2.06763312228972E-6));
#33610=DIRECTION('ref_axis',(5.40165418784382E-6,0.93215039391184,-0.36207132322351));
#33611=DIRECTION('center_axis',(-0.946369788026357,-0.1400991138187,-0.291129631982323));
#33612=DIRECTION('ref_axis',(-0.0114740731618291,0.915097253577214,-0.403069922148152));
#33613=DIRECTION('center_axis',(-7.10542735092901E-15,-0.403096565020731,
-0.915157450534326));
#33614=DIRECTION('ref_axis',(0.703038340194823,0.650816003077036,-0.286662907183576));
#33615=DIRECTION('center_axis',(8.39582282804934E-6,-0.988886315401232,
-0.148673653152415));
#33616=DIRECTION('ref_axis',(0.999999999695544,1.17523290285004E-5,-2.16978224223302E-5));
#33617=DIRECTION('center_axis',(0.914211011085666,-0.0441933407252092,0.402821518597591));
#33618=DIRECTION('ref_axis',(-0.277773809559331,-0.79210955948066,0.543510953433555));
#33619=DIRECTION('center_axis',(0.,0.148660265884823,0.988888328046728));
#33620=DIRECTION('ref_axis',(1.,0.,0.));
#33621=DIRECTION('center_axis',(0.,0.932146353725392,0.362081724527015));
#33622=DIRECTION('ref_axis',(1.,0.,0.));
#33623=DIRECTION('center_axis',(0.999999999998973,-5.4644975272136E-7,1.32480760523532E-6));
#33624=DIRECTION('ref_axis',(1.43267969207677E-6,0.403093238650518,-0.915158915681962));
#33625=DIRECTION('center_axis',(5.46437894932694E-17,-0.915157450787408,
-0.403096564446155));
#33626=DIRECTION('ref_axis',(-0.0114743075683094,0.403070027779414,-0.915097204110979));
#33627=DIRECTION('center_axis',(1.,-2.14814139094165E-10,5.02758452718822E-10));
#33628=DIRECTION('ref_axis',(5.46693998289738E-10,0.403095651075575,-0.915157853096371));
#33629=DIRECTION('center_axis',(-1.15463180403498E-14,-0.148660265884754,
-0.988888328046739));
#33630=DIRECTION('ref_axis',(0.797368987123014,0.596786280331648,-0.089715294026903));
#33631=DIRECTION('center_axis',(-0.946369373547254,0.291131604593958,0.140097814466623));
#33632=DIRECTION('ref_axis',(-0.0114717933272592,0.40307043850639,-0.915097054721587));
#33633=DIRECTION('center_axis',(0.946369839460991,0.291129453301823,0.140099137680288));
#33634=DIRECTION('ref_axis',(0.01147414714799,0.40306998766823,-0.915097223790106));
#33635=DIRECTION('center_axis',(5.69602883164937E-6,0.148651511653502,0.988889644020345));
#33636=DIRECTION('ref_axis',(-0.999999999968588,6.29722269189983E-6,4.81341592428572E-6));
#33637=DIRECTION('center_axis',(-0.946369839460985,-0.291129453301837,-0.1400991376803));
#33638=DIRECTION('ref_axis',(-0.149612220002691,0.779227134302538,-0.608622425476191));
#33639=DIRECTION('center_axis',(4.98146360964622E-17,-0.915157466894445,
-0.403096527878055));
#33640=DIRECTION('ref_axis',(-0.999999999986845,-2.06764294367606E-6,4.69420783326464E-6));
#33641=DIRECTION('center_axis',(5.69120438802073E-6,-0.804363063194495,
0.594138083727999));
#33642=DIRECTION('ref_axis',(-0.271605533891507,-0.571804881957827,-0.774125061555757));
#33643=DIRECTION('center_axis',(-0.946369839249996,0.304924661534112,0.106794560471235));
#33644=DIRECTION('ref_axis',(-0.149612220115205,-0.120635746085756,-0.981357835021728));
#33645=DIRECTION('center_axis',(0.946369839249991,-0.30492466153412,-0.106794560471258));
#33646=DIRECTION('ref_axis',(-0.271594468689797,-0.571798879916688,-0.774133377076023));
#33647=DIRECTION('center_axis',(-8.67361619477312E-19,0.93214633903319,
0.362081762350744));
#33648=DIRECTION('ref_axis',(0.0114792119266496,0.362057905390321,-0.932084921473315));
#33649=DIRECTION('center_axis',(1.,-3.47834350169931E-9,-1.44071563802809E-9));
#33650=DIRECTION('ref_axis',(8.36176223912445E-11,0.403094366741542,-0.915158418800393));
#33651=DIRECTION('center_axis',(0.999999999985404,-2.06763381357569E-6,
4.99170850549968E-6));
#33652=DIRECTION('ref_axis',(5.40165397924269E-6,0.403106775646763,-0.915152953007579));
#33653=DIRECTION('center_axis',(-0.946369788023275,-0.304924770411269,-0.10679470355039));
#33654=DIRECTION('ref_axis',(-0.0114740731721401,0.362057998196173,-0.932084948696749));
#33655=DIRECTION('center_axis',(0.,-0.932146353725394,-0.362081724527009));
#33656=DIRECTION('ref_axis',(0.703038340194793,0.257495123496325,-0.662897694664692));
#33657=DIRECTION('center_axis',(8.39572065812752E-6,-0.804376367758035,
0.594120071132009));
#33658=DIRECTION('ref_axis',(0.999999999695545,-7.03260613071095E-6,-2.36527656856413E-5));
#33659=DIRECTION('center_axis',(0.914195196760818,0.253611443836588,0.31611450105076));
#33660=DIRECTION('ref_axis',(-0.277797379909012,-0.175793291241973,0.944417987159289));
#33661=DIRECTION('center_axis',(-0.914213474905294,0.253579021042076,-0.31608764985195));
#33662=DIRECTION('ref_axis',(-0.263860852594192,-0.964502442909986,-0.0106060402099417));
#33663=DIRECTION('center_axis',(0.,0.804368324698181,0.594130960497972));
#33664=DIRECTION('ref_axis',(1.,0.,0.));
#33665=DIRECTION('center_axis',(0.,0.915157450534316,-0.403096565020755));
#33666=DIRECTION('ref_axis',(1.,0.,0.));
#33667=DIRECTION('center_axis',(0.99999999999897,5.53268491474173E-7,1.32429836705055E-6));
#33668=DIRECTION('ref_axis',(1.43476843527578E-6,-0.362085113182452,-0.932145037432262));
#33669=DIRECTION('center_axis',(-1.14361645153771E-15,-0.932146353498067,
0.362081725112241));
#33670=DIRECTION('ref_axis',(-0.0114743075683103,-0.362057888535797,-0.932084988407617));
#33671=DIRECTION('center_axis',(1.,2.03540282763477E-10,5.0724014766387E-10));
#33672=DIRECTION('ref_axis',(5.46520268530975E-10,-0.362082655389443,-0.932145992141859));
#33673=DIRECTION('center_axis',(5.32906986477686E-15,-0.804368324698189,
-0.59413096049796));
#33674=DIRECTION('ref_axis',(0.797368987123025,0.358553332959033,-0.485429918524157));
#33675=DIRECTION('center_axis',(-0.946369376469017,0.304925241133014,-0.106797006519928));
#33676=DIRECTION('ref_axis',(-0.0114718087425804,-0.362057511495606,-0.932085165622639));
#33677=DIRECTION('center_axis',(0.946369839461072,0.304924660924732,-0.106794560340695));
#33678=DIRECTION('ref_axis',(0.0114741471479501,-0.362057930814027,-0.932084973959935));
#33679=DIRECTION('center_axis',(5.6966045490687E-6,0.804363064404739,0.59413808208948));
#33680=DIRECTION('ref_axis',(-0.999999999968597,7.8555843946347E-6,-1.04712592387451E-6));
#33681=DIRECTION('center_axis',(-0.946369839461086,-0.304924660924705,0.10679456034065));
#33682=DIRECTION('ref_axis',(-0.149612220002605,0.120635746513636,-0.981357834986296));
#33683=DIRECTION('center_axis',(-8.80522392098827E-17,-0.932146339029872,
0.362081762359287));
#33684=DIRECTION('ref_axis',(-0.999999999986845,1.85726372854635E-6,4.78135538727166E-6));
#33685=DIRECTION('center_axis',(0.914218329687893,-0.402804400843518,-0.0441979674167706));
#33686=DIRECTION('ref_axis',(0.263856242961101,0.674512925090226,-0.689501411845313));
#33687=DIRECTION('center_axis',(5.69118558432375E-6,-0.148651508574067,
0.988889644483278));
#33688=DIRECTION('ref_axis',(-0.271605533890658,-0.951716190057283,-0.143061970987472));
#33689=DIRECTION('center_axis',(-0.946369839249939,0.291129453824956,-0.14009913801886));
#33690=DIRECTION('ref_axis',(-0.149612220115201,-0.779227134025074,-0.608622425803773));
#33691=DIRECTION('center_axis',(0.946369839249922,-0.291129453825002,0.140099138018879));
#33692=DIRECTION('ref_axis',(-0.271594468689889,-0.951717825937198,-0.143072095009577));
#33693=DIRECTION('center_axis',(-4.66640551278794E-16,0.915157466890779,
-0.403096527886377));
#33694=DIRECTION('ref_axis',(0.0114792119231403,-0.403069968531815,-0.915097168699251));
#33695=DIRECTION('center_axis',(1.,-3.48100020628989E-9,1.44187777759703E-9));
#33696=DIRECTION('ref_axis',(8.3625497048937E-11,-0.362083963618991,-0.932145483972304));
#33697=DIRECTION('center_axis',(0.999999999985404,2.06763318526536E-6,4.99170918161415E-6));
#33698=DIRECTION('ref_axis',(5.4016543633521E-6,-0.362071323230482,-0.932150393909132));
#33699=DIRECTION('center_axis',(-0.946369788023279,-0.291129631984834,0.140099113834277));
#33700=DIRECTION('ref_axis',(-0.0114740731721399,-0.403069922158076,-0.915097253572714));
#33701=DIRECTION('center_axis',(-7.10542735092901E-15,-0.915157450534326,
0.403096565020731));
#33702=DIRECTION('ref_axis',(0.703038340194823,-0.286662907183576,-0.650816003077037));
#33703=DIRECTION('center_axis',(8.39591592211414E-6,-0.148673653342516,
0.988886315372651));
#33704=DIRECTION('ref_axis',(0.999999999695531,-2.16983267807876E-5,-1.1752498999848E-5));
#33705=DIRECTION('center_axis',(0.914232678033534,0.402769058919062,0.0442232472019623));
#33706=DIRECTION('ref_axis',(-0.263805189109609,0.674511229537102,-0.68952260545046));
#33707=DIRECTION('center_axis',(0.,0.988888328046741,-0.148660265884739));
#33708=DIRECTION('ref_axis',(1.,0.,0.));
#33709=DIRECTION('center_axis',(0.,0.362081724527015,-0.932146353725391));
#33710=DIRECTION('ref_axis',(1.,0.,0.));
#33711=DIRECTION('center_axis',(0.99999999999897,1.32768040064921E-6,5.45217781452942E-7));
#33712=DIRECTION('ref_axis',(1.43481215715695E-6,-0.915158915917704,-0.403093238115296));
#33713=DIRECTION('center_axis',(-6.33174068731535E-17,-0.403096564446156,
0.915157450787408));
#33714=DIRECTION('ref_axis',(-0.0114743075687795,-0.915097204110974,-0.403070027779412));
#33715=DIRECTION('center_axis',(1.,5.02650926101981E-10,2.14770992296926E-10));
#33716=DIRECTION('ref_axis',(5.46578188866671E-10,-0.915157853076047,-0.403095651121716));
#33717=DIRECTION('center_axis',(-1.24344963511336E-14,-0.988888328046739,
0.148660265884755));
#33718=DIRECTION('ref_axis',(0.797368987123014,-0.0897152940269056,-0.596786280331648));
#33719=DIRECTION('center_axis',(-0.946369376466823,0.140097818233099,-0.29113159329094));
#33720=DIRECTION('ref_axis',(-0.0114718087263466,-0.915097062806538,-0.403070419712726));
#33721=DIRECTION('center_axis',(0.946369839461063,0.140099137680155,-0.291129453301653));
#33722=DIRECTION('ref_axis',(0.0114741471479502,-0.915097223790127,-0.403069987668184));
#33723=DIRECTION('center_axis',(-0.914215226225209,0.044196341358579,0.402811622906422));
#33724=DIRECTION('ref_axis',(0.277774424362039,0.792100604739657,0.54352368958621));
#33725=DIRECTION('center_axis',(5.69601044024649E-6,0.988889644017464,-0.148651511672664));
#33726=DIRECTION('ref_axis',(-0.999999999968588,4.81340434744809E-6,-6.29717598173139E-6));
#33727=DIRECTION('center_axis',(-0.946369839461086,-0.140099137680153,0.291129453301579));
#33728=DIRECTION('ref_axis',(-0.149612220002599,-0.608622425476095,-0.77922713430263));
#33729=DIRECTION('center_axis',(2.82299102089821E-17,-0.403096527878027,
0.915157466894457));
#33730=DIRECTION('ref_axis',(-0.999999999986845,4.69421254877053E-6,2.06764502067634E-6));
#33731=DIRECTION('center_axis',(5.69062401486436E-6,0.594138082870581,0.804363063827826));
#33732=DIRECTION('ref_axis',(-0.271605533887031,-0.774125062259951,0.571804881006597));
#33733=DIRECTION('center_axis',(-0.946369839249936,0.106794560471239,-0.304924661534296));
#33734=DIRECTION('ref_axis',(-0.149612220115201,-0.981357835021745,0.120635746085621));
#33735=DIRECTION('center_axis',(0.946369839249922,-0.106794560471299,0.304924661534318));
#33736=DIRECTION('ref_axis',(-0.271594468689908,-0.774133377076162,0.571798879916447));
#33737=DIRECTION('center_axis',(6.07153133634118E-18,0.362081762350716,
-0.932146339033201));
#33738=DIRECTION('ref_axis',(0.0114792119231299,-0.932084921473364,-0.362057905390307));
#33739=DIRECTION('center_axis',(1.,-1.44189805230485E-9,3.48090292427251E-9));
#33740=DIRECTION('ref_axis',(8.35672300487615E-11,-0.915158418800003,-0.403094366742427));
#33741=DIRECTION('center_axis',(0.999999999985404,4.99170888905771E-6,2.06763397278594E-6));
#33742=DIRECTION('ref_axis',(5.40165439448914E-6,-0.915152953203479,-0.403106775202021));
#33743=DIRECTION('center_axis',(-0.94636978802022,-0.106794703541145,0.304924770423991));
#33744=DIRECTION('ref_axis',(-0.0114740731824407,-0.932084948700573,-0.362057998186));
#33745=DIRECTION('center_axis',(0.,-0.362081724527009,0.932146353725394));
#33746=DIRECTION('ref_axis',(0.703038340194793,-0.662897694664692,-0.257495123496325));
#33747=DIRECTION('center_axis',(8.39592187383702E-6,0.594120070955224,0.804376367888607));
#33748=DIRECTION('ref_axis',(0.999999999695531,-2.36533086150239E-5,7.03275698865841E-6));
#33749=DIRECTION('center_axis',(0.,0.594130960497972,-0.804368324698181));
#33750=DIRECTION('ref_axis',(1.,0.,0.));
#33751=DIRECTION('center_axis',(0.,-0.403096565020755,-0.915157450534316));
#33752=DIRECTION('ref_axis',(1.,0.,0.));
#33753=DIRECTION('center_axis',(0.999999999998959,1.33168050215377E-6,-5.56325015337109E-7));
#33754=DIRECTION('ref_axis',(1.44275637767322E-6,-0.932145037436202,0.362085113172275));
#33755=DIRECTION('center_axis',(-3.49546780409327E-16,0.362081725112241,
0.932146353498067));
#33756=DIRECTION('ref_axis',(-0.01147430756877,-0.932084988407612,0.362057888535795));
#33757=DIRECTION('center_axis',(1.,5.0702609627477E-10,-2.034516191357E-10));
#33758=DIRECTION('ref_axis',(5.46288644440416E-10,-0.932145992141857,0.362082655389447));
#33759=DIRECTION('center_axis',(5.32906986477153E-15,-0.59413096049796,
0.804368324698189));
#33760=DIRECTION('ref_axis',(0.797368987123024,-0.485429918524159,-0.358553332959033));
#33761=DIRECTION('center_axis',(-0.946369376467426,-0.106797006532308,-0.304925241133614));
#33762=DIRECTION('ref_axis',(-0.0114718087296023,-0.932085165623876,0.362057511492832));
#33763=DIRECTION('center_axis',(0.946369839461072,-0.106794560340695,-0.304924660924732));
#33764=DIRECTION('ref_axis',(0.0114741471479501,-0.932084973959935,0.362057930814027));
#33765=DIRECTION('center_axis',(5.69661023326282E-6,0.594138082092942,-0.804363064402183));
#33766=DIRECTION('ref_axis',(-0.999999999968597,-1.04711976004056E-6,-7.85558690927704E-6));
#33767=DIRECTION('center_axis',(-0.946369839461086,0.10679456034065,0.304924660924705));
#33768=DIRECTION('ref_axis',(-0.149612220002605,-0.981357834986296,-0.120635746513635));
#33769=DIRECTION('center_axis',(-9.82680269052054E-16,0.362081762359287,
0.932146339029872));
#33770=DIRECTION('ref_axis',(-0.999999999986845,4.78135531787353E-6,-1.85726370254917E-6));
#33771=DIRECTION('center_axis',(0.914207423386785,-0.0441978182448416,0.402829169607777));
#33772=DIRECTION('ref_axis',(0.277780035610593,0.792112742359119,-0.54350313265748));
#33773=DIRECTION('center_axis',(5.69063497141659E-6,0.988889644328729,0.14865150960221));
#33774=DIRECTION('ref_axis',(-0.271605533888581,-0.143061972124941,0.951716189886891));
#33775=DIRECTION('center_axis',(-0.946369839249939,-0.14009913801886,-0.291129453824956));
#33776=DIRECTION('ref_axis',(-0.149612220115201,-0.608622425803773,0.779227134025074));
#33777=DIRECTION('center_axis',(0.946369839249922,0.140099138018879,0.291129453825002));
#33778=DIRECTION('ref_axis',(-0.271594468689889,-0.143072095009577,0.951717825937198));
#33779=DIRECTION('center_axis',(-4.64905828039839E-16,-0.403096527886377,
-0.915157466890779));
#33780=DIRECTION('ref_axis',(0.0114792119231195,-0.915097168699251,0.403069968531815));
#33781=DIRECTION('center_axis',(1.,1.44185618820045E-9,3.48094808359834E-9));
#33782=DIRECTION('ref_axis',(8.36242449135707E-11,-0.932145483976129,0.362083963609144));
#33783=DIRECTION('center_axis',(0.999999999985404,4.99171031427304E-6,-2.06763364991969E-6));
#33784=DIRECTION('ref_axis',(5.401655587451E-6,-0.93215039373556,0.362071323677343));
#33785=DIRECTION('center_axis',(-0.946369788020201,0.140099113849831,0.291129631987354));
#33786=DIRECTION('ref_axis',(-0.0114740731824505,-0.915097253568243,0.403069922167932));
#33787=DIRECTION('center_axis',(-7.10542735092901E-15,0.403096565020731,
0.915157450534326));
#33788=DIRECTION('ref_axis',(0.703038340194823,-0.650816003077036,0.286662907183576));
#33789=DIRECTION('center_axis',(8.39589975016415E-6,0.988886315372978,0.148673653340339));
#33790=DIRECTION('ref_axis',(0.999999999695531,-1.1752482826665E-5,2.16983279843357E-5));
#33791=DIRECTION('center_axis',(0.91423776319055,0.0441882734077247,-0.402761354712172));
#33792=DIRECTION('ref_axis',(-0.277733517155144,0.792111374696756,-0.543528898518422));
#33793=DIRECTION('center_axis',(0.,-0.804368324698238,-0.594130960497894));
#33794=DIRECTION('ref_axis',(1.,0.,0.));
#33795=DIRECTION('center_axis',(-0.946369376471938,-0.304925241130843,0.106797006500241));
#33796=DIRECTION('ref_axis',(-0.0114718087725454,0.362057511526751,0.932085165610172));
#33797=DIRECTION('center_axis',(0.946369839460996,-0.304924660924952,0.10679456034074));
#33798=DIRECTION('ref_axis',(0.0114741471479901,0.362057930814027,0.932084973959935));
#33799=DIRECTION('center_axis',(6.21724817557921E-15,0.804368324698188,
0.594130960497961));
#33800=DIRECTION('ref_axis',(0.797368987123025,-0.358553332959034,0.485429918524156));
#33801=DIRECTION('center_axis',(-3.62123525610159E-16,0.932146353497273,
-0.362081725114285));
#33802=DIRECTION('ref_axis',(-0.0114743075668696,0.362057888537847,0.932084988406839));
#33803=DIRECTION('center_axis',(0.,-0.915157450534316,0.403096565020755));
#33804=DIRECTION('ref_axis',(1.,0.,0.));
#33805=DIRECTION('center_axis',(0.99999999999897,-5.53543085154133E-7,-1.32450328423587E-6));
#33806=DIRECTION('ref_axis',(1.43505887409419E-6,0.36208511306403,0.932145037478261));
#33807=DIRECTION('center_axis',(1.,-2.03585803597008E-10,-5.07346683735424E-10));
#33808=DIRECTION('ref_axis',(5.46636077372728E-10,0.362082655398668,0.932145992138275));
#33809=DIRECTION('center_axis',(1.,3.43715707468504E-9,-1.42371735165538E-9));
#33810=DIRECTION('ref_axis',(8.25722386253937E-11,0.362083963618065,0.932145483972664));
#33811=DIRECTION('center_axis',(-0.946369788029458,0.291129631979785,-0.140099113803026));
#33812=DIRECTION('ref_axis',(-0.0114740731514592,0.403069922138164,0.915097253581743));
#33813=DIRECTION('center_axis',(0.946369839249986,0.291129453824869,-0.140099138018723));
#33814=DIRECTION('ref_axis',(-0.271594468689809,0.951717825937253,0.143072095009363));
#33815=DIRECTION('center_axis',(-6.21724893205666E-15,0.915157450534326,
-0.403096565020732));
#33816=DIRECTION('ref_axis',(0.703038340194823,0.286662907183576,0.650816003077036));
#33817=DIRECTION('center_axis',(8.39574223448429E-6,0.148673653134807,-0.98888631540388));
#33818=DIRECTION('ref_axis',(0.999999999695544,2.16978339305183E-5,1.17522492591548E-5));
#33819=DIRECTION('center_axis',(0.914205544031138,-0.4028338123391,-0.0441943763286409));
#33820=DIRECTION('ref_axis',(-0.277781996737481,-0.543507170848629,-0.792109283826832));
#33821=DIRECTION('center_axis',(0.914204745777582,0.402835190649233,0.0441983254472605));
#33822=DIRECTION('ref_axis',(0.27778213558618,-0.543496513633425,-0.792116547496323));
#33823=DIRECTION('center_axis',(5.69119916378401E-6,0.148651508534004,-0.988889644489301));
#33824=DIRECTION('ref_axis',(-0.271605533901061,0.951716190060724,0.143061970944832));
#33825=DIRECTION('center_axis',(-0.946369839249997,-0.291129453824832,0.140099138018724));
#33826=DIRECTION('ref_axis',(-0.149612220115206,0.779227134025131,0.6086224258037));
#33827=DIRECTION('center_axis',(3.61689795277913E-16,-0.915157466892033,
0.40309652788353));
#33828=DIRECTION('ref_axis',(0.0114792119270605,0.40306996852895,0.915097168700464));
#33829=DIRECTION('center_axis',(-5.78221668413099E-16,0.932146339028668,
-0.362081762362386));
#33830=DIRECTION('ref_axis',(-0.999999999986845,-1.85727697257704E-6,-4.78138948141498E-6));
#33831=DIRECTION('center_axis',(0.999999999985307,-2.07451115399164E-6,
-5.00831315533298E-6));
#33832=DIRECTION('ref_axis',(5.41962207941293E-6,0.362071324606221,0.932150393374655));
#33833=DIRECTION('center_axis',(-0.946369839460982,0.304924660924994,-0.106794560340743));
#33834=DIRECTION('ref_axis',(-0.149612220002695,-0.120635746513443,0.981357834986306));
#33835=DIRECTION('center_axis',(5.69602760281014E-6,-0.804363065044909,
-0.594138081222803));
#33836=DIRECTION('ref_axis',(-0.999999999968588,-7.85643176174389E-6,1.04924418822824E-6));
#33837=DIRECTION('center_axis',(-0.914212817311013,-0.402816410519734,0.0442025347718617));
#33838=DIRECTION('ref_axis',(-0.263860258991997,0.674506642529295,0.689506020937115));
#33839=DIRECTION('center_axis',(0.,-0.148660265884688,-0.988888328046749));
#33840=DIRECTION('ref_axis',(1.,0.,0.));
#33841=DIRECTION('center_axis',(0.,-0.932146353725392,-0.362081724527015));
#33842=DIRECTION('ref_axis',(1.,0.,0.));
#33843=DIRECTION('center_axis',(0.99999999999897,5.47330121552162E-7,-1.32692265765345E-6));
#33844=DIRECTION('ref_axis',(1.43497017188914E-6,-0.403093238651766,0.915158915681408));
#33845=DIRECTION('center_axis',(5.03069808033274E-17,0.915157450787411,
0.403096564446147));
#33846=DIRECTION('ref_axis',(-0.0114743075692297,-0.403070027779401,0.915097204110973));
#33847=DIRECTION('center_axis',(1.,2.14836896434712E-10,-5.02811714092292E-10));
#33848=DIRECTION('ref_axis',(5.46751921211513E-10,-0.403095651121802,0.915157853076009));
#33849=DIRECTION('center_axis',(-1.24344963511336E-14,0.148660265884755,
0.988888328046739));
#33850=DIRECTION('ref_axis',(0.797368987123014,-0.596786280331648,0.0897152940269056));
#33851=DIRECTION('center_axis',(-0.946369373540832,-0.291131604623066,-0.140097814449519));
#33852=DIRECTION('ref_axis',(-0.0114717932857128,-0.403070438540629,0.915097054707027));
#33853=DIRECTION('center_axis',(0.946369839461063,-0.291129453301653,-0.140099137680155));
#33854=DIRECTION('ref_axis',(0.0114741471479502,-0.403069987668184,0.915097223790127));
#33855=DIRECTION('center_axis',(-0.914214770745398,0.402812647158067,-0.0441964279150493));
#33856=DIRECTION('ref_axis',(0.277778098123834,0.54353084089538,-0.792094409270932));
#33857=DIRECTION('center_axis',(5.69660473288689E-6,-0.148651510563523,
-0.988889644184189));
#33858=DIRECTION('ref_axis',(-0.999999999968597,-6.29516651701536E-6,-4.81430738979412E-6));
#33859=DIRECTION('center_axis',(-0.946369839461086,0.291129453301579,0.140099137680153));
#33860=DIRECTION('ref_axis',(-0.149612220002599,-0.77922713430263,0.608622425476095));
#33861=DIRECTION('center_axis',(-5.33840324484981E-17,0.915157466894457,
0.403096527878027));
#33862=DIRECTION('ref_axis',(-0.999999999986845,2.06764506632629E-6,-4.69421265261294E-6));
#33863=DIRECTION('center_axis',(5.69062333891971E-6,0.804363063828125,-0.594138082870176));
#33864=DIRECTION('ref_axis',(-0.271605533887638,0.571804881005956,0.774125062260211));
#33865=DIRECTION('center_axis',(-0.946369839249936,-0.304924661534296,-0.106794560471239));
#33866=DIRECTION('ref_axis',(-0.149612220115201,0.120635746085621,0.981357835021745));
#33867=DIRECTION('center_axis',(0.946369839249921,0.304924661534324,0.106794560471294));
#33868=DIRECTION('ref_axis',(-0.271594468689907,0.571798879916447,0.774133377076162));
#33869=DIRECTION('center_axis',(6.07153133634118E-18,-0.932146339033201,
-0.362081762350716));
#33870=DIRECTION('ref_axis',(0.0114792119231299,-0.362057905390307,0.932084921473364));
#33871=DIRECTION('center_axis',(1.,3.48092280083978E-9,1.44184515186693E-9));
#33872=DIRECTION('ref_axis',(8.3623632745154E-11,-0.403094366742872,0.915158418799807));
#33873=DIRECTION('center_axis',(0.999999999985404,2.06763417181339E-6,-4.99170934833527E-6));
#33874=DIRECTION('ref_axis',(5.40165489491138E-6,-0.403106776244474,0.915152952744299));
#33875=DIRECTION('center_axis',(-0.946369788017145,0.304924770436739,0.106794703531991));
#33876=DIRECTION('ref_axis',(-0.0114740731926795,-0.362057998175877,0.93208494870438));
#33877=DIRECTION('center_axis',(0.,0.932146353725394,0.362081724527009));
#33878=DIRECTION('ref_axis',(0.703038340194793,-0.257495123496325,0.662897694664692));
#33879=DIRECTION('center_axis',(8.39546862823305E-6,0.804376367829452,-0.594120071035321));
#33880=DIRECTION('ref_axis',(0.999999999695535,7.03312350208447E-6,2.36530419473628E-5));
#33881=DIRECTION('center_axis',(0.91416849261592,-0.253716090150975,-0.316107754898293));
#33882=DIRECTION('ref_axis',(-0.263983855302915,-0.964467992945735,0.0106777676803009));
#33883=DIRECTION('center_axis',(1.,0.,0.));
#33884=DIRECTION('ref_axis',(0.,0.8413441809447,0.54049974023166));
#33885=DIRECTION('center_axis',(-1.,0.,0.));
#33886=DIRECTION('ref_axis',(0.,0.54049869329636,0.8413448535202));
#33887=DIRECTION('center_axis',(1.,0.,0.));
#33888=DIRECTION('ref_axis',(0.,0.97711086402508,-0.212730720405307));
#33889=DIRECTION('center_axis',(-1.,0.,0.));
#33890=DIRECTION('ref_axis',(0.,0.977110930685622,0.212730414221093));
#33891=DIRECTION('center_axis',(1.,0.,0.));
#33892=DIRECTION('ref_axis',(0.,0.540499043132554,-0.841344628777526));
#33893=DIRECTION('center_axis',(-1.,0.,0.));
#33894=DIRECTION('ref_axis',(0.,0.841344788899846,-0.540498793884939));
#33895=DIRECTION('center_axis',(1.,0.,0.));
#33896=DIRECTION('ref_axis',(0.,-0.212729213948611,-0.977111192000586));
#33897=DIRECTION('center_axis',(-1.,0.,0.));
#33898=DIRECTION('ref_axis',(0.,0.212730320256165,-0.977110951143067));
#33899=DIRECTION('center_axis',(1.,0.,0.));
#33900=DIRECTION('ref_axis',(0.,-0.841345052956848,-0.540498382851456));
#33901=DIRECTION('center_axis',(-1.,0.,0.));
#33902=DIRECTION('ref_axis',(0.,-0.540502256823511,-0.841342564220242));
#33903=DIRECTION('center_axis',(1.,0.,0.));
#33904=DIRECTION('ref_axis',(0.,-0.977111001077189,0.212730090899086));
#33905=DIRECTION('center_axis',(-1.,0.,0.));
#33906=DIRECTION('ref_axis',(0.,-0.977111063757368,-0.212729802996537));
#33907=DIRECTION('center_axis',(1.,0.,0.));
#33908=DIRECTION('ref_axis',(0.,-0.540504506536072,0.84134111893702));
#33909=DIRECTION('center_axis',(-1.,0.,0.));
#33910=DIRECTION('ref_axis',(0.,-0.841344883607578,0.540498646462089));
#33911=DIRECTION('center_axis',(1.,0.,0.));
#33912=DIRECTION('ref_axis',(0.,0.212729805568991,0.977111063197311));
#33913=DIRECTION('center_axis',(-1.,0.,0.));
#33914=DIRECTION('ref_axis',(0.,-0.212725316405191,0.977112040535941));
#33915=DIRECTION('center_axis',(-1.,0.,0.));
#33916=DIRECTION('ref_axis',(0.,0.,1.));
#33917=DIRECTION('center_axis',(-1.,0.,0.));
#33918=DIRECTION('ref_axis',(0.,0.923879532497291,0.382683432398878));
#33919=DIRECTION('center_axis',(1.,0.,0.));
#33920=DIRECTION('ref_axis',(0.,-0.923879532497291,-0.382683432398878));
#33921=DIRECTION('center_axis',(-1.,0.,0.));
#33922=DIRECTION('ref_axis',(0.,-0.923879532497291,-0.382683432398878));
#33923=DIRECTION('',(-1.,0.,0.));
#33924=DIRECTION('center_axis',(-1.,0.,0.));
#33925=DIRECTION('ref_axis',(0.,0.,1.));
#33926=DIRECTION('center_axis',(-1.,0.,0.));
#33927=DIRECTION('ref_axis',(0.,-0.382683432398878,0.923879532497291));
#33928=DIRECTION('center_axis',(1.,0.,0.));
#33929=DIRECTION('ref_axis',(0.,0.382683432398878,-0.923879532497291));
#33930=DIRECTION('center_axis',(-1.,0.,0.));
#33931=DIRECTION('ref_axis',(0.,0.382683432398878,-0.923879532497291));
#33932=DIRECTION('',(-1.,0.,0.));
#33933=DIRECTION('center_axis',(-1.,0.,0.));
#33934=DIRECTION('ref_axis',(0.,0.,1.));
#33935=DIRECTION('center_axis',(-1.,0.,0.));
#33936=DIRECTION('ref_axis',(0.,-0.923879532497291,-0.382683432398878));
#33937=DIRECTION('center_axis',(1.,0.,0.));
#33938=DIRECTION('ref_axis',(0.,0.923879532497291,0.382683432398878));
#33939=DIRECTION('center_axis',(-1.,0.,0.));
#33940=DIRECTION('ref_axis',(0.,0.923879532497291,0.382683432398878));
#33941=DIRECTION('',(-1.,0.,0.));
#33942=DIRECTION('center_axis',(1.,0.,0.));
#33943=DIRECTION('ref_axis',(0.,1.,0.));
#33944=DIRECTION('center_axis',(-1.,0.,0.));
#33945=DIRECTION('ref_axis',(0.,-0.382683432398878,0.923879532497291));
#33946=DIRECTION('center_axis',(-1.,0.,0.));
#33947=DIRECTION('ref_axis',(0.,0.382683432398878,-0.923879532497291));
#33948=DIRECTION('center_axis',(1.,0.,0.));
#33949=DIRECTION('ref_axis',(0.,-0.382683432398878,0.923879532497291));
#33950=DIRECTION('',(-1.,0.,0.));
#33951=DIRECTION('center_axis',(-1.,0.,0.));
#33952=DIRECTION('ref_axis',(0.,0.,1.));
#33953=DIRECTION('center_axis',(-1.,0.,0.));
#33954=DIRECTION('ref_axis',(0.,0.382683432331302,0.923879532525282));
#33955=DIRECTION('center_axis',(1.,0.,0.));
#33956=DIRECTION('ref_axis',(0.,-0.382683432331302,-0.923879532525282));
#33957=DIRECTION('',(-1.,0.,0.));
#33958=DIRECTION('center_axis',(-1.,0.,0.));
#33959=DIRECTION('ref_axis',(0.,-0.382683432331302,-0.923879532525282));
#33960=DIRECTION('center_axis',(-1.,0.,0.));
#33961=DIRECTION('ref_axis',(0.,0.,1.));
#33962=DIRECTION('center_axis',(-1.,0.,0.));
#33963=DIRECTION('ref_axis',(0.,-0.923879532525282,0.382683432331302));
#33964=DIRECTION('center_axis',(1.,0.,0.));
#33965=DIRECTION('ref_axis',(0.,0.923879532525282,-0.382683432331302));
#33966=DIRECTION('',(-1.,0.,0.));
#33967=DIRECTION('center_axis',(-1.,0.,0.));
#33968=DIRECTION('ref_axis',(0.,0.923879532525282,-0.382683432331302));
#33969=DIRECTION('center_axis',(-1.,0.,0.));
#33970=DIRECTION('ref_axis',(0.,0.,1.));
#33971=DIRECTION('center_axis',(-1.,0.,0.));
#33972=DIRECTION('ref_axis',(0.,-0.382683432331302,-0.923879532525282));
#33973=DIRECTION('center_axis',(1.,0.,0.));
#33974=DIRECTION('ref_axis',(0.,0.382683432331302,0.923879532525282));
#33975=DIRECTION('',(-1.,0.,0.));
#33976=DIRECTION('center_axis',(-1.,0.,0.));
#33977=DIRECTION('ref_axis',(0.,0.382683432331302,0.923879532525282));
#33978=DIRECTION('center_axis',(1.,0.,0.));
#33979=DIRECTION('ref_axis',(0.,1.,0.));
#33980=DIRECTION('axis',(0.,0.,1.));
#33981=DIRECTION('refdir',(1.,0.,0.));
#33982=DIRECTION('center_axis',(0.,-1.,0.));
#33983=DIRECTION('ref_axis',(0.,0.,-1.));
#33984=DIRECTION('center_axis',(0.,-1.,0.));
#33985=DIRECTION('ref_axis',(-1.,0.,0.));
#33986=DIRECTION('',(-0.866025403761798,0.,0.500000000039214));
#33987=DIRECTION('',(0.,0.,1.));
#33988=DIRECTION('',(0.866025403761798,0.,0.500000000039214));
#33989=DIRECTION('',(0.866025403761798,0.,-0.500000000039214));
#33990=DIRECTION('',(0.,0.,-1.));
#33991=DIRECTION('',(-0.866025403761798,0.,-0.500000000039214));
#33992=DIRECTION('center_axis',(0.,1.,0.));
#33993=DIRECTION('ref_axis',(1.,0.,0.));
#33994=DIRECTION('center_axis',(0.,1.,0.));
#33995=DIRECTION('ref_axis',(-1.,0.,0.));
#33996=DIRECTION('center_axis',(0.,-1.,0.));
#33997=DIRECTION('ref_axis',(-1.,0.,0.));
#33998=DIRECTION('',(0.,1.,0.));
#33999=DIRECTION('center_axis',(0.,1.,0.));
#34000=DIRECTION('ref_axis',(1.,0.,0.));
#34001=DIRECTION('',(-0.866025403761798,0.,-0.500000000039214));
#34002=DIRECTION('',(0.,0.,-1.));
#34003=DIRECTION('',(0.866025403761798,0.,-0.500000000039214));
#34004=DIRECTION('',(0.866025403761798,0.,0.500000000039214));
#34005=DIRECTION('',(0.,0.,1.));
#34006=DIRECTION('',(-0.866025403761798,0.,0.500000000039214));
#34007=DIRECTION('center_axis',(0.500000000039214,0.,-0.866025403761798));
#34008=DIRECTION('ref_axis',(0.,-1.,0.));
#34009=DIRECTION('',(0.,-1.,0.));
#34010=DIRECTION('',(0.,-1.,0.));
#34011=DIRECTION('center_axis',(1.,0.,0.));
#34012=DIRECTION('ref_axis',(0.,1.,0.));
#34013=DIRECTION('',(0.,-1.,0.));
#34014=DIRECTION('center_axis',(0.500000000039214,0.,0.866025403761798));
#34015=DIRECTION('ref_axis',(0.,-1.,0.));
#34016=DIRECTION('',(0.,-1.,0.));
#34017=DIRECTION('center_axis',(-0.500000000039214,0.,0.866025403761798));
#34018=DIRECTION('ref_axis',(0.,1.,0.));
#34019=DIRECTION('',(0.,-1.,0.));
#34020=DIRECTION('center_axis',(-1.,0.,0.));
#34021=DIRECTION('ref_axis',(0.,0.,1.));
#34022=DIRECTION('',(0.,-1.,0.));
#34023=DIRECTION('center_axis',(-0.500000000039214,0.,-0.866025403761798));
#34024=DIRECTION('ref_axis',(-0.866025403761798,0.,0.500000000039214));
#34025=DIRECTION('axis',(0.,0.,1.));
#34026=DIRECTION('refdir',(1.,0.,0.));
#34027=DIRECTION('center_axis',(0.,-1.,0.));
#34028=DIRECTION('ref_axis',(0.,0.,-1.));
#34029=DIRECTION('center_axis',(0.,-1.,0.));
#34030=DIRECTION('ref_axis',(1.,0.,0.));
#34031=DIRECTION('center_axis',(0.,1.,0.));
#34032=DIRECTION('ref_axis',(1.,0.,0.));
#34033=DIRECTION('center_axis',(0.,-1.,0.));
#34034=DIRECTION('ref_axis',(1.,0.,0.));
#34035=DIRECTION('',(0.,1.,0.));
#34036=DIRECTION('center_axis',(0.,-1.,0.));
#34037=DIRECTION('ref_axis',(1.,0.,0.));
#34038=DIRECTION('center_axis',(0.,-1.,0.));
#34039=DIRECTION('ref_axis',(1.,0.,0.));
#34040=DIRECTION('center_axis',(0.,0.,-1.));
#34041=DIRECTION('ref_axis',(-1.,0.,0.));
#34042=DIRECTION('center_axis',(0.,-1.,0.));
#34043=DIRECTION('ref_axis',(1.,0.,0.));
#34044=DIRECTION('center_axis',(2.27272746077357E-11,1.,0.));
#34045=DIRECTION('ref_axis',(1.,-2.27272746077357E-11,0.));
#34046=DIRECTION('',(0.,0.,-1.));
#34047=DIRECTION('',(0.866025403795548,-1.96823971693366E-11,-0.499999999980758));
#34048=DIRECTION('',(0.866025403795548,-1.96823971693366E-11,0.499999999980758));
#34049=DIRECTION('',(0.,0.,1.));
#34050=DIRECTION('',(-0.866025403795548,1.96823971693366E-11,0.499999999980758));
#34051=DIRECTION('',(-0.866025403795548,1.96823971693366E-11,-0.499999999980758));
#34052=DIRECTION('center_axis',(0.,-1.,0.));
#34053=DIRECTION('ref_axis',(0.,0.,-1.));
#34054=DIRECTION('',(0.,0.,1.));
#34055=DIRECTION('',(0.866025403795548,0.,0.499999999980758));
#34056=DIRECTION('',(0.866025403795548,0.,-0.499999999980758));
#34057=DIRECTION('',(0.,0.,-1.));
#34058=DIRECTION('',(-0.866025403795548,0.,-0.499999999980758));
#34059=DIRECTION('',(-0.866025403795548,0.,0.499999999980758));
#34060=DIRECTION('center_axis',(-0.499999999980758,0.,-0.866025403795548));
#34061=DIRECTION('ref_axis',(-0.866025403795548,0.,0.499999999980758));
#34062=DIRECTION('',(0.,-1.,0.));
#34063=DIRECTION('',(0.,-1.,0.));
#34064=DIRECTION('center_axis',(0.499999999980758,0.,-0.866025403795548));
#34065=DIRECTION('ref_axis',(0.,-1.,0.));
#34066=DIRECTION('',(0.,-1.,0.));
#34067=DIRECTION('center_axis',(1.,0.,0.));
#34068=DIRECTION('ref_axis',(0.,1.,0.));
#34069=DIRECTION('',(0.,-1.,0.));
#34070=DIRECTION('center_axis',(0.499999999980758,0.,0.866025403795548));
#34071=DIRECTION('ref_axis',(0.,-1.,0.));
#34072=DIRECTION('',(0.,-1.,0.));
#34073=DIRECTION('center_axis',(-0.499999999980758,0.,0.866025403795548));
#34074=DIRECTION('ref_axis',(0.,1.,0.));
#34075=DIRECTION('',(0.,-1.,0.));
#34076=DIRECTION('center_axis',(-1.,0.,0.));
#34077=DIRECTION('ref_axis',(0.,0.,1.));
#34078=DIRECTION('center_axis',(0.,-1.,0.));
#34079=DIRECTION('ref_axis',(0.,0.,-1.));
#34080=DIRECTION('center_axis',(0.,-1.,0.));
#34081=DIRECTION('ref_axis',(1.,0.,0.));
#34082=DIRECTION('center_axis',(0.,1.,0.));
#34083=DIRECTION('ref_axis',(1.,0.,0.));
#34084=DIRECTION('center_axis',(0.,-1.,0.));
#34085=DIRECTION('ref_axis',(1.,0.,0.));
#34086=DIRECTION('',(0.707106781186547,-0.707106781186548,-8.65956056235493E-17));
#34087=DIRECTION('center_axis',(0.,-1.,0.));
#34088=DIRECTION('ref_axis',(1.,0.,0.));
#34089=DIRECTION('',(0.,1.,0.));
#34090=DIRECTION('axis',(0.,0.,1.));
#34091=DIRECTION('refdir',(1.,0.,0.));
#34092=DIRECTION('center_axis',(0.,1.,0.));
#34093=DIRECTION('ref_axis',(1.,0.,0.));
#34094=DIRECTION('center_axis',(0.,1.,0.));
#34095=DIRECTION('ref_axis',(1.,0.,0.));
#34096=DIRECTION('center_axis',(0.,-1.,0.));
#34097=DIRECTION('ref_axis',(1.,0.,0.));
#34098=DIRECTION('center_axis',(0.,1.,0.));
#34099=DIRECTION('ref_axis',(1.,0.,0.));
#34100=DIRECTION('',(0.,-1.,0.));
#34101=DIRECTION('center_axis',(0.,1.,0.));
#34102=DIRECTION('ref_axis',(1.,0.,0.));
#34103=DIRECTION('center_axis',(0.,1.,0.));
#34104=DIRECTION('ref_axis',(1.,0.,0.));
#34105=DIRECTION('center_axis',(0.,0.,1.));
#34106=DIRECTION('ref_axis',(-1.,0.,0.));
#34107=DIRECTION('center_axis',(0.,1.,0.));
#34108=DIRECTION('ref_axis',(1.,0.,0.));
#34109=DIRECTION('center_axis',(2.27272746077357E-11,-1.,0.));
#34110=DIRECTION('ref_axis',(0.,0.,-1.));
#34111=DIRECTION('',(0.,0.,1.));
#34112=DIRECTION('',(0.866025403795548,1.96823971693366E-11,0.499999999980758));
#34113=DIRECTION('',(0.866025403795548,1.96823971693366E-11,-0.499999999980758));
#34114=DIRECTION('',(0.,0.,-1.));
#34115=DIRECTION('',(-0.866025403795548,-1.96823971693366E-11,-0.499999999980758));
#34116=DIRECTION('',(-0.866025403795548,-1.96823971693366E-11,0.499999999980758));
#34117=DIRECTION('center_axis',(0.,1.,0.));
#34118=DIRECTION('ref_axis',(1.,0.,0.));
#34119=DIRECTION('',(0.,0.,-1.));
#34120=DIRECTION('',(0.866025403795548,0.,-0.499999999980758));
#34121=DIRECTION('',(0.866025403795548,0.,0.499999999980758));
#34122=DIRECTION('',(0.,0.,1.));
#34123=DIRECTION('',(-0.866025403795548,0.,0.499999999980758));
#34124=DIRECTION('',(-0.866025403795548,0.,-0.499999999980758));
#34125=DIRECTION('center_axis',(-0.499999999980758,0.,0.866025403795548));
#34126=DIRECTION('ref_axis',(0.,1.,0.));
#34127=DIRECTION('',(0.,1.,0.));
#34128=DIRECTION('',(0.,1.,0.));
#34129=DIRECTION('center_axis',(0.499999999980758,0.,0.866025403795548));
#34130=DIRECTION('ref_axis',(0.,-1.,0.));
#34131=DIRECTION('',(0.,1.,0.));
#34132=DIRECTION('center_axis',(1.,0.,0.));
#34133=DIRECTION('ref_axis',(0.,1.,0.));
#34134=DIRECTION('',(0.,1.,0.));
#34135=DIRECTION('center_axis',(0.499999999980758,0.,-0.866025403795548));
#34136=DIRECTION('ref_axis',(0.,-1.,0.));
#34137=DIRECTION('',(0.,1.,0.));
#34138=DIRECTION('center_axis',(-0.499999999980758,0.,-0.866025403795548));
#34139=DIRECTION('ref_axis',(-0.866025403795548,0.,0.499999999980758));
#34140=DIRECTION('',(0.,1.,0.));
#34141=DIRECTION('center_axis',(-1.,0.,0.));
#34142=DIRECTION('ref_axis',(0.,0.,1.));
#34143=DIRECTION('center_axis',(0.,1.,0.));
#34144=DIRECTION('ref_axis',(1.,0.,0.));
#34145=DIRECTION('center_axis',(0.,1.,0.));
#34146=DIRECTION('ref_axis',(1.,0.,0.));
#34147=DIRECTION('center_axis',(0.,-1.,0.));
#34148=DIRECTION('ref_axis',(1.,0.,0.));
#34149=DIRECTION('center_axis',(0.,1.,0.));
#34150=DIRECTION('ref_axis',(1.,0.,0.));
#34151=DIRECTION('',(0.707106781186547,0.707106781186548,8.65956056235493E-17));
#34152=DIRECTION('center_axis',(0.,1.,0.));
#34153=DIRECTION('ref_axis',(1.,0.,0.));
#34154=DIRECTION('',(0.,-1.,0.));
#34155=DIRECTION('axis',(0.,0.,1.));
#34156=DIRECTION('refdir',(1.,0.,0.));
#34157=DIRECTION('center_axis',(1.,0.,0.));
#34158=DIRECTION('ref_axis',(0.,1.,0.));
#34159=DIRECTION('',(0.,0.,-1.));
#34160=DIRECTION('center_axis',(1.,0.,0.));
#34161=DIRECTION('ref_axis',(0.,-0.707106781186548,0.707106781186548));
#34162=DIRECTION('',(0.,0.,-1.));
#34163=DIRECTION('center_axis',(-1.,0.,0.));
#34164=DIRECTION('ref_axis',(0.,-0.707106781186548,0.707106781186548));
#34165=DIRECTION('center_axis',(-1.,0.,0.));
#34166=DIRECTION('ref_axis',(0.,1.,8.30073289439369E-17));
#34167=DIRECTION('center_axis',(1.,0.,0.));
#34168=DIRECTION('ref_axis',(0.,-0.707106781186548,0.707106781186548));
#34169=DIRECTION('',(0.707104308763575,0.,-0.707109253600875));
#34170=DIRECTION('',(-0.707104308763575,0.,-0.707109253600875));
#34171=DIRECTION('center_axis',(-1.,0.,0.));
#34172=DIRECTION('ref_axis',(0.,0.,1.));
#34173=DIRECTION('center_axis',(1.,0.,0.));
#34174=DIRECTION('ref_axis',(0.,1.,0.));
#34175=DIRECTION('center_axis',(1.,0.,0.));
#34176=DIRECTION('ref_axis',(0.,-0.707106781186548,0.707106781186548));
#34177=DIRECTION('center_axis',(1.,0.,0.));
#34178=DIRECTION('ref_axis',(0.,0.,-1.));
#34179=DIRECTION('center_axis',(1.,0.,0.));
#34180=DIRECTION('ref_axis',(0.,0.707106781186547,-0.707106781186547));
#34181=DIRECTION('center_axis',(-1.,0.,0.));
#34182=DIRECTION('ref_axis',(0.,0.,1.));
#34183=DIRECTION('center_axis',(1.,0.,0.));
#34184=DIRECTION('ref_axis',(0.,0.,-1.));
#34185=DIRECTION('center_axis',(1.,0.,0.));
#34186=DIRECTION('ref_axis',(0.,-0.707106781186548,0.707106781186548));
#34187=DIRECTION('center_axis',(1.,0.,0.));
#34188=DIRECTION('ref_axis',(0.,-1.,0.));
#34189=DIRECTION('center_axis',(1.,0.,0.));
#34190=DIRECTION('ref_axis',(0.,0.707106781186547,-0.707106781186547));
#34191=DIRECTION('center_axis',(-1.,0.,0.));
#34192=DIRECTION('ref_axis',(0.,0.707106781186547,-0.707106781186547));
#34193=DIRECTION('center_axis',(1.,0.,0.));
#34194=DIRECTION('ref_axis',(0.,0.707106781186547,-0.707106781186547));
#34195=DIRECTION('',(-1.,0.,0.));
#34196=DIRECTION('',(1.,0.,0.));
#34197=DIRECTION('center_axis',(-1.,0.,0.));
#34198=DIRECTION('ref_axis',(0.,0.707106781186547,-0.707106781186547));
#34199=DIRECTION('',(-1.,0.,0.));
#34200=DIRECTION('',(1.,0.,0.));
#34201=DIRECTION('center_axis',(1.,0.,0.));
#34202=DIRECTION('ref_axis',(0.,0.707106781186547,-0.707106781186547));
#34203=DIRECTION('center_axis',(-1.,0.,0.));
#34204=DIRECTION('ref_axis',(0.,0.963284345089114,0.2684832778894));
#34205=DIRECTION('',(-1.,0.,0.));
#34206=DIRECTION('center_axis',(1.,0.,0.));
#34207=DIRECTION('ref_axis',(0.,-1.,0.));
#34208=DIRECTION('center_axis',(-1.,0.,0.));
#34209=DIRECTION('ref_axis',(0.,-0.2684832778894,0.963284345089114));
#34210=DIRECTION('',(-1.,0.,0.));
#34211=DIRECTION('center_axis',(1.,0.,0.));
#34212=DIRECTION('ref_axis',(0.,0.,-1.));
#34213=DIRECTION('center_axis',(-1.,0.,0.));
#34214=DIRECTION('ref_axis',(0.,0.,-1.));
#34215=DIRECTION('center_axis',(1.,0.,0.));
#34216=DIRECTION('ref_axis',(0.,0.,-1.));
#34217=DIRECTION('',(1.,0.,0.));
#34218=DIRECTION('center_axis',(-1.,0.,0.));
#34219=DIRECTION('ref_axis',(0.,1.,0.));
#34220=DIRECTION('center_axis',(1.,0.,0.));
#34221=DIRECTION('ref_axis',(0.,1.,0.));
#34222=DIRECTION('',(1.,0.,0.));
#34223=DIRECTION('center_axis',(1.,0.,0.));
#34224=DIRECTION('ref_axis',(0.,1.,-1.61486985400023E-16));
#34225=DIRECTION('center_axis',(1.,0.,0.));
#34226=DIRECTION('ref_axis',(0.,-0.707106781186548,0.707106781186548));
#34227=DIRECTION('center_axis',(1.,0.,0.));
#34228=DIRECTION('ref_axis',(0.,-0.707106781186548,0.707106781186548));
#34229=DIRECTION('',(1.,0.,0.));
#34230=DIRECTION('',(-1.,0.,0.));
#34231=DIRECTION('center_axis',(1.,0.,0.));
#34232=DIRECTION('ref_axis',(0.,-0.707106781186548,0.707106781186548));
#34233=DIRECTION('',(-1.,0.,0.));
#34234=DIRECTION('center_axis',(1.,0.,0.));
#34235=DIRECTION('ref_axis',(0.,1.,-1.85037170770859E-16));
#34236=DIRECTION('',(-1.,0.,0.));
#34237=DIRECTION('center_axis',(1.,0.,0.));
#34238=DIRECTION('ref_axis',(0.,-0.707106781186548,0.707106781186548));
#34239=DIRECTION('',(1.,0.,0.));
#34240=DIRECTION('center_axis',(1.,0.,0.));
#34241=DIRECTION('ref_axis',(0.,1.,0.));
#34242=DIRECTION('',(0.,0.,1.));
#34243=DIRECTION('',(0.,0.,1.));
#34244=DIRECTION('center_axis',(0.,-1.,0.));
#34245=DIRECTION('ref_axis',(1.,0.,0.));
#34246=DIRECTION('',(0.,-1.,0.));
#34247=DIRECTION('center_axis',(0.,-1.,0.));
#34248=DIRECTION('ref_axis',(1.,0.,0.));
#34249=DIRECTION('center_axis',(0.,-1.,0.));
#34250=DIRECTION('ref_axis',(0.,0.,-1.));
#34251=DIRECTION('center_axis',(0.,1.,0.));
#34252=DIRECTION('ref_axis',(1.,0.,0.));
#34253=DIRECTION('center_axis',(0.,1.,0.));
#34254=DIRECTION('ref_axis',(1.,0.,0.));
#34255=DIRECTION('center_axis',(0.,1.,0.));
#34256=DIRECTION('ref_axis',(1.,0.,0.));
#34257=DIRECTION('center_axis',(0.,1.,0.));
#34258=DIRECTION('ref_axis',(1.,0.,0.));
#34259=DIRECTION('',(0.,1.,0.));
#34260=DIRECTION('center_axis',(0.,-1.,0.));
#34261=DIRECTION('ref_axis',(0.,0.,-1.));
#34262=DIRECTION('center_axis',(0.,1.,0.));
#34263=DIRECTION('ref_axis',(1.,0.,0.));
#34264=DIRECTION('center_axis',(0.,1.,0.));
#34265=DIRECTION('ref_axis',(1.,0.,0.));
#34266=DIRECTION('center_axis',(0.,-1.,0.));
#34267=DIRECTION('ref_axis',(1.,0.,0.));
#34268=DIRECTION('',(0.,1.,0.));
#34269=DIRECTION('center_axis',(0.,-1.,0.));
#34270=DIRECTION('ref_axis',(0.,0.,-1.));
#34271=DIRECTION('center_axis',(0.,-1.,0.));
#34272=DIRECTION('ref_axis',(0.,0.,-1.));
#34273=DIRECTION('center_axis',(0.,1.,0.));
#34274=DIRECTION('ref_axis',(5.0532154980743E-16,0.,-1.));
#34275=DIRECTION('center_axis',(0.,-1.,0.));
#34276=DIRECTION('ref_axis',(5.0532154980743E-16,0.,1.));
#34277=DIRECTION('center_axis',(0.,-1.,0.));
#34278=DIRECTION('ref_axis',(1.,0.,0.));
#34279=DIRECTION('center_axis',(0.,1.,0.));
#34280=DIRECTION('ref_axis',(1.,0.,0.));
#34281=DIRECTION('',(-0.707104308763575,0.,0.707109253600875));
#34282=DIRECTION('',(0.,0.,1.));
#34283=DIRECTION('',(1.,0.,0.));
#34284=DIRECTION('',(0.,0.,-1.));
#34285=DIRECTION('',(-1.,0.,0.));
#34286=DIRECTION('center_axis',(0.,1.,0.));
#34287=DIRECTION('ref_axis',(1.,0.,0.));
#34288=DIRECTION('center_axis',(0.,1.,0.));
#34289=DIRECTION('ref_axis',(1.,0.,0.));
#34290=DIRECTION('',(0.,1.,0.));
#34291=DIRECTION('center_axis',(0.,-1.,0.));
#34292=DIRECTION('ref_axis',(1.,0.,0.));
#34293=DIRECTION('center_axis',(0.,1.,0.));
#34294=DIRECTION('ref_axis',(1.,0.,0.));
#34295=DIRECTION('',(0.,-1.,0.));
#34296=DIRECTION('center_axis',(0.,-1.,0.));
#34297=DIRECTION('ref_axis',(1.,0.,0.));
#34298=DIRECTION('center_axis',(0.,1.,0.));
#34299=DIRECTION('ref_axis',(1.,0.,0.));
#34300=DIRECTION('center_axis',(0.,-1.,0.));
#34301=DIRECTION('ref_axis',(1.,0.,0.));
#34302=DIRECTION('center_axis',(0.,-1.,0.));
#34303=DIRECTION('ref_axis',(1.,0.,0.));
#34304=DIRECTION('',(0.,-1.,0.));
#34305=DIRECTION('center_axis',(0.,-1.,0.));
#34306=DIRECTION('ref_axis',(1.,0.,0.));
#34307=DIRECTION('center_axis',(0.,1.,0.));
#34308=DIRECTION('ref_axis',(1.,0.,0.));
#34309=DIRECTION('',(-1.,0.,0.));
#34310=DIRECTION('center_axis',(0.,1.,0.));
#34311=DIRECTION('ref_axis',(1.,0.,0.));
#34312=DIRECTION('',(0.707104308763575,0.,0.707109253600875));
#34313=DIRECTION('',(1.,0.,0.));
#34314=DIRECTION('',(0.,0.,-1.));
#34315=DIRECTION('',(-1.,0.,0.));
#34316=DIRECTION('',(0.,0.,1.));
#34317=DIRECTION('center_axis',(1.,0.,0.));
#34318=DIRECTION('ref_axis',(0.,1.,0.));
#34319=DIRECTION('center_axis',(-1.,0.,0.));
#34320=DIRECTION('ref_axis',(0.,-0.707106781186548,0.707106781186548));
#34321=DIRECTION('',(0.,-1.,0.));
#34322=DIRECTION('',(0.,0.,1.));
#34323=DIRECTION('',(0.,1.,0.));
#34324=DIRECTION('center_axis',(-1.,0.,0.));
#34325=DIRECTION('ref_axis',(0.,-0.707106781186548,0.707106781186548));
#34326=DIRECTION('center_axis',(1.,0.,0.));
#34327=DIRECTION('ref_axis',(0.,-0.707106781186548,0.707106781186548));
#34328=DIRECTION('center_axis',(-1.,0.,0.));
#34329=DIRECTION('ref_axis',(0.,-0.707106781186548,0.707106781186548));
#34330=DIRECTION('center_axis',(1.,0.,0.));
#34331=DIRECTION('ref_axis',(0.,-0.707106781186548,0.707106781186548));
#34332=DIRECTION('center_axis',(1.,0.,0.));
#34333=DIRECTION('ref_axis',(0.,1.,0.));
#34334=DIRECTION('center_axis',(1.,0.,0.));
#34335=DIRECTION('ref_axis',(0.,-0.707106781186548,0.707106781186548));
#34336=DIRECTION('center_axis',(1.,0.,0.));
#34337=DIRECTION('ref_axis',(0.,-1.,0.));
#34338=DIRECTION('center_axis',(1.,0.,0.));
#34339=DIRECTION('ref_axis',(0.,0.707106781186547,-0.707106781186547));
#34340=DIRECTION('center_axis',(1.,0.,0.));
#34341=DIRECTION('ref_axis',(0.,0.,1.));
#34342=DIRECTION('center_axis',(1.,0.,0.));
#34343=DIRECTION('ref_axis',(0.,-0.707106781186548,0.707106781186548));
#34344=DIRECTION('center_axis',(1.,0.,0.));
#34345=DIRECTION('ref_axis',(0.,0.,1.));
#34346=DIRECTION('center_axis',(1.,0.,0.));
#34347=DIRECTION('ref_axis',(0.,0.707106781186547,-0.707106781186547));
#34348=DIRECTION('center_axis',(1.,0.,0.));
#34349=DIRECTION('ref_axis',(0.,1.,0.));
#34350=DIRECTION('center_axis',(1.,0.,0.));
#34351=DIRECTION('ref_axis',(0.,-0.707106781186548,0.707106781186548));
#34352=DIRECTION('center_axis',(1.,0.,0.));
#34353=DIRECTION('ref_axis',(0.,-0.707106781186548,0.707106781186548));
#34354=DIRECTION('',(0.,-1.,0.));
#34355=DIRECTION('',(0.,0.,-1.));
#34356=DIRECTION('',(0.,1.,0.));
#34357=DIRECTION('center_axis',(1.,0.,0.));
#34358=DIRECTION('ref_axis',(0.,-0.707106781186548,0.707106781186548));
#34359=DIRECTION('center_axis',(1.,0.,0.));
#34360=DIRECTION('ref_axis',(0.,-0.707106781186548,0.707106781186548));
#34361=DIRECTION('',(1.,0.,0.));
#34362=DIRECTION('',(1.,0.,0.));
#34363=DIRECTION('center_axis',(1.,0.,0.));
#34364=DIRECTION('ref_axis',(0.,-0.707106781186548,0.707106781186548));
#34365=DIRECTION('',(-1.,0.,0.));
#34366=DIRECTION('',(-1.,0.,0.));
#34367=DIRECTION('center_axis',(1.,0.,0.));
#34368=DIRECTION('ref_axis',(0.,-0.707106781186548,0.707106781186548));
#34369=DIRECTION('',(1.,0.,0.));
#34370=DIRECTION('',(-1.,0.,0.));
#34371=DIRECTION('center_axis',(1.,0.,0.));
#34372=DIRECTION('ref_axis',(0.,-0.707106781186548,0.707106781186548));
#34373=DIRECTION('center_axis',(0.,-1.,0.));
#34374=DIRECTION('ref_axis',(-1.,0.,0.));
#34375=DIRECTION('center_axis',(0.,1.,0.));
#34376=DIRECTION('ref_axis',(-1.,0.,0.));
#34377=DIRECTION('',(0.,-1.,0.));
#34378=DIRECTION('center_axis',(0.,1.,0.));
#34379=DIRECTION('ref_axis',(-1.,0.,0.));
#34380=DIRECTION('',(0.,1.,0.));
#34381=DIRECTION('',(0.,-1.,0.));
#34382=DIRECTION('center_axis',(0.,1.,0.));
#34383=DIRECTION('ref_axis',(-1.,0.,0.));
#34384=DIRECTION('',(0.,1.,0.));
#34385=DIRECTION('',(0.,-1.,0.));
#34386=DIRECTION('center_axis',(0.,0.,1.));
#34387=DIRECTION('ref_axis',(1.,0.,0.));
#34388=DIRECTION('',(1.,0.,0.));
#34389=DIRECTION('center_axis',(0.,0.,1.));
#34390=DIRECTION('ref_axis',(1.,0.,0.));
#34391=DIRECTION('',(1.,0.,0.));
#34392=DIRECTION('center_axis',(0.,-1.,0.));
#34393=DIRECTION('ref_axis',(0.,0.,-1.));
#34394=DIRECTION('',(-1.,0.,0.));
#34395=DIRECTION('center_axis',(0.,-1.,0.));
#34396=DIRECTION('ref_axis',(0.,0.,-1.));
#34397=DIRECTION('',(-1.,0.,0.));
#34398=DIRECTION('center_axis',(0.,0.,-1.));
#34399=DIRECTION('ref_axis',(0.,-1.,0.));
#34400=DIRECTION('center_axis',(0.,0.,-1.));
#34401=DIRECTION('ref_axis',(0.,-1.,0.));
#34402=DIRECTION('center_axis',(-1.,0.,0.));
#34403=DIRECTION('ref_axis',(0.,-0.963284345089114,-0.2684832778894));
#34404=DIRECTION('center_axis',(1.,0.,0.));
#34405=DIRECTION('ref_axis',(0.,1.,0.));
#34406=DIRECTION('',(-1.,0.,0.));
#34407=DIRECTION('',(1.,0.,0.));
#34408=DIRECTION('center_axis',(-1.,0.,0.));
#34409=DIRECTION('ref_axis',(0.,0.2684832778894,-0.963284345089114));
#34410=DIRECTION('center_axis',(1.,0.,0.));
#34411=DIRECTION('ref_axis',(0.,0.,1.));
#34412=DIRECTION('',(-1.,0.,0.));
#34413=DIRECTION('',(1.,0.,0.));
#34414=DIRECTION('center_axis',(-1.,0.,0.));
#34415=DIRECTION('ref_axis',(0.,-1.,0.));
#34416=DIRECTION('',(1.,0.,0.));
#34417=DIRECTION('center_axis',(1.,0.,0.));
#34418=DIRECTION('ref_axis',(0.,-1.,0.));
#34419=DIRECTION('',(-1.,0.,0.));
#34420=DIRECTION('center_axis',(-1.,0.,0.));
#34421=DIRECTION('ref_axis',(0.,-0.707106781186548,0.707106781186547));
#34422=DIRECTION('center_axis',(1.,0.,0.));
#34423=DIRECTION('ref_axis',(0.,0.707106781186547,-0.707106781186547));
#34424=DIRECTION('',(-1.,0.,0.));
#34425=DIRECTION('center_axis',(-1.,0.,0.));
#34426=DIRECTION('ref_axis',(0.,0.707106781186547,-0.707106781186547));
#34427=DIRECTION('center_axis',(1.,0.,0.));
#34428=DIRECTION('ref_axis',(0.,0.707106781186547,-0.707106781186547));
#34429=DIRECTION('center_axis',(-1.,0.,0.));
#34430=DIRECTION('ref_axis',(0.,0.,1.));
#34431=DIRECTION('',(1.,0.,0.));
#34432=DIRECTION('center_axis',(1.,0.,0.));
#34433=DIRECTION('ref_axis',(0.,0.,1.));
#34434=DIRECTION('center_axis',(-1.,0.,0.));
#34435=DIRECTION('ref_axis',(0.,0.,1.));
#34436=DIRECTION('center_axis',(1.,0.,0.));
#34437=DIRECTION('ref_axis',(0.,-0.707106781186548,0.707106781186548));
#34438=DIRECTION('center_axis',(-1.,0.,0.));
#34439=DIRECTION('ref_axis',(0.,0.,1.));
#34440=DIRECTION('center_axis',(1.,0.,0.));
#34441=DIRECTION('ref_axis',(0.,-0.707106781186548,0.707106781186548));
#34442=DIRECTION('center_axis',(1.,0.,0.));
#34443=DIRECTION('ref_axis',(0.,-0.707106781186548,0.707106781186548));
#34444=DIRECTION('center_axis',(0.946028810149189,0.229160959873926,0.229160958361957));
#34445=DIRECTION('ref_axis',(0.0238519321546227,-0.754422194584299,0.655955972341971));
#34446=DIRECTION('',(-1.,0.,0.));
#34447=DIRECTION('center_axis',(-0.946028810160763,-0.229160959093836,-0.229160959094266));
#34448=DIRECTION('ref_axis',(0.00756181520526069,-0.722522721083779,0.691305819784915));
#34449=DIRECTION('',(-1.,0.,0.));
#34450=DIRECTION('center_axis',(1.,0.,0.));
#34451=DIRECTION('ref_axis',(0.,-0.707106781186548,0.707106781186548));
#34452=DIRECTION('',(-1.,0.,0.));
#34453=DIRECTION('center_axis',(-1.,0.,0.));
#34454=DIRECTION('ref_axis',(0.,-0.707106781186548,0.707106781186548));
#34455=DIRECTION('',(1.,0.,0.));
#34456=DIRECTION('center_axis',(1.,0.,0.));
#34457=DIRECTION('ref_axis',(0.,-0.707106781186548,0.707106781186548));
#34458=DIRECTION('',(-1.,0.,0.));
#34459=DIRECTION('center_axis',(-1.,0.,0.));
#34460=DIRECTION('ref_axis',(0.,-0.707106781186548,0.707106781186548));
#34461=DIRECTION('',(-1.,0.,0.));
#34462=DIRECTION('center_axis',(-1.,0.,0.));
#34463=DIRECTION('ref_axis',(0.,-0.707106781186548,0.707106781186548));
#34464=DIRECTION('',(1.,0.,0.));
#34465=DIRECTION('center_axis',(1.,0.,0.));
#34466=DIRECTION('ref_axis',(0.,-0.707106781186548,0.707106781186548));
#34467=DIRECTION('',(-1.,0.,0.));
#34468=DIRECTION('',(1.,0.,0.));
#34469=DIRECTION('center_axis',(0.500000000011387,0.612372435691271,0.612372435691021));
#34470=DIRECTION('ref_axis',(0.866025403777864,-0.353553390477781,-0.353553390724871));
#34471=DIRECTION('center_axis',(-0.5000000000114,0.612372435691098,0.612372435691183));
#34472=DIRECTION('ref_axis',(0.866025403777857,0.35355339068672,0.353553390515949));
#34473=DIRECTION('',(1.,0.,0.));
#34474=DIRECTION('center_axis',(0.500000000001143,-0.612372435695232,-0.612372435695424));
#34475=DIRECTION('ref_axis',(0.866025403783779,0.35355339057273,0.353553390615434));
#34476=DIRECTION('center_axis',(-0.500000000001141,-0.612372435695253,-0.612372435695405));
#34477=DIRECTION('ref_axis',(0.86602540378378,-0.353553390639258,-0.353553390548903));
#34478=DIRECTION('center_axis',(-0.855183382509445,-0.366511515698828,-0.366511515698828));
#34479=DIRECTION('ref_axis',(0.518325556267202,-0.604705968930477,-0.604705968930477));
#34480=DIRECTION('',(-1.,0.,0.));
#34481=DIRECTION('center_axis',(-0.855183382508489,-0.366511515700201,-0.366511515699686));
#34482=DIRECTION('ref_axis',(0.00559375624135859,-0.713591574246071,0.7005396313244));
#34483=DIRECTION('center_axis',(1.,0.,0.));
#34484=DIRECTION('ref_axis',(0.,-0.707106781186548,0.707106781186548));
#34485=DIRECTION('',(-1.,0.,0.));
#34486=DIRECTION('center_axis',(-1.,0.,0.));
#34487=DIRECTION('ref_axis',(0.,-0.707106781186548,0.707106781186548));
#34488=DIRECTION('',(1.,0.,0.));
#34489=DIRECTION('center_axis',(1.,0.,0.));
#34490=DIRECTION('ref_axis',(0.,-0.707106781186548,0.707106781186548));
#34491=DIRECTION('center_axis',(-0.829037572548623,0.395409094042037,0.395409094042541));
#34492=DIRECTION('ref_axis',(0.0360858435025385,-0.667803081109337,0.74346274739195));
#34493=DIRECTION('',(1.,0.,0.));
#34494=DIRECTION('center_axis',(0.829037572553119,-0.395409094037575,-0.395409094037575));
#34495=DIRECTION('ref_axis',(-0.559192903473597,-0.586218089410745,-0.586218089410745));
#34496=DIRECTION('center_axis',(0.500000000011394,-0.612372435691112,-0.612372435691174));
#34497=DIRECTION('ref_axis',(0.86602540377786,0.353553390446867,0.353553390755794));
#34498=DIRECTION('',(-1.,0.,0.));
#34499=DIRECTION('center_axis',(-0.500000000001142,0.612372435695436,0.612372435695221));
#34500=DIRECTION('ref_axis',(0.866025403783779,0.353553390611745,0.353553390576418));
#34501=DIRECTION('center_axis',(0.500000000001144,0.612372435695425,0.61237243569523));
#34502=DIRECTION('ref_axis',(0.866025403783778,-0.353553390710462,-0.353553390477703));
#34503=DIRECTION('',(-1.,0.,0.));
#34504=DIRECTION('center_axis',(-0.500000000011398,-0.61237243569113,-0.612372435691153));
#34505=DIRECTION('ref_axis',(0.866025403777858,-0.353553390837826,-0.35355339036484));
#34506=DIRECTION('center_axis',(1.,0.,0.));
#34507=DIRECTION('ref_axis',(0.,-0.707106781186548,0.707106781186548));
#34508=DIRECTION('center_axis',(-1.,0.,0.));
#34509=DIRECTION('ref_axis',(0.,-0.707106781186548,0.707106781186548));
#34510=DIRECTION('',(1.,0.,0.));
#34511=DIRECTION('center_axis',(-1.,0.,0.));
#34512=DIRECTION('ref_axis',(0.,-0.707106781186548,0.707106781186548));
#34513=DIRECTION('',(-1.,0.,0.));
#34514=DIRECTION('center_axis',(1.,0.,0.));
#34515=DIRECTION('ref_axis',(0.,-0.707106781186548,0.707106781186548));
#34516=DIRECTION('',(1.,0.,0.));
#34517=DIRECTION('center_axis',(1.,0.,0.));
#34518=DIRECTION('ref_axis',(0.,-0.707106781186548,0.707106781186548));
#34519=DIRECTION('',(1.,0.,0.));
#34520=DIRECTION('center_axis',(-1.,0.,0.));
#34521=DIRECTION('ref_axis',(0.,0.,1.));
#34522=DIRECTION('',(0.,-0.707106781186547,0.707106781186547));
#34523=DIRECTION('',(0.,-0.707106781186547,0.707106781186547));
#34524=DIRECTION('center_axis',(0.,-0.707106781186548,-0.707106781186548));
#34525=DIRECTION('ref_axis',(0.,-0.707106781186548,0.707106781186548));
#34526=DIRECTION('',(0.,-0.707106781186547,0.707106781186547));
#34527=DIRECTION('center_axis',(0.,-0.707106781186548,-0.707106781186548));
#34528=DIRECTION('ref_axis',(0.,-0.707106781186548,0.707106781186548));
#34529=DIRECTION('',(0.,-0.707106781186547,0.707106781186547));
#34530=DIRECTION('center_axis',(-1.,0.,0.));
#34531=DIRECTION('ref_axis',(0.,0.,1.));
#34532=DIRECTION('',(0.,-0.707106781186547,0.707106781186547));
#34533=DIRECTION('center_axis',(0.,0.707106781186548,0.707106781186548));
#34534=DIRECTION('ref_axis',(1.,0.,0.));
#34535=DIRECTION('',(0.,-0.707106781186547,0.707106781186547));
#34536=DIRECTION('center_axis',(1.,0.,0.));
#34537=DIRECTION('ref_axis',(0.,1.,0.));
#34538=DIRECTION('',(0.,-0.707106781186547,0.707106781186547));
#34539=DIRECTION('center_axis',(0.,-0.707106781186548,-0.707106781186548));
#34540=DIRECTION('ref_axis',(0.,-0.707106781186548,0.707106781186548));
#34541=DIRECTION('',(0.,-0.707106781186547,0.707106781186547));
#34542=DIRECTION('center_axis',(1.,0.,0.));
#34543=DIRECTION('ref_axis',(0.,1.,0.));
#34544=DIRECTION('center_axis',(-0.855183382508501,-0.366511515699929,-0.366511515699929));
#34545=DIRECTION('ref_axis',(-0.393923250037275,2.21791245245237E-17,0.919143336525958));
#34546=DIRECTION('',(0.,-0.707106781186547,0.707106781186547));
#34547=DIRECTION('center_axis',(0.855183382508501,0.366511515699929,0.366511515699929));
#34548=DIRECTION('ref_axis',(0.518325556268759,-0.60470596892981,-0.60470596892981));
#34549=DIRECTION('',(0.,-0.707106781186547,0.707106781186547));
#34550=DIRECTION('center_axis',(0.,-0.707106781186548,-0.707106781186548));
#34551=DIRECTION('ref_axis',(0.,-0.707106781186548,0.707106781186548));
#34552=DIRECTION('',(0.,-0.707106781186547,0.707106781186547));
#34553=DIRECTION('',(1.,0.,0.));
#34554=DIRECTION('center_axis',(0.855183382509445,0.366511515698828,0.366511515698828));
#34555=DIRECTION('ref_axis',(1.39157273869269E-18,0.707106781186548,-0.707106781186548));
#34556=DIRECTION('',(0.,-0.707106781186548,0.707106781186548));
#34557=DIRECTION('center_axis',(0.855183382509445,0.366511515698828,0.366511515698828));
#34558=DIRECTION('ref_axis',(0.518325556267202,-0.604705968930478,-0.604705968930478));
#34559=DIRECTION('center_axis',(0.,0.707106781186548,0.707106781186548));
#34560=DIRECTION('ref_axis',(1.,0.,0.));
#34561=DIRECTION('',(0.,-0.707106781186547,0.707106781186547));
#34562=DIRECTION('',(-1.,0.,0.));
#34563=DIRECTION('',(0.,-0.707106781186547,0.707106781186547));
#34564=DIRECTION('center_axis',(-0.829037572548639,0.395409094042272,0.395409094042272));
#34565=DIRECTION('ref_axis',(0.430491988667656,7.53182077044634E-18,0.902594398217143));
#34566=DIRECTION('',(0.,-0.707106781186547,0.707106781186547));
#34567=DIRECTION('center_axis',(0.82903757254862,-0.395409094041967,-0.395409094042617));
#34568=DIRECTION('ref_axis',(0.0128476572574178,-0.693451556770021,0.7203886979376));
#34569=DIRECTION('center_axis',(1.,0.,0.));
#34570=DIRECTION('ref_axis',(0.,1.,0.));
#34571=DIRECTION('',(0.,-0.707106781186547,0.707106781186547));
#34572=DIRECTION('center_axis',(-1.,0.,0.));
#34573=DIRECTION('ref_axis',(0.,-0.707106781186548,0.707106781186548));
#34574=DIRECTION('center_axis',(0.,0.707106781186548,0.707106781186548));
#34575=DIRECTION('ref_axis',(1.,0.,0.));
#34576=DIRECTION('',(0.,-0.707106781186547,0.707106781186547));
#34577=DIRECTION('',(-1.,0.,0.));
#34578=DIRECTION('center_axis',(-1.,0.,0.));
#34579=DIRECTION('ref_axis',(0.,0.,1.));
#34580=DIRECTION('',(0.,-0.707106781186547,0.707106781186547));
#34581=DIRECTION('center_axis',(1.,0.,0.));
#34582=DIRECTION('ref_axis',(0.,-0.707106781186548,0.707106781186548));
#34583=DIRECTION('center_axis',(0.,-0.707106781186548,-0.707106781186548));
#34584=DIRECTION('ref_axis',(0.,-0.707106781186548,0.707106781186548));
#34585=DIRECTION('',(0.,-0.707106781186547,0.707106781186547));
#34586=DIRECTION('',(1.,0.,0.));
#34587=DIRECTION('center_axis',(1.,0.,0.));
#34588=DIRECTION('ref_axis',(0.,1.,0.));
#34589=DIRECTION('center_axis',(-1.,0.,0.));
#34590=DIRECTION('ref_axis',(0.,-0.707106781186548,0.707106781186548));
#34591=DIRECTION('center_axis',(0.829037572553119,-0.395409094037575,-0.395409094037575));
#34592=DIRECTION('ref_axis',(-9.11250315044804E-18,-0.707106781186548,0.707106781186548));
#34593=DIRECTION('center_axis',(-0.829037572553119,0.395409094037575,0.395409094037575));
#34594=DIRECTION('ref_axis',(-0.559192903473597,-0.586218089410745,-0.586218089410745));
#34595=DIRECTION('center_axis',(1.,0.,0.));
#34596=DIRECTION('ref_axis',(0.,-0.707106781186548,0.707106781186548));
#34597=DIRECTION('center_axis',(1.,0.,0.));
#34598=DIRECTION('ref_axis',(0.,-0.707106781186548,0.707106781186548));
#34599=DIRECTION('center_axis',(-0.500000000001105,0.612372435695761,0.612372435694926));
#34600=DIRECTION('ref_axis',(0.866025403783801,0.353553390633539,0.353553390554571));
#34601=DIRECTION('',(-1.,0.,0.));
#34602=DIRECTION('center_axis',(0.500000000011393,-0.612372435691199,-0.612372435691088));
#34603=DIRECTION('ref_axis',(0.866025403777861,0.353553390281616,0.353553390921043));
#34604=DIRECTION('center_axis',(-0.500000000011371,-0.612372435691481,-0.612372435690824));
#34605=DIRECTION('ref_axis',(0.866025403777874,-0.353553389921635,-0.353553391280993));
#34606=DIRECTION('',(-1.,0.,0.));
#34607=DIRECTION('center_axis',(0.500000000001104,0.612372435695737,0.612372435694951));
#34608=DIRECTION('ref_axis',(0.866025403783801,-0.353553390620861,-0.353553390567248));
#34609=DIRECTION('center_axis',(-0.500000000011394,0.612372435691143,0.612372435691143));
#34610=DIRECTION('ref_axis',(0.774596669232069,-4.54116170797946E-18,0.632455532045206));
#34611=DIRECTION('',(0.,-0.707106781186547,0.707106781186547));
#34612=DIRECTION('',(0.,-0.707106781186547,0.707106781186547));
#34613=DIRECTION('center_axis',(0.500000000011394,0.612372435691143,0.612372435691143));
#34614=DIRECTION('ref_axis',(0.774596669232069,4.54116170797946E-18,-0.632455532045206));
#34615=DIRECTION('',(0.,-0.707106781186547,0.707106781186547));
#34616=DIRECTION('center_axis',(0.,0.707106781186548,0.707106781186548));
#34617=DIRECTION('ref_axis',(1.,0.,0.));
#34618=DIRECTION('',(0.,-0.707106781186547,0.707106781186547));
#34619=DIRECTION('center_axis',(0.500000000001135,-0.612372435695331,-0.612372435695331));
#34620=DIRECTION('ref_axis',(-1.13185083784068E-17,-0.707106781186548,0.707106781186548));
#34621=DIRECTION('',(0.,-0.707106781186547,0.707106781186547));
#34622=DIRECTION('center_axis',(-0.500000000001135,-0.612372435695331,-0.612372435695331));
#34623=DIRECTION('ref_axis',(1.13185083784068E-17,-0.707106781186548,0.707106781186548));
#34624=DIRECTION('',(0.,-0.707106781186547,0.707106781186547));
#34625=DIRECTION('center_axis',(0.,0.707106781186548,0.707106781186548));
#34626=DIRECTION('ref_axis',(1.,0.,0.));
#34627=DIRECTION('center_axis',(0.,-0.707106781186548,-0.707106781186548));
#34628=DIRECTION('ref_axis',(0.,-0.707106781186548,0.707106781186548));
#34629=DIRECTION('',(0.,-0.707106781186547,0.707106781186547));
#34630=DIRECTION('',(1.,0.,0.));
#34631=DIRECTION('',(0.,-0.707106781186547,0.707106781186547));
#34632=DIRECTION('center_axis',(0.500000000001135,0.612372435695331,0.612372435695331));
#34633=DIRECTION('ref_axis',(0.774596669240545,3.67462033374012E-17,-0.632455532034825));
#34634=DIRECTION('',(0.,-0.707106781186547,0.707106781186547));
#34635=DIRECTION('center_axis',(-0.5000000000011,-0.612372435694895,-0.612372435695796));
#34636=DIRECTION('ref_axis',(0.866025403783803,-0.353553390588746,-0.353553390599358));
#34637=DIRECTION('center_axis',(-0.500000000001135,0.612372435695331,0.612372435695331));
#34638=DIRECTION('ref_axis',(0.774596669240545,-3.67462033374012E-17,0.632455532034825));
#34639=DIRECTION('',(0.,-0.707106781186547,0.707106781186547));
#34640=DIRECTION('center_axis',(0.500000000001106,-0.612372435694935,-0.612372435695752));
#34641=DIRECTION('ref_axis',(0.8660254037838,0.353553390608041,0.35355339058007));
#34642=DIRECTION('center_axis',(0.,-0.707106781186548,-0.707106781186548));
#34643=DIRECTION('ref_axis',(0.,-0.707106781186548,0.707106781186548));
#34644=DIRECTION('',(0.,-0.707106781186547,0.707106781186547));
#34645=DIRECTION('',(1.,0.,0.));
#34646=DIRECTION('center_axis',(-0.500000000011394,-0.612372435691143,-0.612372435691143));
#34647=DIRECTION('ref_axis',(6.99246513044329E-19,-0.707106781186548,0.707106781186548));
#34648=DIRECTION('center_axis',(0.500000000011403,0.612372435691209,0.61237243569107));
#34649=DIRECTION('ref_axis',(0.866025403777855,-0.353553390419331,-0.353553390783343));
#34650=DIRECTION('',(0.,-0.707106781186547,0.707106781186547));
#34651=DIRECTION('center_axis',(0.500000000011394,-0.612372435691143,-0.612372435691143));
#34652=DIRECTION('ref_axis',(-6.99246513044329E-19,-0.707106781186548,0.707106781186548));
#34653=DIRECTION('center_axis',(-0.500000000011383,0.612372435690964,0.612372435691331));
#34654=DIRECTION('ref_axis',(0.866025403777866,0.353553390491497,0.35355339071115));
#34655=DIRECTION('center_axis',(1.,0.,0.));
#34656=DIRECTION('ref_axis',(0.,-0.707106781186548,0.707106781186548));
#34657=DIRECTION('center_axis',(-0.946028810160758,-0.229160959094061,-0.229160959094061));
#34658=DIRECTION('ref_axis',(-0.235425987742297,-1.02571817929429E-18,0.971892280191362));
#34659=DIRECTION('',(0.,-0.707106781186547,0.707106781186547));
#34660=DIRECTION('center_axis',(0.946028810160763,0.229160959093891,0.229160959094211));
#34661=DIRECTION('ref_axis',(0.0242942123304843,-0.75526323419992,0.654971173650504));
#34662=DIRECTION('',(0.,-0.707106781186548,0.707106781186548));
#34663=DIRECTION('center_axis',(0.,-0.707106781186548,-0.707106781186548));
#34664=DIRECTION('ref_axis',(0.,-0.707106781186548,0.707106781186548));
#34665=DIRECTION('',(0.,-0.707106781186547,0.707106781186547));
#34666=DIRECTION('',(1.,0.,0.));
#34667=DIRECTION('center_axis',(0.946028810171404,0.229160959072088,0.229160959072088));
#34668=DIRECTION('ref_axis',(7.7304114234421E-18,0.707106781186548,-0.707106781186548));
#34669=DIRECTION('',(0.,-0.707106781186547,0.707106781186547));
#34670=DIRECTION('center_axis',(-0.946028810149188,-0.229160959860184,-0.229160958375702));
#34671=DIRECTION('ref_axis',(0.00521156151953889,-0.717772603447844,0.696258091059797));
#34672=DIRECTION('center_axis',(0.,-0.707106781186548,0.707106781186548));
#34673=DIRECTION('ref_axis',(0.587785252292473,-0.572061402817684,-0.572061402817684));
#34674=DIRECTION('',(0.,-0.707106781186547,0.707106781186547));
#34675=DIRECTION('center_axis',(0.,0.707106781186548,0.707106781186548));
#34676=DIRECTION('ref_axis',(1.,0.,0.));
#34677=DIRECTION('',(0.,-0.707106781186547,0.707106781186547));
#34678=DIRECTION('',(-1.,0.,0.));
#34679=DIRECTION('center_axis',(-1.,0.,0.));
#34680=DIRECTION('ref_axis',(0.,0.,1.));
#34681=DIRECTION('',(0.,-0.707106781186548,0.707106781186548));
#34682=DIRECTION('center_axis',(-1.,0.,0.));
#34683=DIRECTION('ref_axis',(0.,-0.707106781186548,0.707106781186548));
#34684=DIRECTION('',(0.,-0.707106781186547,0.707106781186547));
#34685=DIRECTION('center_axis',(0.,0.707106781186548,0.707106781186548));
#34686=DIRECTION('ref_axis',(1.,0.,0.));
#34687=DIRECTION('',(0.,-0.707106781186548,0.707106781186548));
#34688=DIRECTION('',(1.,0.,0.));
#34689=DIRECTION('center_axis',(-1.,0.,0.));
#34690=DIRECTION('ref_axis',(0.,0.,1.));
#34691=DIRECTION('',(0.,-0.707106781186547,0.707106781186547));
#34692=DIRECTION('center_axis',(1.,0.,0.));
#34693=DIRECTION('ref_axis',(0.,-0.707106781186548,0.707106781186548));
#34694=DIRECTION('center_axis',(0.,-0.707106781186548,-0.707106781186548));
#34695=DIRECTION('ref_axis',(0.,-0.707106781186548,0.707106781186548));
#34696=DIRECTION('',(0.,-0.707106781186547,0.707106781186547));
#34697=DIRECTION('',(1.,0.,0.));
#34698=DIRECTION('center_axis',(1.,0.,0.));
#34699=DIRECTION('ref_axis',(0.,1.,0.));
#34700=DIRECTION('',(0.,-0.707106781186548,0.707106781186548));
#34701=DIRECTION('center_axis',(-1.,0.,0.));
#34702=DIRECTION('ref_axis',(0.,-0.707106781186548,0.707106781186548));
#34703=DIRECTION('center_axis',(0.,-0.707106781186548,-0.707106781186548));
#34704=DIRECTION('ref_axis',(0.,-0.707106781186548,0.707106781186548));
#34705=DIRECTION('',(1.,0.,0.));
#34706=DIRECTION('center_axis',(0.,-0.707106781186548,0.707106781186548));
#34707=DIRECTION('ref_axis',(0.,-0.707106781186547,-0.707106781186547));
#34708=DIRECTION('',(0.,-0.707106781186547,0.707106781186547));
#34709=DIRECTION('center_axis',(0.,-0.707106781186548,-0.707106781186548));
#34710=DIRECTION('ref_axis',(0.,-0.707106781186548,0.707106781186548));
#34711=DIRECTION('',(-1.,0.,0.));
#34712=DIRECTION('center_axis',(1.,0.,0.));
#34713=DIRECTION('ref_axis',(0.,-0.707106781186548,0.707106781186548));
#34714=DIRECTION('axis',(0.,0.,1.));
#34715=DIRECTION('refdir',(1.,0.,0.));
#34716=DIRECTION('center_axis',(0.,0.707106781186548,0.707106781186548));
#34717=DIRECTION('ref_axis',(1.,0.,0.));
#34718=DIRECTION('center_axis',(0.,0.707106781186548,0.707106781186548));
#34719=DIRECTION('ref_axis',(1.,0.,0.));
#34720=DIRECTION('',(0.866025403761799,-0.353553390621002,0.353553390621002));
#34721=DIRECTION('',(0.,-0.707106781186547,0.707106781186547));
#34722=DIRECTION('',(-0.866025403761799,-0.353553390621002,0.353553390621002));
#34723=DIRECTION('',(-0.866025403761799,0.353553390621002,-0.353553390621002));
#34724=DIRECTION('',(0.,0.707106781186547,-0.707106781186547));
#34725=DIRECTION('',(0.866025403761799,0.353553390621002,-0.353553390621002));
#34726=DIRECTION('center_axis',(0.,-0.707106781186548,-0.707106781186548));
#34727=DIRECTION('ref_axis',(0.,-0.707106781186548,0.707106781186548));
#34728=DIRECTION('center_axis',(0.,-0.707106781186548,-0.707106781186548));
#34729=DIRECTION('ref_axis',(1.,0.,0.));
#34730=DIRECTION('center_axis',(0.,0.707106781186548,0.707106781186548));
#34731=DIRECTION('ref_axis',(1.,0.,0.));
#34732=DIRECTION('',(0.,-0.707106781186548,-0.707106781186548));
#34733=DIRECTION('center_axis',(0.,-0.707106781186547,-0.707106781186548));
#34734=DIRECTION('ref_axis',(0.,-0.707106781186548,0.707106781186547));
#34735=DIRECTION('',(0.866025403761798,0.353553390621003,-0.353553390621002));
#34736=DIRECTION('',(0.,0.707106781186548,-0.707106781186547));
#34737=DIRECTION('',(-0.866025403761798,0.353553390621003,-0.353553390621002));
#34738=DIRECTION('',(-0.866025403761798,-0.353553390621003,0.353553390621002));
#34739=DIRECTION('',(0.,-0.707106781186548,0.707106781186547));
#34740=DIRECTION('',(0.866025403761798,-0.353553390621003,0.353553390621002));
#34741=DIRECTION('center_axis',(-0.500000000039214,0.612372435679786,-0.612372435679785));
#34742=DIRECTION('ref_axis',(-0.774596669209083,-2.65897497434893E-17,0.632455532073358));
#34743=DIRECTION('',(0.,0.707106781186547,0.707106781186548));
#34744=DIRECTION('',(0.,0.707106781186547,0.707106781186548));
#34745=DIRECTION('center_axis',(-1.,0.,0.));
#34746=DIRECTION('ref_axis',(0.,0.,1.));
#34747=DIRECTION('',(0.,0.707106781186547,0.707106781186548));
#34748=DIRECTION('center_axis',(-0.500000000039214,-0.612372435679786,0.612372435679785));
#34749=DIRECTION('ref_axis',(-0.774596669209084,0.632455532073357,1.86150232200487E-17));
#34750=DIRECTION('',(0.,0.707106781186547,0.707106781186548));
#34751=DIRECTION('center_axis',(0.500000000039214,-0.612372435679786,0.612372435679785));
#34752=DIRECTION('ref_axis',(-0.774596669209084,-0.632455532073357,-1.86150232200487E-17));
#34753=DIRECTION('',(0.,0.707106781186547,0.707106781186548));
#34754=DIRECTION('center_axis',(1.,0.,0.));
#34755=DIRECTION('ref_axis',(0.,1.,0.));
#34756=DIRECTION('',(0.,0.707106781186547,0.707106781186548));
#34757=DIRECTION('center_axis',(0.500000000039214,0.612372435679786,-0.612372435679785));
#34758=DIRECTION('ref_axis',(-0.774596669209083,2.65897497434893E-17,-0.632455532073358));
#34759=DIRECTION('axis',(0.,0.,1.));
#34760=DIRECTION('refdir',(1.,0.,0.));
#34761=DIRECTION('center_axis',(0.,0.707106781186548,0.707106781186548));
#34762=DIRECTION('ref_axis',(1.,0.,0.));
#34763=DIRECTION('center_axis',(0.,0.707106781186548,0.707106781186548));
#34764=DIRECTION('ref_axis',(-1.,0.,0.));
#34765=DIRECTION('center_axis',(0.,-0.707106781186548,-0.707106781186548));
#34766=DIRECTION('ref_axis',(-1.,0.,0.));
#34767=DIRECTION('center_axis',(0.,0.707106781186548,0.707106781186548));
#34768=DIRECTION('ref_axis',(-1.,0.,0.));
#34769=DIRECTION('',(0.,-0.707106781186547,-0.707106781186547));
#34770=DIRECTION('center_axis',(0.,0.707106781186548,0.707106781186548));
#34771=DIRECTION('ref_axis',(-1.,0.,0.));
#34772=DIRECTION('center_axis',(0.,0.707106781186548,0.707106781186548));
#34773=DIRECTION('ref_axis',(-1.,0.,0.));
#34774=DIRECTION('center_axis',(-7.85046229357589E-17,0.707106781186548,
-0.707106781186548));
#34775=DIRECTION('ref_axis',(1.,0.,-1.11022302464736E-16));
#34776=DIRECTION('center_axis',(0.,0.707106781186548,0.707106781186548));
#34777=DIRECTION('ref_axis',(-1.,0.,0.));
#34778=DIRECTION('center_axis',(-2.27272746077357E-11,-0.707106781186548,
-0.707106781186548));
#34779=DIRECTION('ref_axis',(-4.86851002232982E-28,-0.707106781186548,0.707106781186548));
#34780=DIRECTION('',(0.,0.707106781186547,-0.707106781186547));
#34781=DIRECTION('',(-0.866025403795548,0.353553390593585,-0.35355339056575));
#34782=DIRECTION('',(-0.866025403795548,-0.35355339056575,0.353553390593585));
#34783=DIRECTION('',(0.,-0.707106781186547,0.707106781186547));
#34784=DIRECTION('',(0.866025403795548,-0.353553390593585,0.35355339056575));
#34785=DIRECTION('',(0.866025403795548,0.35355339056575,-0.353553390593585));
#34786=DIRECTION('center_axis',(0.,0.707106781186547,0.707106781186548));
#34787=DIRECTION('ref_axis',(1.,0.,0.));
#34788=DIRECTION('',(0.,-0.707106781186548,0.707106781186547));
#34789=DIRECTION('',(-0.866025403795548,-0.353553390579667,0.353553390579667));
#34790=DIRECTION('',(-0.866025403795548,0.353553390579667,-0.353553390579667));
#34791=DIRECTION('',(0.,0.707106781186548,-0.707106781186547));
#34792=DIRECTION('',(0.866025403795548,0.353553390579667,-0.353553390579667));
#34793=DIRECTION('',(0.866025403795548,-0.353553390579667,0.353553390579667));
#34794=DIRECTION('center_axis',(0.499999999980758,0.61237243570365,-0.61237243570365));
#34795=DIRECTION('ref_axis',(-0.774596669257382,1.17004406563443E-17,-0.632455532014204));
#34796=DIRECTION('',(0.,0.707106781186547,0.707106781186548));
#34797=DIRECTION('',(0.,0.707106781186547,0.707106781186548));
#34798=DIRECTION('center_axis',(-0.499999999980758,0.61237243570365,-0.61237243570365));
#34799=DIRECTION('ref_axis',(-0.774596669257382,-1.17004406563443E-17,0.632455532014204));
#34800=DIRECTION('',(0.,0.707106781186547,0.707106781186548));
#34801=DIRECTION('center_axis',(-1.,0.,0.));
#34802=DIRECTION('ref_axis',(0.,0.,1.));
#34803=DIRECTION('',(0.,0.707106781186547,0.707106781186548));
#34804=DIRECTION('center_axis',(-0.499999999980758,-0.61237243570365,0.61237243570365));
#34805=DIRECTION('ref_axis',(-0.774596669257382,0.632455532014204,-1.19590756914335E-17));
#34806=DIRECTION('',(0.,0.707106781186547,0.707106781186548));
#34807=DIRECTION('center_axis',(0.499999999980758,-0.61237243570365,0.61237243570365));
#34808=DIRECTION('ref_axis',(-0.774596669257382,-0.632455532014204,1.19590756914335E-17));
#34809=DIRECTION('',(0.,0.707106781186547,0.707106781186548));
#34810=DIRECTION('center_axis',(1.,0.,0.));
#34811=DIRECTION('ref_axis',(0.,1.,0.));
#34812=DIRECTION('center_axis',(0.,0.707106781186548,0.707106781186548));
#34813=DIRECTION('ref_axis',(1.,0.,0.));
#34814=DIRECTION('center_axis',(0.,0.707106781186548,0.707106781186548));
#34815=DIRECTION('ref_axis',(-1.,0.,0.));
#34816=DIRECTION('center_axis',(0.,-0.707106781186548,-0.707106781186548));
#34817=DIRECTION('ref_axis',(-1.,0.,0.));
#34818=DIRECTION('center_axis',(0.,0.707106781186548,0.707106781186548));
#34819=DIRECTION('ref_axis',(-1.,0.,0.));
#34820=DIRECTION('',(-0.707106781186547,0.5,0.5));
#34821=DIRECTION('center_axis',(0.,0.707106781186548,0.707106781186548));
#34822=DIRECTION('ref_axis',(-1.,0.,0.));
#34823=DIRECTION('',(0.,-0.707106781186548,-0.707106781186548));
#34824=DIRECTION('axis',(0.,0.,1.));
#34825=DIRECTION('refdir',(1.,0.,0.));
#34826=DIRECTION('center_axis',(0.,-0.707106781186548,-0.707106781186548));
#34827=DIRECTION('ref_axis',(0.,-0.707106781186548,0.707106781186548));
#34828=DIRECTION('center_axis',(0.,-0.707106781186548,-0.707106781186548));
#34829=DIRECTION('ref_axis',(-1.,0.,0.));
#34830=DIRECTION('center_axis',(0.,0.707106781186548,0.707106781186548));
#34831=DIRECTION('ref_axis',(-1.,0.,0.));
#34832=DIRECTION('center_axis',(0.,-0.707106781186548,-0.707106781186548));
#34833=DIRECTION('ref_axis',(-1.,0.,0.));
#34834=DIRECTION('',(0.,0.707106781186547,0.707106781186547));
#34835=DIRECTION('center_axis',(0.,-0.707106781186548,-0.707106781186548));
#34836=DIRECTION('ref_axis',(-1.,0.,0.));
#34837=DIRECTION('center_axis',(0.,-0.707106781186548,-0.707106781186548));
#34838=DIRECTION('ref_axis',(-1.,0.,0.));
#34839=DIRECTION('center_axis',(-7.85046229357589E-17,-0.707106781186548,
0.707106781186548));
#34840=DIRECTION('ref_axis',(1.,0.,1.11022302464736E-16));
#34841=DIRECTION('center_axis',(0.,-0.707106781186548,-0.707106781186548));
#34842=DIRECTION('ref_axis',(-1.,0.,0.));
#34843=DIRECTION('center_axis',(-2.27272746077357E-11,0.707106781186548,
0.707106781186548));
#34844=DIRECTION('ref_axis',(1.,-1.16819139994433E-27,3.21412199860375E-11));
#34845=DIRECTION('',(0.,-0.707106781186547,0.707106781186547));
#34846=DIRECTION('',(-0.866025403795548,-0.353553390593585,0.35355339056575));
#34847=DIRECTION('',(-0.866025403795548,0.35355339056575,-0.353553390593585));
#34848=DIRECTION('',(0.,0.707106781186547,-0.707106781186547));
#34849=DIRECTION('',(0.866025403795548,0.353553390593585,-0.35355339056575));
#34850=DIRECTION('',(0.866025403795548,-0.35355339056575,0.353553390593585));
#34851=DIRECTION('center_axis',(0.,-0.707106781186547,-0.707106781186548));
#34852=DIRECTION('ref_axis',(0.,-0.707106781186548,0.707106781186547));
#34853=DIRECTION('',(0.,0.707106781186548,-0.707106781186547));
#34854=DIRECTION('',(-0.866025403795548,0.353553390579667,-0.353553390579667));
#34855=DIRECTION('',(-0.866025403795548,-0.353553390579667,0.353553390579667));
#34856=DIRECTION('',(0.,-0.707106781186548,0.707106781186547));
#34857=DIRECTION('',(0.866025403795548,-0.353553390579667,0.353553390579667));
#34858=DIRECTION('',(0.866025403795548,0.353553390579667,-0.353553390579667));
#34859=DIRECTION('center_axis',(0.499999999980758,-0.61237243570365,0.61237243570365));
#34860=DIRECTION('ref_axis',(-0.774596669257382,-0.632455532014204,1.19590756914335E-17));
#34861=DIRECTION('',(0.,-0.707106781186547,-0.707106781186548));
#34862=DIRECTION('',(0.,-0.707106781186547,-0.707106781186548));
#34863=DIRECTION('center_axis',(-0.499999999980758,-0.61237243570365,0.61237243570365));
#34864=DIRECTION('ref_axis',(-0.774596669257382,0.632455532014204,-1.19590756914335E-17));
#34865=DIRECTION('',(0.,-0.707106781186547,-0.707106781186548));
#34866=DIRECTION('center_axis',(-1.,0.,0.));
#34867=DIRECTION('ref_axis',(0.,0.,1.));
#34868=DIRECTION('',(0.,-0.707106781186547,-0.707106781186548));
#34869=DIRECTION('center_axis',(-0.499999999980758,0.61237243570365,-0.61237243570365));
#34870=DIRECTION('ref_axis',(-0.774596669257382,-1.17004406563443E-17,0.632455532014204));
#34871=DIRECTION('',(0.,-0.707106781186547,-0.707106781186548));
#34872=DIRECTION('center_axis',(0.499999999980758,0.61237243570365,-0.61237243570365));
#34873=DIRECTION('ref_axis',(-0.774596669257382,1.17004406563443E-17,-0.632455532014204));
#34874=DIRECTION('',(0.,-0.707106781186547,-0.707106781186548));
#34875=DIRECTION('center_axis',(1.,0.,0.));
#34876=DIRECTION('ref_axis',(0.,1.,0.));
#34877=DIRECTION('center_axis',(0.,-0.707106781186548,-0.707106781186548));
#34878=DIRECTION('ref_axis',(0.,-0.707106781186548,0.707106781186548));
#34879=DIRECTION('center_axis',(0.,-0.707106781186548,-0.707106781186548));
#34880=DIRECTION('ref_axis',(-1.,0.,0.));
#34881=DIRECTION('center_axis',(0.,0.707106781186548,0.707106781186548));
#34882=DIRECTION('ref_axis',(-1.,0.,0.));
#34883=DIRECTION('center_axis',(0.,-0.707106781186548,-0.707106781186548));
#34884=DIRECTION('ref_axis',(-1.,0.,0.));
#34885=DIRECTION('',(-0.707106781186547,-0.5,-0.5));
#34886=DIRECTION('center_axis',(0.,-0.707106781186548,-0.707106781186548));
#34887=DIRECTION('ref_axis',(-1.,0.,0.));
#34888=DIRECTION('',(0.,0.707106781186548,0.707106781186548));
#34889=DIRECTION('axis',(0.,0.,1.));
#34890=DIRECTION('refdir',(1.,0.,0.));
#34891=DIRECTION('center_axis',(-1.,0.,0.));
#34892=DIRECTION('ref_axis',(0.,0.,1.));
#34893=DIRECTION('',(0.,0.707106781186548,-0.707106781186548));
#34894=DIRECTION('center_axis',(-1.,0.,0.));
#34895=DIRECTION('ref_axis',(0.,0.,1.));
#34896=DIRECTION('',(0.,0.707106781186547,-0.707106781186547));
#34897=DIRECTION('center_axis',(1.,0.,0.));
#34898=DIRECTION('ref_axis',(0.,0.,1.));
#34899=DIRECTION('center_axis',(1.,0.,0.));
#34900=DIRECTION('ref_axis',(0.,-0.707106781186548,-0.707106781186547));
#34901=DIRECTION('center_axis',(-1.,0.,0.));
#34902=DIRECTION('ref_axis',(0.,0.,1.));
#34903=DIRECTION('',(-0.707104308763577,0.500001748260936,-0.500001748260935));
#34904=DIRECTION('',(0.707104308763577,0.500001748260935,-0.500001748260936));
#34905=DIRECTION('center_axis',(1.,0.,0.));
#34906=DIRECTION('ref_axis',(0.,1.,0.));
#34907=DIRECTION('center_axis',(-1.,0.,0.));
#34908=DIRECTION('ref_axis',(0.,-0.707106781186547,-0.707106781186548));
#34909=DIRECTION('center_axis',(-1.,0.,0.));
#34910=DIRECTION('ref_axis',(0.,0.,1.));
#34911=DIRECTION('center_axis',(-1.,0.,0.));
#34912=DIRECTION('ref_axis',(0.,0.707106781186548,-0.707106781186547));
#34913=DIRECTION('center_axis',(-1.,0.,0.));
#34914=DIRECTION('ref_axis',(0.,0.,-1.));
#34915=DIRECTION('center_axis',(1.,0.,0.));
#34916=DIRECTION('ref_axis',(0.,1.,0.));
#34917=DIRECTION('center_axis',(-1.,0.,0.));
#34918=DIRECTION('ref_axis',(0.,0.707106781186548,-0.707106781186547));
#34919=DIRECTION('center_axis',(-1.,0.,0.));
#34920=DIRECTION('ref_axis',(0.,0.,1.));
#34921=DIRECTION('center_axis',(-1.,0.,0.));
#34922=DIRECTION('ref_axis',(0.,0.707106781186547,0.707106781186548));
#34923=DIRECTION('center_axis',(-1.,0.,0.));
#34924=DIRECTION('ref_axis',(0.,0.,-1.));
#34925=DIRECTION('center_axis',(1.,0.,0.));
#34926=DIRECTION('ref_axis',(0.,0.,-1.));
#34927=DIRECTION('center_axis',(-1.,0.,0.));
#34928=DIRECTION('ref_axis',(0.,0.,-1.));
#34929=DIRECTION('',(1.,0.,0.));
#34930=DIRECTION('',(-1.,0.,0.));
#34931=DIRECTION('center_axis',(1.,0.,0.));
#34932=DIRECTION('ref_axis',(0.,0.,-1.));
#34933=DIRECTION('',(1.,0.,0.));
#34934=DIRECTION('',(-1.,0.,0.));
#34935=DIRECTION('center_axis',(-1.,0.,0.));
#34936=DIRECTION('ref_axis',(0.,0.,-1.));
#34937=DIRECTION('center_axis',(1.,0.,0.));
#34938=DIRECTION('ref_axis',(0.,-0.870991239054279,-0.491298546192324));
#34939=DIRECTION('',(1.,0.,0.));
#34940=DIRECTION('center_axis',(-1.,0.,0.));
#34941=DIRECTION('ref_axis',(0.,0.707106781186547,0.707106781186548));
#34942=DIRECTION('center_axis',(1.,0.,0.));
#34943=DIRECTION('ref_axis',(0.,-0.491298546192324,0.870991239054279));
#34944=DIRECTION('',(1.,0.,0.));
#34945=DIRECTION('center_axis',(-1.,0.,0.));
#34946=DIRECTION('ref_axis',(0.,0.707106781186548,-0.707106781186547));
#34947=DIRECTION('center_axis',(1.,0.,0.));
#34948=DIRECTION('ref_axis',(0.,0.707106781186548,-0.707106781186547));
#34949=DIRECTION('center_axis',(-1.,0.,0.));
#34950=DIRECTION('ref_axis',(0.,0.707106781186548,-0.707106781186547));
#34951=DIRECTION('',(-1.,0.,0.));
#34952=DIRECTION('center_axis',(1.,0.,0.));
#34953=DIRECTION('ref_axis',(0.,-0.707106781186547,-0.707106781186548));
#34954=DIRECTION('center_axis',(-1.,0.,0.));
#34955=DIRECTION('ref_axis',(0.,-0.707106781186547,-0.707106781186548));
#34956=DIRECTION('',(-1.,0.,0.));
#34957=DIRECTION('center_axis',(-1.,0.,0.));
#34958=DIRECTION('ref_axis',(0.,-0.707106781186547,-0.707106781186548));
#34959=DIRECTION('center_axis',(-1.,0.,0.));
#34960=DIRECTION('ref_axis',(0.,0.,1.));
#34961=DIRECTION('center_axis',(-1.,0.,0.));
#34962=DIRECTION('ref_axis',(0.,0.,1.));
#34963=DIRECTION('',(-1.,0.,0.));
#34964=DIRECTION('',(1.,0.,0.));
#34965=DIRECTION('center_axis',(-1.,0.,0.));
#34966=DIRECTION('ref_axis',(0.,0.,1.));
#34967=DIRECTION('',(1.,0.,0.));
#34968=DIRECTION('center_axis',(-1.,0.,0.));
#34969=DIRECTION('ref_axis',(0.,-0.707106781186547,-0.707106781186548));
#34970=DIRECTION('',(1.,0.,0.));
#34971=DIRECTION('center_axis',(-1.,0.,0.));
#34972=DIRECTION('ref_axis',(0.,0.,1.));
#34973=DIRECTION('',(-1.,0.,0.));
#34974=DIRECTION('center_axis',(-1.,0.,0.));
#34975=DIRECTION('ref_axis',(0.,0.,1.));
#34976=DIRECTION('',(0.,-0.707106781186547,0.707106781186547));
#34977=DIRECTION('',(0.,-0.707106781186547,0.707106781186547));
#34978=DIRECTION('center_axis',(0.,0.707106781186549,0.707106781186546));
#34979=DIRECTION('ref_axis',(-1.,0.,0.));
#34980=DIRECTION('',(0.,0.707106781186549,0.707106781186546));
#34981=DIRECTION('center_axis',(0.,0.707106781186548,0.707106781186548));
#34982=DIRECTION('ref_axis',(-1.,0.,0.));
#34983=DIRECTION('center_axis',(0.,0.707106781186549,0.707106781186546));
#34984=DIRECTION('ref_axis',(1.,0.,0.));
#34985=DIRECTION('center_axis',(0.,-0.707106781186549,-0.707106781186546));
#34986=DIRECTION('ref_axis',(-1.,0.,0.));
#34987=DIRECTION('center_axis',(0.,-0.707106781186549,-0.707106781186546));
#34988=DIRECTION('ref_axis',(-1.,0.,0.));
#34989=DIRECTION('center_axis',(0.,-0.707106781186549,-0.707106781186546));
#34990=DIRECTION('ref_axis',(-1.,0.,0.));
#34991=DIRECTION('center_axis',(0.,-0.707106781186549,-0.707106781186546));
#34992=DIRECTION('ref_axis',(-1.,0.,0.));
#34993=DIRECTION('',(0.,-0.707106781186549,-0.707106781186546));
#34994=DIRECTION('center_axis',(0.,0.707106781186549,0.707106781186546));
#34995=DIRECTION('ref_axis',(1.,0.,0.));
#34996=DIRECTION('center_axis',(0.,-0.707106781186549,-0.707106781186546));
#34997=DIRECTION('ref_axis',(-1.,0.,0.));
#34998=DIRECTION('center_axis',(0.,-0.707106781186549,-0.707106781186546));
#34999=DIRECTION('ref_axis',(-1.,0.,0.));
#35000=DIRECTION('center_axis',(0.,0.707106781186548,0.707106781186548));
#35001=DIRECTION('ref_axis',(-1.,0.,0.));
#35002=DIRECTION('',(0.,-0.707106781186549,-0.707106781186546));
#35003=DIRECTION('center_axis',(0.,0.707106781186548,0.707106781186548));
#35004=DIRECTION('ref_axis',(1.,0.,0.));
#35005=DIRECTION('center_axis',(0.,0.707106781186548,0.707106781186548));
#35006=DIRECTION('ref_axis',(1.,0.,0.));
#35007=DIRECTION('center_axis',(0.,-0.707106781186549,-0.707106781186546));
#35008=DIRECTION('ref_axis',(-5.0532154980743E-16,0.707106781186546,-0.707106781186549));
#35009=DIRECTION('center_axis',(0.,0.707106781186549,0.707106781186546));
#35010=DIRECTION('ref_axis',(-5.0532154980743E-16,-0.707106781186546,0.707106781186549));
#35011=DIRECTION('center_axis',(0.,0.707106781186549,0.707106781186546));
#35012=DIRECTION('ref_axis',(-1.,0.,0.));
#35013=DIRECTION('center_axis',(0.,-0.707106781186548,-0.707106781186548));
#35014=DIRECTION('ref_axis',(0.,-0.707106781186548,0.707106781186548));
#35015=DIRECTION('',(0.707104308763575,-0.500001748260937,0.500001748260937));
#35016=DIRECTION('',(0.,-0.707106781186547,0.707106781186547));
#35017=DIRECTION('',(-1.,0.,0.));
#35018=DIRECTION('',(0.,0.707106781186547,-0.707106781186547));
#35019=DIRECTION('',(1.,0.,0.));
#35020=DIRECTION('center_axis',(0.,-0.707106781186548,-0.707106781186548));
#35021=DIRECTION('ref_axis',(-1.,0.,0.));
#35022=DIRECTION('center_axis',(0.,-0.707106781186549,-0.707106781186546));
#35023=DIRECTION('ref_axis',(-1.,0.,0.));
#35024=DIRECTION('',(0.,-0.707106781186549,-0.707106781186546));
#35025=DIRECTION('center_axis',(0.,0.707106781186549,0.707106781186546));
#35026=DIRECTION('ref_axis',(-1.,0.,0.));
#35027=DIRECTION('center_axis',(0.,-0.707106781186548,-0.707106781186548));
#35028=DIRECTION('ref_axis',(-1.,0.,0.));
#35029=DIRECTION('',(0.,0.707106781186549,0.707106781186546));
#35030=DIRECTION('center_axis',(0.,0.707106781186549,0.707106781186546));
#35031=DIRECTION('ref_axis',(-1.,0.,0.));
#35032=DIRECTION('center_axis',(0.,-0.707106781186549,-0.707106781186546));
#35033=DIRECTION('ref_axis',(0.,0.707106781186546,-0.707106781186549));
#35034=DIRECTION('center_axis',(0.,0.707106781186549,0.707106781186546));
#35035=DIRECTION('ref_axis',(-1.,0.,0.));
#35036=DIRECTION('center_axis',(0.,0.707106781186549,0.707106781186546));
#35037=DIRECTION('ref_axis',(-1.,0.,0.));
#35038=DIRECTION('',(0.,0.707106781186549,0.707106781186546));
#35039=DIRECTION('center_axis',(0.,0.707106781186549,0.707106781186546));
#35040=DIRECTION('ref_axis',(-1.,0.,0.));
#35041=DIRECTION('center_axis',(0.,-0.707106781186549,-0.707106781186546));
#35042=DIRECTION('ref_axis',(0.,0.707106781186546,-0.707106781186549));
#35043=DIRECTION('',(1.,0.,0.));
#35044=DIRECTION('center_axis',(0.,-0.707106781186548,-0.707106781186548));
#35045=DIRECTION('ref_axis',(0.,-0.707106781186548,0.707106781186548));
#35046=DIRECTION('',(-0.707104308763575,-0.500001748260937,0.500001748260937));
#35047=DIRECTION('',(-1.,0.,0.));
#35048=DIRECTION('',(0.,0.707106781186547,-0.707106781186547));
#35049=DIRECTION('',(1.,0.,0.));
#35050=DIRECTION('',(0.,-0.707106781186547,0.707106781186547));
#35051=DIRECTION('center_axis',(-1.,0.,0.));
#35052=DIRECTION('ref_axis',(0.,0.,1.));
#35053=DIRECTION('center_axis',(1.,0.,0.));
#35054=DIRECTION('ref_axis',(0.,0.,1.));
#35055=DIRECTION('',(0.,0.707106781186547,0.707106781186547));
#35056=DIRECTION('',(0.,-0.707106781186547,0.707106781186547));
#35057=DIRECTION('',(0.,-0.707106781186547,-0.707106781186547));
#35058=DIRECTION('center_axis',(1.,0.,0.));
#35059=DIRECTION('ref_axis',(0.,0.,1.));
#35060=DIRECTION('center_axis',(-1.,0.,0.));
#35061=DIRECTION('ref_axis',(0.,0.,1.));
#35062=DIRECTION('center_axis',(1.,0.,0.));
#35063=DIRECTION('ref_axis',(0.,0.,1.));
#35064=DIRECTION('center_axis',(-1.,0.,0.));
#35065=DIRECTION('ref_axis',(0.,0.,1.));
#35066=DIRECTION('center_axis',(-1.,0.,0.));
#35067=DIRECTION('ref_axis',(0.,0.,1.));
#35068=DIRECTION('center_axis',(-1.,0.,0.));
#35069=DIRECTION('ref_axis',(0.,0.,1.));
#35070=DIRECTION('center_axis',(-1.,0.,0.));
#35071=DIRECTION('ref_axis',(0.,0.707106781186547,0.707106781186548));
#35072=DIRECTION('center_axis',(-1.,0.,0.));
#35073=DIRECTION('ref_axis',(0.,0.,-1.));
#35074=DIRECTION('center_axis',(-1.,0.,0.));
#35075=DIRECTION('ref_axis',(0.,-0.707106781186548,0.707106781186547));
#35076=DIRECTION('center_axis',(-1.,0.,0.));
#35077=DIRECTION('ref_axis',(0.,0.,1.));
#35078=DIRECTION('center_axis',(-1.,0.,0.));
#35079=DIRECTION('ref_axis',(0.,-0.707106781186548,0.707106781186547));
#35080=DIRECTION('center_axis',(-1.,0.,0.));
#35081=DIRECTION('ref_axis',(0.,0.,-1.));
#35082=DIRECTION('center_axis',(-1.,0.,0.));
#35083=DIRECTION('ref_axis',(0.,-0.707106781186547,-0.707106781186548));
#35084=DIRECTION('center_axis',(-1.,0.,0.));
#35085=DIRECTION('ref_axis',(0.,0.,1.));
#35086=DIRECTION('center_axis',(-1.,0.,0.));
#35087=DIRECTION('ref_axis',(0.,0.,1.));
#35088=DIRECTION('',(0.,0.707106781186547,0.707106781186547));
#35089=DIRECTION('',(0.,0.707106781186547,-0.707106781186547));
#35090=DIRECTION('',(0.,-0.707106781186547,-0.707106781186547));
#35091=DIRECTION('center_axis',(-1.,0.,0.));
#35092=DIRECTION('ref_axis',(0.,0.,1.));
#35093=DIRECTION('center_axis',(-1.,0.,0.));
#35094=DIRECTION('ref_axis',(0.,0.,1.));
#35095=DIRECTION('',(-1.,0.,0.));
#35096=DIRECTION('center_axis',(-1.,0.,0.));
#35097=DIRECTION('ref_axis',(0.,0.,1.));
#35098=DIRECTION('',(1.,0.,0.));
#35099=DIRECTION('center_axis',(-1.,0.,0.));
#35100=DIRECTION('ref_axis',(0.,0.,1.));
#35101=DIRECTION('',(-1.,0.,0.));
#35102=DIRECTION('',(1.,0.,0.));
#35103=DIRECTION('center_axis',(-1.,0.,0.));
#35104=DIRECTION('ref_axis',(0.,0.,1.));
#35105=DIRECTION('center_axis',(0.,0.707106781186548,0.707106781186548));
#35106=DIRECTION('ref_axis',(1.,0.,0.));
#35107=DIRECTION('center_axis',(0.,-0.707106781186548,-0.707106781186548));
#35108=DIRECTION('ref_axis',(1.,0.,0.));
#35109=DIRECTION('',(0.,0.707106781186548,0.707106781186548));
#35110=DIRECTION('center_axis',(0.,-0.707106781186548,0.707106781186548));
#35111=DIRECTION('ref_axis',(-1.,0.,0.));
#35112=DIRECTION('',(-1.,0.,0.));
#35113=DIRECTION('center_axis',(0.,0.707106781186548,-0.707106781186548));
#35114=DIRECTION('ref_axis',(-1.,0.,0.));
#35115=DIRECTION('',(1.,0.,0.));
#35116=DIRECTION('center_axis',(0.,0.707106781186548,0.707106781186548));
#35117=DIRECTION('ref_axis',(1.,0.,0.));
#35118=DIRECTION('center_axis',(1.,0.,0.));
#35119=DIRECTION('ref_axis',(0.,0.870991239054279,0.491298546192324));
#35120=DIRECTION('center_axis',(-1.,0.,0.));
#35121=DIRECTION('ref_axis',(0.,-0.707106781186547,-0.707106781186548));
#35122=DIRECTION('',(1.,0.,0.));
#35123=DIRECTION('',(-1.,0.,0.));
#35124=DIRECTION('center_axis',(1.,0.,0.));
#35125=DIRECTION('ref_axis',(0.,0.491298546192324,-0.870991239054279));
#35126=DIRECTION('center_axis',(-1.,0.,0.));
#35127=DIRECTION('ref_axis',(0.,-0.707106781186548,0.707106781186547));
#35128=DIRECTION('',(1.,0.,0.));
#35129=DIRECTION('',(-1.,0.,0.));
#35130=DIRECTION('center_axis',(1.,0.,0.));
#35131=DIRECTION('ref_axis',(0.,0.707106781186547,0.707106781186548));
#35132=DIRECTION('',(-1.,0.,0.));
#35133=DIRECTION('center_axis',(-1.,0.,0.));
#35134=DIRECTION('ref_axis',(0.,0.707106781186547,0.707106781186548));
#35135=DIRECTION('',(1.,0.,0.));
#35136=DIRECTION('center_axis',(1.,0.,0.));
#35137=DIRECTION('ref_axis',(0.,1.22464679914735E-16,1.));
#35138=DIRECTION('center_axis',(-1.,0.,0.));
#35139=DIRECTION('ref_axis',(0.,0.,-1.));
#35140=DIRECTION('',(1.,0.,0.));
#35141=DIRECTION('center_axis',(1.,0.,0.));
#35142=DIRECTION('ref_axis',(0.,0.,-1.));
#35143=DIRECTION('center_axis',(-1.,0.,0.));
#35144=DIRECTION('ref_axis',(0.,0.,-1.));
#35145=DIRECTION('center_axis',(1.,0.,0.));
#35146=DIRECTION('ref_axis',(0.,-0.707106781186548,0.707106781186547));
#35147=DIRECTION('',(-1.,0.,0.));
#35148=DIRECTION('center_axis',(-1.,0.,0.));
#35149=DIRECTION('ref_axis',(0.,-0.707106781186548,0.707106781186547));
#35150=DIRECTION('center_axis',(1.,0.,0.));
#35151=DIRECTION('ref_axis',(0.,1.,0.));
#35152=DIRECTION('center_axis',(-1.,0.,0.));
#35153=DIRECTION('ref_axis',(0.,0.,1.));
#35154=DIRECTION('center_axis',(1.,0.,0.));
#35155=DIRECTION('ref_axis',(0.,1.,0.));
#35156=DIRECTION('center_axis',(-1.,0.,0.));
#35157=DIRECTION('ref_axis',(0.,0.,1.));
#35158=DIRECTION('center_axis',(-1.,0.,0.));
#35159=DIRECTION('ref_axis',(0.,0.,1.));
#35160=DIRECTION('center_axis',(-0.946028810149193,-0.324082536351007,-1.06892949644448E-9));
#35161=DIRECTION('ref_axis',(-0.0238519321544925,0.069626133465603,0.997287965871005));
#35162=DIRECTION('',(1.,0.,0.));
#35163=DIRECTION('center_axis',(0.946028810160761,0.324082536317239,-1.73103110021756E-13));
#35164=DIRECTION('ref_axis',(-0.00756181520538782,0.0220736825960291,0.999727748683335));
#35165=DIRECTION('',(1.,0.,0.));
#35166=DIRECTION('center_axis',(-1.,0.,0.));
#35167=DIRECTION('ref_axis',(0.,0.,1.));
#35168=DIRECTION('',(1.,0.,0.));
#35169=DIRECTION('center_axis',(1.,0.,0.));
#35170=DIRECTION('ref_axis',(0.,0.,1.));
#35171=DIRECTION('',(-1.,0.,0.));
#35172=DIRECTION('center_axis',(-1.,0.,0.));
#35173=DIRECTION('ref_axis',(0.,0.,1.));
#35174=DIRECTION('',(1.,0.,0.));
#35175=DIRECTION('center_axis',(1.,0.,0.));
#35176=DIRECTION('ref_axis',(0.,0.,1.));
#35177=DIRECTION('',(1.,0.,0.));
#35178=DIRECTION('center_axis',(1.,0.,0.));
#35179=DIRECTION('ref_axis',(0.,0.,1.));
#35180=DIRECTION('',(-1.,0.,0.));
#35181=DIRECTION('center_axis',(-1.,0.,0.));
#35182=DIRECTION('ref_axis',(0.,0.,1.));
#35183=DIRECTION('',(1.,0.,0.));
#35184=DIRECTION('',(-1.,0.,0.));
#35185=DIRECTION('center_axis',(-0.500000000011387,-0.866025403777865,-1.13502270606945E-13));
#35186=DIRECTION('ref_axis',(0.866025403777865,-0.500000000011387,-1.2232312709768E-10));
#35187=DIRECTION('center_axis',(0.500000000011405,-0.866025403777854,2.15654314153191E-13));
#35188=DIRECTION('ref_axis',(0.866025403777854,0.500000000011405,7.56457705137375E-10));
#35189=DIRECTION('',(-1.,0.,0.));
#35190=DIRECTION('center_axis',(-0.500000000001134,0.866025403783784,1.17302365318434E-14));
#35191=DIRECTION('ref_axis',(0.866025403783784,0.500000000001134,-3.36774821015014E-10));
#35192=DIRECTION('center_axis',(0.500000000001136,0.866025403783783,-1.95503942197372E-14));
#35193=DIRECTION('ref_axis',(0.866025403783783,-0.500000000001136,1.13706776558401E-10));
#35194=DIRECTION('center_axis',(0.855183382509445,0.518325556267202,0.));
#35195=DIRECTION('ref_axis',(-0.518325556267202,0.855183382509445,0.));
#35196=DIRECTION('',(1.,0.,0.));
#35197=DIRECTION('center_axis',(0.855183382508505,0.518325556268753,-1.92327333756619E-13));
#35198=DIRECTION('ref_axis',(-0.00559375624087415,0.00922911734785472,0.999941764946388));
#35199=DIRECTION('center_axis',(-1.,0.,0.));
#35200=DIRECTION('ref_axis',(0.,0.,1.));
#35201=DIRECTION('',(1.,0.,0.));
#35202=DIRECTION('center_axis',(1.,0.,0.));
#35203=DIRECTION('ref_axis',(0.,0.,1.));
#35204=DIRECTION('',(-1.,0.,0.));
#35205=DIRECTION('center_axis',(-1.,0.,0.));
#35206=DIRECTION('ref_axis',(0.,0.,1.));
#35207=DIRECTION('center_axis',(0.829037572548643,-0.559192903480234,-1.64064661511221E-13));
#35208=DIRECTION('ref_axis',(-0.0360858435021883,-0.0534994630911657,0.997915637390102));
#35209=DIRECTION('',(-1.,0.,0.));
#35210=DIRECTION('center_axis',(-0.82903757255312,0.559192903473596,0.));
#35211=DIRECTION('ref_axis',(0.559192903473596,0.82903757255312,0.));
#35212=DIRECTION('center_axis',(-0.500000000011404,0.866025403777855,1.81603632971102E-13));
#35213=DIRECTION('ref_axis',(0.866025403777855,0.500000000011404,-1.23583351950854E-10));
#35214=DIRECTION('',(1.,0.,0.));
#35215=DIRECTION('center_axis',(0.500000000001135,-0.866025403783783,-7.82015768789461E-15));
#35216=DIRECTION('ref_axis',(0.866025403783783,0.500000000001135,1.8743640553155E-10));
#35217=DIRECTION('center_axis',(-0.500000000001136,-0.866025403783783,-1.56403153757889E-14));
#35218=DIRECTION('ref_axis',(0.866025403783783,-0.500000000001136,-1.67428462619296E-10));
#35219=DIRECTION('',(1.,0.,0.));
#35220=DIRECTION('center_axis',(0.500000000011388,0.866025403777864,-9.08018164855533E-14));
#35221=DIRECTION('ref_axis',(0.866025403777864,-0.500000000011388,8.55286471205808E-10));
#35222=DIRECTION('center_axis',(-1.,0.,0.));
#35223=DIRECTION('ref_axis',(0.,0.,1.));
#35224=DIRECTION('center_axis',(1.,0.,0.));
#35225=DIRECTION('ref_axis',(0.,0.,1.));
#35226=DIRECTION('',(-1.,0.,0.));
#35227=DIRECTION('center_axis',(1.,0.,0.));
#35228=DIRECTION('ref_axis',(0.,0.,1.));
#35229=DIRECTION('',(1.,0.,0.));
#35230=DIRECTION('center_axis',(-1.,0.,0.));
#35231=DIRECTION('ref_axis',(0.,0.,1.));
#35232=DIRECTION('',(-1.,0.,0.));
#35233=DIRECTION('center_axis',(-1.,0.,0.));
#35234=DIRECTION('ref_axis',(0.,0.,1.));
#35235=DIRECTION('',(-1.,0.,0.));
#35236=DIRECTION('center_axis',(1.,0.,0.));
#35237=DIRECTION('ref_axis',(0.,1.,0.));
#35238=DIRECTION('',(0.,0.,1.));
#35239=DIRECTION('',(0.,0.,1.));
#35240=DIRECTION('center_axis',(0.,1.,0.));
#35241=DIRECTION('ref_axis',(1.,0.,0.));
#35242=DIRECTION('',(0.,0.,1.));
#35243=DIRECTION('center_axis',(0.,1.,0.));
#35244=DIRECTION('ref_axis',(1.,0.,0.));
#35245=DIRECTION('',(0.,0.,1.));
#35246=DIRECTION('center_axis',(1.,0.,0.));
#35247=DIRECTION('ref_axis',(0.,1.,0.));
#35248=DIRECTION('',(0.,0.,1.));
#35249=DIRECTION('center_axis',(0.,-1.,0.));
#35250=DIRECTION('ref_axis',(0.,0.,-1.));
#35251=DIRECTION('',(0.,0.,1.));
#35252=DIRECTION('center_axis',(-1.,0.,0.));
#35253=DIRECTION('ref_axis',(0.,0.,1.));
#35254=DIRECTION('',(0.,0.,1.));
#35255=DIRECTION('center_axis',(0.,1.,0.));
#35256=DIRECTION('ref_axis',(1.,0.,0.));
#35257=DIRECTION('',(0.,0.,1.));
#35258=DIRECTION('center_axis',(-1.,0.,0.));
#35259=DIRECTION('ref_axis',(0.,0.,1.));
#35260=DIRECTION('center_axis',(0.855183382508501,0.518325556268759,0.));
#35261=DIRECTION('ref_axis',(0.,0.,-1.));
#35262=DIRECTION('',(0.,0.,1.));
#35263=DIRECTION('center_axis',(-0.855183382508501,-0.518325556268759,0.));
#35264=DIRECTION('ref_axis',(-0.518325556268759,0.855183382508501,0.));
#35265=DIRECTION('',(0.,0.,1.));
#35266=DIRECTION('center_axis',(0.,1.,0.));
#35267=DIRECTION('ref_axis',(1.,0.,0.));
#35268=DIRECTION('',(0.,0.,1.));
#35269=DIRECTION('',(-1.,0.,0.));
#35270=DIRECTION('center_axis',(-0.855183382509445,-0.518325556267202,0.));
#35271=DIRECTION('ref_axis',(-0.518325556267202,0.855183382509445,0.));
#35272=DIRECTION('',(0.,0.,1.));
#35273=DIRECTION('center_axis',(-0.855183382509445,-0.518325556267202,0.));
#35274=DIRECTION('ref_axis',(-0.518325556267202,0.855183382509445,0.));
#35275=DIRECTION('center_axis',(0.,-1.,0.));
#35276=DIRECTION('ref_axis',(0.,0.,-1.));
#35277=DIRECTION('',(0.,0.,1.));
#35278=DIRECTION('',(1.,0.,0.));
#35279=DIRECTION('',(0.,0.,1.));
#35280=DIRECTION('center_axis',(0.829037572548639,-0.55919290348024,0.));
#35281=DIRECTION('ref_axis',(0.,0.,-1.));
#35282=DIRECTION('',(0.,0.,1.));
#35283=DIRECTION('center_axis',(-0.829037572548647,0.559192903480227,3.27863405626968E-13));
#35284=DIRECTION('ref_axis',(-0.0128476572568338,-0.0190474351859132,0.999736031618271));
#35285=DIRECTION('center_axis',(-1.,0.,0.));
#35286=DIRECTION('ref_axis',(0.,0.,1.));
#35287=DIRECTION('',(0.,0.,1.));
#35288=DIRECTION('center_axis',(1.,0.,0.));
#35289=DIRECTION('ref_axis',(0.,0.,1.));
#35290=DIRECTION('center_axis',(0.,-1.,0.));
#35291=DIRECTION('ref_axis',(0.,0.,-1.));
#35292=DIRECTION('',(0.,0.,1.));
#35293=DIRECTION('',(1.,0.,0.));
#35294=DIRECTION('center_axis',(1.,0.,0.));
#35295=DIRECTION('ref_axis',(0.,1.,0.));
#35296=DIRECTION('',(0.,0.,1.));
#35297=DIRECTION('center_axis',(-1.,0.,0.));
#35298=DIRECTION('ref_axis',(0.,0.,1.));
#35299=DIRECTION('center_axis',(0.,1.,0.));
#35300=DIRECTION('ref_axis',(1.,0.,0.));
#35301=DIRECTION('',(0.,0.,1.));
#35302=DIRECTION('',(-1.,0.,0.));
#35303=DIRECTION('center_axis',(-1.,0.,0.));
#35304=DIRECTION('ref_axis',(0.,0.,1.));
#35305=DIRECTION('center_axis',(1.,0.,0.));
#35306=DIRECTION('ref_axis',(0.,0.,1.));
#35307=DIRECTION('center_axis',(-0.82903757255312,0.559192903473596,0.));
#35308=DIRECTION('ref_axis',(0.,0.,1.));
#35309=DIRECTION('center_axis',(0.82903757255312,-0.559192903473596,0.));
#35310=DIRECTION('ref_axis',(0.559192903473596,0.82903757255312,0.));
#35311=DIRECTION('center_axis',(-1.,0.,0.));
#35312=DIRECTION('ref_axis',(0.,0.,1.));
#35313=DIRECTION('center_axis',(-1.,0.,0.));
#35314=DIRECTION('ref_axis',(0.,0.,1.));
#35315=DIRECTION('center_axis',(0.500000000001141,-0.86602540378378,9.20240256887291E-14));
#35316=DIRECTION('ref_axis',(0.86602540378378,0.500000000001141,4.288515013244E-11));
#35317=DIRECTION('',(1.,0.,0.));
#35318=DIRECTION('center_axis',(-0.500000000011408,0.866025403777852,-2.56081897120736E-13));
#35319=DIRECTION('ref_axis',(0.866025403777852,0.500000000011408,4.05069188609369E-10));
#35320=DIRECTION('center_axis',(0.500000000011408,0.866025403777853,-2.33813906066936E-13));
#35321=DIRECTION('ref_axis',(0.866025403777853,-0.500000000011407,3.46137901213225E-10));
#35322=DIRECTION('',(1.,0.,0.));
#35323=DIRECTION('center_axis',(-0.50000000000114,-0.86602540378378,7.66866880739418E-14));
#35324=DIRECTION('ref_axis',(0.86602540378378,-0.50000000000114,2.49921069793427E-11));
#35325=DIRECTION('center_axis',(0.500000000011394,-0.866025403777861,0.));
#35326=DIRECTION('ref_axis',(0.,0.,-1.));
#35327=DIRECTION('',(0.,0.,1.));
#35328=DIRECTION('',(0.,0.,1.));
#35329=DIRECTION('center_axis',(-0.500000000011394,-0.866025403777861,0.));
#35330=DIRECTION('ref_axis',(-0.866025403777861,0.500000000011394,0.));
#35331=DIRECTION('',(0.,0.,1.));
#35332=DIRECTION('center_axis',(0.,-1.,0.));
#35333=DIRECTION('ref_axis',(0.,0.,-1.));
#35334=DIRECTION('',(0.,0.,1.));
#35335=DIRECTION('center_axis',(-0.500000000001135,0.866025403783784,0.));
#35336=DIRECTION('ref_axis',(0.,0.,1.));
#35337=DIRECTION('',(0.,0.,1.));
#35338=DIRECTION('center_axis',(0.500000000001135,0.866025403783784,0.));
#35339=DIRECTION('ref_axis',(0.,0.,-1.));
#35340=DIRECTION('',(0.,0.,1.));
#35341=DIRECTION('center_axis',(0.,-1.,0.));
#35342=DIRECTION('ref_axis',(0.,0.,-1.));
#35343=DIRECTION('center_axis',(0.,1.,0.));
#35344=DIRECTION('ref_axis',(1.,0.,0.));
#35345=DIRECTION('',(0.,0.,1.));
#35346=DIRECTION('',(-1.,0.,0.));
#35347=DIRECTION('',(0.,0.,1.));
#35348=DIRECTION('center_axis',(-0.500000000001135,-0.866025403783784,0.));
#35349=DIRECTION('ref_axis',(-0.866025403783784,0.500000000001135,0.));
#35350=DIRECTION('',(0.,0.,1.));
#35351=DIRECTION('center_axis',(0.500000000001142,0.866025403783779,1.0736136330352E-13));
#35352=DIRECTION('ref_axis',(0.866025403783779,-0.500000000001142,-1.03942187968842E-11));
#35353=DIRECTION('center_axis',(0.500000000001135,-0.866025403783784,0.));
#35354=DIRECTION('ref_axis',(0.,0.,-1.));
#35355=DIRECTION('',(0.,0.,1.));
#35356=DIRECTION('center_axis',(-0.500000000001139,0.866025403783781,6.13493504591534E-14));
#35357=DIRECTION('ref_axis',(0.866025403783781,0.500000000001139,4.35266584402982E-13));
#35358=DIRECTION('center_axis',(0.,1.,0.));
#35359=DIRECTION('ref_axis',(1.,0.,0.));
#35360=DIRECTION('',(0.,0.,1.));
#35361=DIRECTION('',(-1.,0.,0.));
#35362=DIRECTION('center_axis',(0.500000000011394,0.866025403777861,0.));
#35363=DIRECTION('ref_axis',(0.,0.,-1.));
#35364=DIRECTION('center_axis',(-0.50000000001141,-0.866025403777851,-2.89483883701782E-13));
#35365=DIRECTION('ref_axis',(0.866025403777851,-0.50000000001141,-1.20134541954323E-10));
#35366=DIRECTION('',(0.,0.,1.));
#35367=DIRECTION('center_axis',(-0.500000000011394,0.866025403777861,0.));
#35368=DIRECTION('ref_axis',(0.,0.,1.));
#35369=DIRECTION('center_axis',(0.500000000011409,-0.866025403777852,-2.67215892647728E-13));
#35370=DIRECTION('ref_axis',(0.866025403777852,0.500000000011409,1.29145984166572E-9));
#35371=DIRECTION('center_axis',(-1.,0.,0.));
#35372=DIRECTION('ref_axis',(0.,0.,1.));
#35373=DIRECTION('center_axis',(0.946028810160758,0.324082536317247,0.));
#35374=DIRECTION('ref_axis',(0.,0.,-1.));
#35375=DIRECTION('',(0.,0.,1.));
#35376=DIRECTION('center_axis',(-0.94602881016076,-0.324082536317244,6.79718201582214E-14));
#35377=DIRECTION('ref_axis',(-0.0242942123306427,0.0709171961136464,0.997186312853627));
#35378=DIRECTION('',(0.,0.,1.));
#35379=DIRECTION('center_axis',(0.,1.,0.));
#35380=DIRECTION('ref_axis',(1.,0.,0.));
#35381=DIRECTION('',(0.,0.,1.));
#35382=DIRECTION('',(-1.,0.,0.));
#35383=DIRECTION('center_axis',(-0.946028810171404,-0.324082536286173,0.));
#35384=DIRECTION('ref_axis',(-0.324082536286173,0.946028810171404,0.));
#35385=DIRECTION('',(0.,0.,1.));
#35386=DIRECTION('center_axis',(0.946028810149194,0.324082536351006,1.04940553439243E-9));
#35387=DIRECTION('ref_axis',(-0.00521156151927112,0.015213057603577,0.999870692892276));
#35388=DIRECTION('center_axis',(0.,0.,1.));
#35389=DIRECTION('ref_axis',(-0.587785252292473,0.809016994374947,0.));
#35390=DIRECTION('',(0.,0.,1.));
#35391=DIRECTION('center_axis',(0.,-1.,0.));
#35392=DIRECTION('ref_axis',(0.,0.,-1.));
#35393=DIRECTION('',(0.,0.,1.));
#35394=DIRECTION('',(1.,0.,0.));
#35395=DIRECTION('center_axis',(1.,0.,0.));
#35396=DIRECTION('ref_axis',(0.,1.,0.));
#35397=DIRECTION('',(0.,0.,1.));
#35398=DIRECTION('center_axis',(1.,0.,0.));
#35399=DIRECTION('ref_axis',(0.,0.,1.));
#35400=DIRECTION('',(0.,0.,1.));
#35401=DIRECTION('center_axis',(0.,-1.,0.));
#35402=DIRECTION('ref_axis',(0.,0.,-1.));
#35403=DIRECTION('',(0.,0.,1.));
#35404=DIRECTION('',(-1.,0.,0.));
#35405=DIRECTION('center_axis',(1.,0.,0.));
#35406=DIRECTION('ref_axis',(0.,1.,0.));
#35407=DIRECTION('',(0.,0.,1.));
#35408=DIRECTION('center_axis',(-1.,0.,0.));
#35409=DIRECTION('ref_axis',(0.,0.,1.));
#35410=DIRECTION('center_axis',(0.,1.,0.));
#35411=DIRECTION('ref_axis',(1.,0.,0.));
#35412=DIRECTION('',(0.,0.,1.));
#35413=DIRECTION('',(-1.,0.,0.));
#35414=DIRECTION('center_axis',(-1.,0.,0.));
#35415=DIRECTION('ref_axis',(0.,0.,1.));
#35416=DIRECTION('',(0.,0.,1.));
#35417=DIRECTION('center_axis',(1.,0.,0.));
#35418=DIRECTION('ref_axis',(0.,0.,1.));
#35419=DIRECTION('center_axis',(0.,1.,0.));
#35420=DIRECTION('ref_axis',(1.,0.,0.));
#35421=DIRECTION('',(-1.,0.,0.));
#35422=DIRECTION('center_axis',(0.,0.,1.));
#35423=DIRECTION('ref_axis',(0.,1.,0.));
#35424=DIRECTION('',(0.,0.,1.));
#35425=DIRECTION('center_axis',(0.,1.,0.));
#35426=DIRECTION('ref_axis',(1.,0.,0.));
#35427=DIRECTION('',(1.,0.,0.));
#35428=DIRECTION('center_axis',(-1.,0.,0.));
#35429=DIRECTION('ref_axis',(0.,0.,1.));
#35430=DIRECTION('',(0.,-9.48817606357755E-32,1.));
#35431=DIRECTION('',(1.,4.93038065763132E-32,4.67803197400633E-63));
#35432=DIRECTION('',(0.,-9.48817606357755E-32,1.));
#35433=DIRECTION('',(1.,4.93038065763132E-32,4.67803197400633E-63));
#35434=DIRECTION('',(0.,-9.48817606357755E-32,1.));
#35435=DIRECTION('',(1.,4.93038065763132E-32,4.67803197400633E-63));
#35436=DIRECTION('',(0.,-9.48817606357755E-32,1.));
#35437=DIRECTION('',(1.,4.93038065763132E-32,4.67803197400633E-63));
#35438=DIRECTION('',(0.,-9.48817606357755E-32,1.));
#35439=DIRECTION('',(1.,4.93038065763132E-32,4.67803197400633E-63));
#35440=DIRECTION('',(0.,-9.48817606357755E-32,1.));
#35441=DIRECTION('',(1.,4.93038065763132E-32,4.67803197400633E-63));
#35442=DIRECTION('',(0.,-9.48817606357755E-32,1.));
#35443=DIRECTION('',(1.,4.93038065763132E-32,4.67803197400633E-63));
#35444=DIRECTION('',(0.,-9.48817606357755E-32,1.));
#35445=DIRECTION('',(1.,4.93038065763132E-32,4.67803197400633E-63));
#35446=DIRECTION('',(0.,-9.48817606357755E-32,1.));
#35447=DIRECTION('',(1.,4.93038065763132E-32,4.67803197400633E-63));
#35448=DIRECTION('',(0.,-9.48817606357755E-32,1.));
#35449=DIRECTION('',(1.,2.46519032881566E-32,2.33901598700316E-63));
#35450=DIRECTION('axis',(0.,0.,1.));
#35451=DIRECTION('refdir',(1.,0.,0.));
#35452=DIRECTION('center_axis',(0.,-1.,0.));
#35453=DIRECTION('ref_axis',(0.,0.,-1.));
#35454=DIRECTION('center_axis',(0.,-1.,0.));
#35455=DIRECTION('ref_axis',(0.,0.,-1.));
#35456=DIRECTION('',(0.,-1.,0.));
#35457=DIRECTION('center_axis',(0.,-1.,0.));
#35458=DIRECTION('ref_axis',(0.,0.,-1.));
#35459=DIRECTION('center_axis',(0.,-1.,0.));
#35460=DIRECTION('ref_axis',(0.,0.,-1.));
#35461=DIRECTION('',(-1.04972719113862E-16,-0.515038074910054,0.857167300702112));
#35462=DIRECTION('center_axis',(0.,-1.,0.));
#35463=DIRECTION('ref_axis',(0.,0.,-1.));
#35464=DIRECTION('center_axis',(0.,-1.,0.));
#35465=DIRECTION('ref_axis',(0.,0.,-1.));
#35466=DIRECTION('',(0.,-1.,0.));
#35467=DIRECTION('center_axis',(0.,-1.,0.));
#35468=DIRECTION('ref_axis',(0.,0.,-1.));
#35469=DIRECTION('center_axis',(0.,-1.,0.));
#35470=DIRECTION('ref_axis',(0.,0.,-1.));
#35471=DIRECTION('',(-1.04972719113862E-16,-0.515038074910054,0.857167300702112));
#35472=DIRECTION('center_axis',(0.,-1.,0.));
#35473=DIRECTION('ref_axis',(0.,0.,-1.));
#35474=DIRECTION('center_axis',(0.,-1.,0.));
#35475=DIRECTION('ref_axis',(0.,0.,-1.));
#35476=DIRECTION('',(0.,-1.,0.));
#35477=DIRECTION('center_axis',(0.,-1.,0.));
#35478=DIRECTION('ref_axis',(0.,0.,-1.));
#35479=DIRECTION('center_axis',(0.,-1.,0.));
#35480=DIRECTION('ref_axis',(0.,0.,-1.));
#35481=DIRECTION('',(-1.04972719113862E-16,-0.515038074910054,0.857167300702112));
#35482=DIRECTION('center_axis',(0.,-1.,0.));
#35483=DIRECTION('ref_axis',(0.,0.,-1.));
#35484=DIRECTION('center_axis',(0.,-1.,0.));
#35485=DIRECTION('ref_axis',(0.,0.,-1.));
#35486=DIRECTION('',(0.,-1.,0.));
#35487=DIRECTION('center_axis',(0.,-1.,0.));
#35488=DIRECTION('ref_axis',(0.,0.,-1.));
#35489=DIRECTION('center_axis',(0.,-1.,0.));
#35490=DIRECTION('ref_axis',(0.,0.,-1.));
#35491=DIRECTION('',(-1.04972719113862E-16,-0.515038074910054,0.857167300702112));
#35492=DIRECTION('center_axis',(0.,-1.,0.));
#35493=DIRECTION('ref_axis',(0.,0.,-1.));
#35494=DIRECTION('center_axis',(0.,-1.,0.));
#35495=DIRECTION('ref_axis',(0.,0.,-1.));
#35496=DIRECTION('',(0.,-1.,0.));
#35497=DIRECTION('center_axis',(0.,-1.,0.));
#35498=DIRECTION('ref_axis',(0.,0.,-1.));
#35499=DIRECTION('center_axis',(0.,-1.,0.));
#35500=DIRECTION('ref_axis',(0.,0.,-1.));
#35501=DIRECTION('',(-1.04972719113862E-16,-0.515038074910054,0.857167300702112));
#35502=DIRECTION('center_axis',(0.,-1.,0.));
#35503=DIRECTION('ref_axis',(0.,0.,-1.));
#35504=DIRECTION('center_axis',(0.,-1.,0.));
#35505=DIRECTION('ref_axis',(0.,0.,-1.));
#35506=DIRECTION('',(0.,-1.,0.));
#35507=DIRECTION('center_axis',(0.,-1.,0.));
#35508=DIRECTION('ref_axis',(0.,0.,-1.));
#35509=DIRECTION('center_axis',(0.,-1.,0.));
#35510=DIRECTION('ref_axis',(0.,0.,-1.));
#35511=DIRECTION('',(-1.04972719113862E-16,-0.515038074910054,0.857167300702112));
#35512=DIRECTION('center_axis',(0.,-1.,0.));
#35513=DIRECTION('ref_axis',(0.,0.,-1.));
#35514=DIRECTION('center_axis',(0.,-1.,0.));
#35515=DIRECTION('ref_axis',(0.,0.,-1.));
#35516=DIRECTION('',(0.,-1.,0.));
#35517=DIRECTION('center_axis',(0.,-1.,0.));
#35518=DIRECTION('ref_axis',(0.,0.,-1.));
#35519=DIRECTION('center_axis',(0.,-1.,0.));
#35520=DIRECTION('ref_axis',(0.,0.,-1.));
#35521=DIRECTION('',(-1.04972719113862E-16,-0.515038074910054,0.857167300702112));
#35522=DIRECTION('center_axis',(0.,-1.,0.));
#35523=DIRECTION('ref_axis',(0.,0.,-1.));
#35524=DIRECTION('center_axis',(0.,-1.,0.));
#35525=DIRECTION('ref_axis',(0.,0.,-1.));
#35526=DIRECTION('',(0.,-1.,0.));
#35527=DIRECTION('center_axis',(0.,-1.,0.));
#35528=DIRECTION('ref_axis',(0.,0.,-1.));
#35529=DIRECTION('center_axis',(0.,-1.,0.));
#35530=DIRECTION('ref_axis',(0.,0.,-1.));
#35531=DIRECTION('',(-1.04972719113862E-16,-0.515038074910057,0.857167300702111));
#35532=DIRECTION('center_axis',(0.,-1.,0.));
#35533=DIRECTION('ref_axis',(0.,0.,-1.));
#35534=DIRECTION('center_axis',(0.,-1.,0.));
#35535=DIRECTION('ref_axis',(0.,0.,-1.));
#35536=DIRECTION('',(0.,-1.,0.));
#35537=DIRECTION('center_axis',(0.,-1.,0.));
#35538=DIRECTION('ref_axis',(0.,0.,-1.));
#35539=DIRECTION('center_axis',(0.,-1.,0.));
#35540=DIRECTION('ref_axis',(0.,0.,-1.));
#35541=DIRECTION('',(-1.04972719113862E-16,-0.515038074910054,0.857167300702112));
#35542=DIRECTION('center_axis',(0.,-1.,0.));
#35543=DIRECTION('ref_axis',(0.,0.,-1.));
#35544=DIRECTION('center_axis',(0.,-1.,0.));
#35545=DIRECTION('ref_axis',(0.,0.,-1.));
#35546=DIRECTION('',(0.,-1.,0.));
#35547=DIRECTION('center_axis',(0.,-1.,0.));
#35548=DIRECTION('ref_axis',(0.,0.,-1.));
#35549=DIRECTION('center_axis',(0.,-1.,0.));
#35550=DIRECTION('ref_axis',(0.,0.,-1.));
#35551=DIRECTION('',(-1.04972719113862E-16,-0.515038074910054,0.857167300702112));
#35552=DIRECTION('center_axis',(0.,-1.,0.));
#35553=DIRECTION('ref_axis',(0.,0.,-1.));
#35554=DIRECTION('center_axis',(0.,-1.,0.));
#35555=DIRECTION('ref_axis',(0.,0.,-1.));
#35556=DIRECTION('',(0.,-1.,0.));
#35557=DIRECTION('center_axis',(0.,-1.,0.));
#35558=DIRECTION('ref_axis',(0.,0.,-1.));
#35559=DIRECTION('center_axis',(0.,-1.,0.));
#35560=DIRECTION('ref_axis',(0.,0.,-1.));
#35561=DIRECTION('',(-1.04972719113862E-16,-0.515038074910054,0.857167300702112));
#35562=DIRECTION('center_axis',(0.,-1.,0.));
#35563=DIRECTION('ref_axis',(0.,0.,-1.));
#35564=DIRECTION('center_axis',(0.,-1.,0.));
#35565=DIRECTION('ref_axis',(0.,0.,-1.));
#35566=DIRECTION('',(0.,-1.,0.));
#35567=DIRECTION('center_axis',(0.,-1.,0.));
#35568=DIRECTION('ref_axis',(0.,0.,-1.));
#35569=DIRECTION('center_axis',(0.,-1.,0.));
#35570=DIRECTION('ref_axis',(0.,0.,-1.));
#35571=DIRECTION('',(-1.04972719113862E-16,-0.515038074910054,0.857167300702112));
#35572=DIRECTION('center_axis',(0.,-1.,0.));
#35573=DIRECTION('ref_axis',(0.,0.,-1.));
#35574=DIRECTION('center_axis',(0.,-1.,0.));
#35575=DIRECTION('ref_axis',(0.,0.,-1.));
#35576=DIRECTION('',(0.,-1.,0.));
#35577=DIRECTION('center_axis',(0.,-1.,0.));
#35578=DIRECTION('ref_axis',(0.,0.,-1.));
#35579=DIRECTION('center_axis',(0.,-1.,0.));
#35580=DIRECTION('ref_axis',(0.,0.,-1.));
#35581=DIRECTION('',(-1.04972719113862E-16,-0.515038074910054,0.857167300702112));
#35582=DIRECTION('center_axis',(0.,-1.,0.));
#35583=DIRECTION('ref_axis',(0.,0.,-1.));
#35584=DIRECTION('center_axis',(0.,-1.,0.));
#35585=DIRECTION('ref_axis',(0.,0.,-1.));
#35586=DIRECTION('',(0.,-1.,0.));
#35587=DIRECTION('center_axis',(0.,-1.,0.));
#35588=DIRECTION('ref_axis',(0.,0.,-1.));
#35589=DIRECTION('center_axis',(0.,-1.,0.));
#35590=DIRECTION('ref_axis',(0.,0.,-1.));
#35591=DIRECTION('',(-1.04972719113862E-16,-0.515038074910054,0.857167300702112));
#35592=DIRECTION('center_axis',(0.,-1.,0.));
#35593=DIRECTION('ref_axis',(0.,0.,-1.));
#35594=DIRECTION('center_axis',(0.,-1.,0.));
#35595=DIRECTION('ref_axis',(0.,0.,-1.));
#35596=DIRECTION('',(0.,-1.,0.));
#35597=DIRECTION('center_axis',(0.,-1.,0.));
#35598=DIRECTION('ref_axis',(0.,0.,-1.));
#35599=DIRECTION('center_axis',(0.,-1.,0.));
#35600=DIRECTION('ref_axis',(0.,0.,-1.));
#35601=DIRECTION('',(-1.04972719113862E-16,-0.515038074910054,0.857167300702112));
#35602=DIRECTION('center_axis',(0.,-1.,0.));
#35603=DIRECTION('ref_axis',(0.,0.,-1.));
#35604=DIRECTION('center_axis',(0.,-1.,0.));
#35605=DIRECTION('ref_axis',(0.,0.,-1.));
#35606=DIRECTION('',(0.,-1.,0.));
#35607=DIRECTION('center_axis',(0.,-1.,0.));
#35608=DIRECTION('ref_axis',(0.,0.,-1.));
#35609=DIRECTION('center_axis',(0.,-1.,0.));
#35610=DIRECTION('ref_axis',(0.,0.,-1.));
#35611=DIRECTION('',(-1.04972719113862E-16,-0.515038074910057,0.857167300702111));
#35612=DIRECTION('center_axis',(0.,-1.,0.));
#35613=DIRECTION('ref_axis',(0.,0.,-1.));
#35614=DIRECTION('center_axis',(0.,-1.,0.));
#35615=DIRECTION('ref_axis',(0.,0.,-1.));
#35616=DIRECTION('',(0.,-1.,0.));
#35617=DIRECTION('center_axis',(0.,-1.,0.));
#35618=DIRECTION('ref_axis',(0.,0.,-1.));
#35619=DIRECTION('center_axis',(0.,-1.,0.));
#35620=DIRECTION('ref_axis',(0.,0.,-1.));
#35621=DIRECTION('',(-1.04972719113862E-16,-0.515038074910056,0.857167300702111));
#35622=DIRECTION('center_axis',(0.,1.,0.));
#35623=DIRECTION('ref_axis',(0.,0.,1.));
#35624=DIRECTION('',(0.,0.,-1.));
#35625=DIRECTION('',(1.,0.,0.));
#35626=DIRECTION('',(0.,0.,-1.));
#35627=DIRECTION('',(1.,0.,0.));
#35628=DIRECTION('center_axis',(-1.,0.,0.));
#35629=DIRECTION('ref_axis',(0.,0.,1.));
#35630=DIRECTION('',(0.,-1.,0.));
#35631=DIRECTION('center_axis',(-1.,0.,0.));
#35632=DIRECTION('ref_axis',(0.,0.,1.));
#35633=DIRECTION('',(0.,0.,1.));
#35634=DIRECTION('center_axis',(-1.,0.,0.));
#35635=DIRECTION('ref_axis',(0.,0.,1.));
#35636=DIRECTION('',(0.,1.,0.));
#35637=DIRECTION('',(0.,0.,-1.));
#35638=DIRECTION('',(0.,1.,0.));
#35639=DIRECTION('',(0.,0.,-1.));
#35640=DIRECTION('',(0.,1.,0.));
#35641=DIRECTION('center_axis',(0.,-1.,0.));
#35642=DIRECTION('ref_axis',(0.,0.,-1.));
#35643=DIRECTION('',(-1.,0.,0.));
#35644=DIRECTION('',(0.,0.,-1.));
#35645=DIRECTION('',(-1.,0.,0.));
#35646=DIRECTION('center_axis',(1.,0.,0.));
#35647=DIRECTION('ref_axis',(0.,0.,-1.));
#35648=DIRECTION('',(0.,1.,0.));
#35649=DIRECTION('center_axis',(1.,0.,0.));
#35650=DIRECTION('ref_axis',(0.,0.,-1.));
#35651=DIRECTION('',(0.,0.,1.));
#35652=DIRECTION('center_axis',(1.,0.,0.));
#35653=DIRECTION('ref_axis',(0.,0.,-1.));
#35654=DIRECTION('',(0.,-1.,0.));
#35655=DIRECTION('',(0.,-1.,0.));
#35656=DIRECTION('',(0.,-1.,0.));
#35657=DIRECTION('',(0.,0.,-1.));
#35658=DIRECTION('center_axis',(0.,1.,0.));
#35659=DIRECTION('ref_axis',(0.,0.,1.));
#35660=DIRECTION('',(1.,0.,0.));
#35661=DIRECTION('',(1.,0.,0.));
#35662=DIRECTION('center_axis',(0.,0.,1.));
#35663=DIRECTION('ref_axis',(1.,0.,0.));
#35664=DIRECTION('center_axis',(0.,0.,1.));
#35665=DIRECTION('ref_axis',(1.,0.,0.));
#35666=DIRECTION('center_axis',(0.,0.,1.));
#35667=DIRECTION('ref_axis',(1.,0.,0.));
#35668=DIRECTION('',(1.,0.,0.));
#35669=DIRECTION('center_axis',(0.,1.,0.));
#35670=DIRECTION('ref_axis',(0.,0.,1.));
#35671=DIRECTION('',(1.,0.,0.));
#35672=DIRECTION('',(-1.,0.,0.));
#35673=DIRECTION('center_axis',(0.,0.,-1.));
#35674=DIRECTION('ref_axis',(-1.,0.,0.));
#35675=DIRECTION('',(-1.,0.,0.));
#35676=DIRECTION('center_axis',(-1.,0.,0.));
#35677=DIRECTION('ref_axis',(0.,0.,1.));
#35678=DIRECTION('center_axis',(-1.,0.,0.));
#35679=DIRECTION('ref_axis',(0.,0.,1.));
#35680=DIRECTION('axis',(0.,0.,1.));
#35681=DIRECTION('refdir',(1.,0.,0.));
#35682=DIRECTION('center_axis',(1.,1.22464679914735E-16,0.));
#35683=DIRECTION('ref_axis',(-1.22464679914735E-16,1.,0.));
#35684=DIRECTION('center_axis',(1.,1.22464679914735E-16,0.));
#35685=DIRECTION('ref_axis',(-1.22464679914735E-16,1.,0.));
#35686=DIRECTION('',(-1.,-1.22464679914735E-16,0.));
#35687=DIRECTION('center_axis',(1.,1.22464679914735E-16,0.));
#35688=DIRECTION('ref_axis',(-1.22464679914735E-16,1.,0.));
#35689=DIRECTION('center_axis',(1.,1.22464679914735E-16,0.));
#35690=DIRECTION('ref_axis',(-1.22464679914735E-16,1.,0.));
#35691=DIRECTION('',(-0.70710678118655,0.707106781186545,8.6595605623549E-17));
#35692=DIRECTION('center_axis',(1.,1.22464679914735E-16,0.));
#35693=DIRECTION('ref_axis',(-1.22464679914735E-16,1.,0.));
#35694=DIRECTION('center_axis',(-1.,-1.22464679914735E-16,0.));
#35695=DIRECTION('ref_axis',(1.22464679914735E-16,-1.,0.));
#35696=DIRECTION('center_axis',(1.,1.22464679914735E-16,0.));
#35697=DIRECTION('ref_axis',(-1.22464679914735E-16,1.,0.));
#35698=DIRECTION('',(0.707106781186548,-0.707106781186547,8.65956056235493E-17));
#35699=DIRECTION('center_axis',(1.,1.22464679914735E-16,0.));
#35700=DIRECTION('ref_axis',(-1.22464679914735E-16,1.,0.));
#35701=DIRECTION('center_axis',(1.,1.22464679914735E-16,0.));
#35702=DIRECTION('ref_axis',(-1.22464679914735E-16,1.,0.));
#35703=DIRECTION('center_axis',(1.,1.22464679914735E-16,0.));
#35704=DIRECTION('ref_axis',(-1.22464679914735E-16,1.,0.));
#35705=DIRECTION('',(-1.,-1.22464679914735E-16,0.));
#35706=DIRECTION('center_axis',(1.,1.22464679914735E-16,0.));
#35707=DIRECTION('ref_axis',(-1.22464679914735E-16,1.,0.));
#35708=DIRECTION('center_axis',(1.,1.22464679914735E-16,0.));
#35709=DIRECTION('ref_axis',(-1.22464679914735E-16,1.,0.));
#35710=DIRECTION('center_axis',(-1.,-1.22464679914735E-16,0.));
#35711=DIRECTION('ref_axis',(1.22464679914735E-16,-1.,0.));
#35712=DIRECTION('',(0.,0.5,-0.866025403784439));
#35713=DIRECTION('',(0.,1.,0.));
#35714=DIRECTION('',(0.,0.5,0.866025403784439));
#35715=DIRECTION('',(0.,-0.5,0.866025403784438));
#35716=DIRECTION('',(0.,-1.,-1.50231459873716E-16));
#35717=DIRECTION('',(0.,-0.5,-0.866025403784439));
#35718=DIRECTION('center_axis',(1.,1.22464679914735E-16,0.));
#35719=DIRECTION('ref_axis',(-1.22464679914735E-16,1.,0.));
#35720=DIRECTION('center_axis',(-1.06057523872491E-16,0.866025403784439,
0.5));
#35721=DIRECTION('ref_axis',(-5.09861652542584E-33,-0.5,0.866025403784439));
#35722=DIRECTION('',(-1.,-1.22464679914735E-16,0.));
#35723=DIRECTION('',(0.,0.5,-0.866025403784439));
#35724=DIRECTION('',(-1.,-1.22464679914735E-16,0.));
#35725=DIRECTION('center_axis',(0.,0.,1.));
#35726=DIRECTION('ref_axis',(1.,0.,0.));
#35727=DIRECTION('',(0.,1.,0.));
#35728=DIRECTION('',(-1.,-1.22464679914735E-16,0.));
#35729=DIRECTION('center_axis',(1.06057523872491E-16,-0.866025403784439,
0.5));
#35730=DIRECTION('ref_axis',(-8.4117933897259E-34,-0.5,-0.866025403784439));
#35731=DIRECTION('',(0.,0.5,0.866025403784439));
#35732=DIRECTION('',(-1.,-1.22464679914735E-16,0.));
#35733=DIRECTION('center_axis',(1.06057523872491E-16,-0.866025403784439,
-0.5));
#35734=DIRECTION('ref_axis',(-5.93979586439842E-33,0.5,-0.866025403784439));
#35735=DIRECTION('',(0.,-0.5,0.866025403784438));
#35736=DIRECTION('',(-1.,-1.22464679914735E-16,0.));
#35737=DIRECTION('center_axis',(-1.8398047646558E-32,1.50231459873716E-16,
-1.));
#35738=DIRECTION('ref_axis',(0.,1.,1.50231459873716E-16));
#35739=DIRECTION('',(0.,-1.,-1.50231459873716E-16));
#35740=DIRECTION('',(-1.,-1.22464679914735E-16,0.));
#35741=DIRECTION('center_axis',(-1.06057523872491E-16,0.866025403784439,
-0.5));
#35742=DIRECTION('ref_axis',(2.96989793219921E-33,0.5,0.866025403784439));
#35743=DIRECTION('',(0.,-0.5,-0.866025403784439));
#35744=DIRECTION('center_axis',(-1.,0.,0.));
#35745=DIRECTION('ref_axis',(0.,0.,1.));
#35746=DIRECTION('axis',(0.,0.,1.));
#35747=DIRECTION('refdir',(1.,0.,0.));
#35748=DIRECTION('center_axis',(1.,0.,0.));
#35749=DIRECTION('ref_axis',(0.,0.,-1.));
#35750=DIRECTION('center_axis',(1.,0.,0.));
#35751=DIRECTION('ref_axis',(0.,0.,-1.));
#35752=DIRECTION('center_axis',(1.,0.,0.));
#35753=DIRECTION('ref_axis',(0.,0.,-1.));
#35754=DIRECTION('',(-0.70710678118655,8.65956056235489E-17,-0.707106781186544));
#35755=DIRECTION('center_axis',(-1.,0.,0.));
#35756=DIRECTION('ref_axis',(0.,0.,-1.));
#35757=DIRECTION('center_axis',(-1.,5.24877093477881E-17,0.));
#35758=DIRECTION('ref_axis',(-5.24877093477881E-17,-1.,0.));
#35759=DIRECTION('',(-0.515038074910058,0.85716730070211,-1.04972719113862E-16));
#35760=DIRECTION('center_axis',(-1.,5.24877093477881E-17,0.));
#35761=DIRECTION('ref_axis',(-5.24877093477881E-17,-1.,0.));
#35762=DIRECTION('center_axis',(-1.,5.24877093477881E-17,0.));
#35763=DIRECTION('ref_axis',(-5.24877093477881E-17,-1.,0.));
#35764=DIRECTION('center_axis',(-1.,5.24877093477881E-17,0.));
#35765=DIRECTION('ref_axis',(-5.24877093477881E-17,-1.,0.));
#35766=DIRECTION('center_axis',(-1.,5.24877093477881E-17,0.));
#35767=DIRECTION('ref_axis',(-5.24877093477881E-17,-1.,0.));
#35768=DIRECTION('center_axis',(-1.,5.24877093477881E-17,0.));
#35769=DIRECTION('ref_axis',(-5.24877093477881E-17,-1.,0.));
#35770=DIRECTION('center_axis',(-1.,5.24877093477881E-17,0.));
#35771=DIRECTION('ref_axis',(-5.24877093477881E-17,-1.,0.));
#35772=DIRECTION('center_axis',(-1.,5.24877093477881E-17,0.));
#35773=DIRECTION('ref_axis',(-5.24877093477881E-17,-1.,0.));
#35774=DIRECTION('center_axis',(-1.,0.,0.));
#35775=DIRECTION('ref_axis',(0.,0.,1.));
#35776=DIRECTION('',(1.,0.,0.));
#35777=DIRECTION('center_axis',(-1.,0.,0.));
#35778=DIRECTION('ref_axis',(0.,0.,1.));
#35779=DIRECTION('center_axis',(-1.,0.,0.));
#35780=DIRECTION('ref_axis',(0.,0.,1.));
#35781=DIRECTION('center_axis',(-1.,0.,0.));
#35782=DIRECTION('ref_axis',(0.,0.,1.));
#35783=DIRECTION('',(1.,0.,0.));
#35784=DIRECTION('center_axis',(-1.,0.,0.));
#35785=DIRECTION('ref_axis',(0.,0.,1.));
#35786=DIRECTION('center_axis',(-1.,0.,0.));
#35787=DIRECTION('ref_axis',(0.,0.,1.));
#35788=DIRECTION('center_axis',(-1.,0.,0.));
#35789=DIRECTION('ref_axis',(0.,0.,1.));
#35790=DIRECTION('',(1.,0.,0.));
#35791=DIRECTION('center_axis',(-1.,0.,0.));
#35792=DIRECTION('ref_axis',(0.,0.,1.));
#35793=DIRECTION('center_axis',(1.,0.,0.));
#35794=DIRECTION('ref_axis',(0.,0.,-1.));
#35795=DIRECTION('',(0.,0.5,-0.866025403784439));
#35796=DIRECTION('',(0.,1.,-1.87789324842145E-16));
#35797=DIRECTION('',(0.,0.5,0.866025403784439));
#35798=DIRECTION('',(0.,-0.5,0.866025403784439));
#35799=DIRECTION('',(0.,-1.,0.));
#35800=DIRECTION('',(0.,-0.5,-0.866025403784439));
#35801=DIRECTION('center_axis',(-1.,0.,0.));
#35802=DIRECTION('ref_axis',(0.,0.,1.));
#35803=DIRECTION('center_axis',(1.,0.,0.));
#35804=DIRECTION('ref_axis',(0.,0.,-1.));
#35805=DIRECTION('center_axis',(-1.,0.,0.));
#35806=DIRECTION('ref_axis',(0.,0.,1.));
#35807=DIRECTION('center_axis',(0.,1.87789324842145E-16,1.));
#35808=DIRECTION('ref_axis',(0.,-1.,1.87789324842145E-16));
#35809=DIRECTION('',(0.,1.,-1.87789324842145E-16));
#35810=DIRECTION('',(-1.,0.,0.));
#35811=DIRECTION('',(-1.,0.,0.));
#35812=DIRECTION('',(0.,1.,-1.87789324842145E-16));
#35813=DIRECTION('center_axis',(0.,-0.866025403784439,0.5));
#35814=DIRECTION('ref_axis',(0.,-0.5,-0.866025403784439));
#35815=DIRECTION('',(0.,0.5,0.866025403784439));
#35816=DIRECTION('',(-1.,0.,0.));
#35817=DIRECTION('',(0.,0.5,0.866025403784439));
#35818=DIRECTION('center_axis',(0.,-0.866025403784439,-0.5));
#35819=DIRECTION('ref_axis',(0.,0.5,-0.866025403784439));
#35820=DIRECTION('',(0.,-0.5,0.866025403784439));
#35821=DIRECTION('',(-1.,0.,0.));
#35822=DIRECTION('',(0.,-0.5,0.866025403784439));
#35823=DIRECTION('center_axis',(0.,0.,-1.));
#35824=DIRECTION('ref_axis',(-1.,0.,0.));
#35825=DIRECTION('',(0.,-1.,0.));
#35826=DIRECTION('',(-1.,0.,0.));
#35827=DIRECTION('',(0.,-1.,0.));
#35828=DIRECTION('center_axis',(0.,0.866025403784439,-0.5));
#35829=DIRECTION('ref_axis',(0.,0.5,0.866025403784439));
#35830=DIRECTION('',(0.,-0.5,-0.866025403784439));
#35831=DIRECTION('',(-1.,0.,0.));
#35832=DIRECTION('',(0.,-0.5,-0.866025403784439));
#35833=DIRECTION('center_axis',(0.,0.866025403784439,0.5));
#35834=DIRECTION('ref_axis',(0.,-0.5,0.866025403784439));
#35835=DIRECTION('',(0.,0.5,-0.866025403784439));
#35836=DIRECTION('',(0.,0.5,-0.866025403784439));
#35837=DIRECTION('center_axis',(-1.,0.,0.));
#35838=DIRECTION('ref_axis',(0.,0.,1.));
#35839=DIRECTION('center_axis',(-1.,0.,0.));
#35840=DIRECTION('ref_axis',(0.,0.,1.));
#35841=DIRECTION('center_axis',(-1.,0.,0.));
#35842=DIRECTION('ref_axis',(0.,0.,1.));
#35843=DIRECTION('center_axis',(-1.,0.,0.));
#35844=DIRECTION('ref_axis',(0.,0.,1.));
#35845=DIRECTION('center_axis',(-1.,0.,0.));
#35846=DIRECTION('ref_axis',(0.,0.,1.));
#35847=DIRECTION('center_axis',(-1.,0.,0.));
#35848=DIRECTION('ref_axis',(0.,0.,1.));
#35849=DIRECTION('center_axis',(-1.,-3.84779799073557E-18,0.));
#35850=DIRECTION('ref_axis',(3.84779799073557E-18,-1.,0.));
#35851=DIRECTION('center_axis',(-1.,-3.84779799073557E-18,0.));
#35852=DIRECTION('ref_axis',(3.84779799073557E-18,-1.,0.));
#35853=DIRECTION('',(1.,3.84779799073557E-18,0.));
#35854=DIRECTION('center_axis',(-1.,-3.84779799073557E-18,0.));
#35855=DIRECTION('ref_axis',(3.84779799073557E-18,-1.,0.));
#35856=DIRECTION('center_axis',(-1.,-3.84779799073557E-18,0.));
#35857=DIRECTION('ref_axis',(3.84779799073557E-18,-1.,0.));
#35858=DIRECTION('center_axis',(-1.,-3.84779799073557E-18,0.));
#35859=DIRECTION('ref_axis',(3.84779799073557E-18,-1.,0.));
#35860=DIRECTION('',(-1.,-3.84779799073557E-18,0.));
#35861=DIRECTION('center_axis',(-1.,-3.84779799073557E-18,0.));
#35862=DIRECTION('ref_axis',(3.84779799073557E-18,-1.,0.));
#35863=DIRECTION('center_axis',(1.,3.84779799073557E-18,0.));
#35864=DIRECTION('ref_axis',(-3.84779799073557E-18,1.,0.));
#35865=DIRECTION('center_axis',(-1.,-3.84779799073557E-18,0.));
#35866=DIRECTION('ref_axis',(3.84779799073557E-18,-1.,0.));
#35867=DIRECTION('center_axis',(-1.,-1.22125762314651E-17,0.));
#35868=DIRECTION('ref_axis',(-3.62527989531715E-33,1.83697019872103E-16,
-1.));
#35869=DIRECTION('center_axis',(-1.,-1.22125762314651E-17,0.));
#35870=DIRECTION('ref_axis',(1.22125762314651E-17,-1.,0.));
#35871=DIRECTION('',(1.,0.,0.));
#35872=DIRECTION('center_axis',(-1.,-1.22125762314651E-17,0.));
#35873=DIRECTION('ref_axis',(1.22125762314651E-17,-1.,0.));
#35874=DIRECTION('',(1.,0.,0.));
#35875=DIRECTION('center_axis',(-1.,-1.22125762314651E-17,0.));
#35876=DIRECTION('ref_axis',(-3.08148791101958E-33,1.83697019872103E-16,
-1.));
#35877=DIRECTION('center_axis',(-1.,-1.22125762314651E-17,0.));
#35878=DIRECTION('ref_axis',(1.22125762314651E-17,-1.,0.));
#35879=DIRECTION('',(1.,0.,0.));
#35880=DIRECTION('center_axis',(-1.,-1.22125762314651E-17,0.));
#35881=DIRECTION('ref_axis',(1.22125762314651E-17,-1.,0.));
#35882=DIRECTION('',(1.,0.,0.));
#35883=DIRECTION('center_axis',(1.,1.22125762314651E-17,0.));
#35884=DIRECTION('ref_axis',(-1.22125762314651E-17,1.,0.));
#35885=DIRECTION('',(0.,0.,-1.));
#35886=DIRECTION('',(0.,0.,1.));
#35887=DIRECTION('center_axis',(-1.,-1.22125762314651E-17,0.));
#35888=DIRECTION('ref_axis',(1.22125762314651E-17,-1.,0.));
#35889=DIRECTION('',(0.,0.,-1.));
#35890=DIRECTION('',(0.,0.,1.));
#35891=DIRECTION('center_axis',(0.,1.,0.));
#35892=DIRECTION('ref_axis',(0.,0.,1.));
#35893=DIRECTION('center_axis',(0.,-1.,0.));
#35894=DIRECTION('ref_axis',(0.,0.,-1.));
#35895=DIRECTION('axis',(0.,0.,1.));
#35896=DIRECTION('refdir',(1.,0.,0.));
#35897=DIRECTION('center_axis',(0.,0.,1.));
#35898=DIRECTION('ref_axis',(1.,0.,0.));
#35899=DIRECTION('center_axis',(0.,0.,1.));
#35900=DIRECTION('ref_axis',(1.,0.,0.));
#35901=DIRECTION('',(0.,0.,1.));
#35902=DIRECTION('center_axis',(0.,0.,1.));
#35903=DIRECTION('ref_axis',(1.,0.,0.));
#35904=DIRECTION('center_axis',(0.,0.,1.));
#35905=DIRECTION('ref_axis',(1.,0.,0.));
#35906=DIRECTION('center_axis',(0.,0.,1.));
#35907=DIRECTION('ref_axis',(1.,0.,0.));
#35908=DIRECTION('',(0.,0.,1.));
#35909=DIRECTION('center_axis',(0.,0.,1.));
#35910=DIRECTION('ref_axis',(1.,0.,0.));
#35911=DIRECTION('center_axis',(0.,0.,1.));
#35912=DIRECTION('ref_axis',(1.,0.,0.));
#35913=DIRECTION('center_axis',(0.,0.,1.));
#35914=DIRECTION('ref_axis',(1.,0.,0.));
#35915=DIRECTION('',(0.,0.,1.));
#35916=DIRECTION('center_axis',(0.,0.,1.));
#35917=DIRECTION('ref_axis',(1.,0.,0.));
#35918=DIRECTION('center_axis',(0.,0.,1.));
#35919=DIRECTION('ref_axis',(1.,0.,0.));
#35920=DIRECTION('center_axis',(0.,0.,1.));
#35921=DIRECTION('ref_axis',(1.,0.,0.));
#35922=DIRECTION('',(0.,0.,1.));
#35923=DIRECTION('center_axis',(0.,0.,1.));
#35924=DIRECTION('ref_axis',(1.,0.,0.));
#35925=DIRECTION('center_axis',(0.,0.,1.));
#35926=DIRECTION('ref_axis',(1.,0.,0.));
#35927=DIRECTION('center_axis',(0.,0.,1.));
#35928=DIRECTION('ref_axis',(1.,0.,0.));
#35929=DIRECTION('',(0.,0.,1.));
#35930=DIRECTION('center_axis',(0.,0.,1.));
#35931=DIRECTION('ref_axis',(1.,0.,0.));
#35932=DIRECTION('center_axis',(0.,0.,1.));
#35933=DIRECTION('ref_axis',(1.,0.,0.));
#35934=DIRECTION('center_axis',(0.,0.,1.));
#35935=DIRECTION('ref_axis',(1.,0.,0.));
#35936=DIRECTION('',(0.,0.,1.));
#35937=DIRECTION('center_axis',(0.,0.,1.));
#35938=DIRECTION('ref_axis',(1.,0.,0.));
#35939=DIRECTION('center_axis',(0.,0.,1.));
#35940=DIRECTION('ref_axis',(1.,0.,0.));
#35941=DIRECTION('center_axis',(0.,0.,1.));
#35942=DIRECTION('ref_axis',(1.,0.,0.));
#35943=DIRECTION('',(0.,0.,1.));
#35944=DIRECTION('center_axis',(0.,0.,1.));
#35945=DIRECTION('ref_axis',(1.,0.,0.));
#35946=DIRECTION('center_axis',(0.,0.,1.));
#35947=DIRECTION('ref_axis',(1.,0.,0.));
#35948=DIRECTION('center_axis',(0.,0.,1.));
#35949=DIRECTION('ref_axis',(1.,0.,0.));
#35950=DIRECTION('',(0.,0.,1.));
#35951=DIRECTION('center_axis',(0.,0.,1.));
#35952=DIRECTION('ref_axis',(1.,0.,0.));
#35953=DIRECTION('center_axis',(0.,0.,1.));
#35954=DIRECTION('ref_axis',(1.,0.,0.));
#35955=DIRECTION('center_axis',(0.,0.,1.));
#35956=DIRECTION('ref_axis',(1.,0.,0.));
#35957=DIRECTION('',(0.,0.,1.));
#35958=DIRECTION('center_axis',(0.,0.,1.));
#35959=DIRECTION('ref_axis',(1.,0.,0.));
#35960=DIRECTION('center_axis',(0.,0.,1.));
#35961=DIRECTION('ref_axis',(1.,0.,0.));
#35962=DIRECTION('center_axis',(0.,0.,1.));
#35963=DIRECTION('ref_axis',(1.,0.,0.));
#35964=DIRECTION('',(0.,0.,1.));
#35965=DIRECTION('center_axis',(0.,0.,1.));
#35966=DIRECTION('ref_axis',(1.,0.,0.));
#35967=DIRECTION('center_axis',(0.,0.,1.));
#35968=DIRECTION('ref_axis',(1.,0.,0.));
#35969=DIRECTION('',(0.,-1.,0.));
#35970=DIRECTION('',(-1.,0.,0.));
#35971=DIRECTION('',(-1.23908819712629E-16,1.,0.));
#35972=DIRECTION('',(1.,0.,0.));
#35973=DIRECTION('center_axis',(-1.,-1.23908819712629E-16,0.));
#35974=DIRECTION('ref_axis',(1.23908819712629E-16,-1.,0.));
#35975=DIRECTION('',(0.,0.,-1.));
#35976=DIRECTION('',(-1.23908819712629E-16,1.,0.));
#35977=DIRECTION('',(0.,0.,-1.));
#35978=DIRECTION('center_axis',(0.,-1.,0.));
#35979=DIRECTION('ref_axis',(0.,0.,-1.));
#35980=DIRECTION('',(0.,0.,-1.));
#35981=DIRECTION('',(-1.,0.,0.));
#35982=DIRECTION('',(0.,0.,-1.));
#35983=DIRECTION('',(-1.,0.,0.));
#35984=DIRECTION('center_axis',(1.,1.23908819712629E-16,0.));
#35985=DIRECTION('ref_axis',(-1.23908819712629E-16,1.,0.));
#35986=DIRECTION('',(0.,-1.,0.));
#35987=DIRECTION('',(0.,0.,-1.));
#35988=DIRECTION('',(1.23908819712629E-16,-1.,0.));
#35989=DIRECTION('center_axis',(0.,1.,0.));
#35990=DIRECTION('ref_axis',(0.,0.,1.));
#35991=DIRECTION('',(1.,0.,0.));
#35992=DIRECTION('',(0.,0.,1.));
#35993=DIRECTION('',(1.,0.,0.));
#35994=DIRECTION('center_axis',(0.,0.,1.));
#35995=DIRECTION('ref_axis',(1.,0.,0.));
#35996=DIRECTION('center_axis',(1.,0.,0.));
#35997=DIRECTION('ref_axis',(0.,0.,-1.));
#35998=DIRECTION('',(0.,-1.,0.));
#35999=DIRECTION('center_axis',(0.,0.,-1.));
#36000=DIRECTION('ref_axis',(-1.,0.,0.));
#36001=DIRECTION('axis',(0.,0.,1.));
#36002=DIRECTION('refdir',(1.,0.,0.));
#36003=DIRECTION('center_axis',(1.,1.22464679914735E-16,0.));
#36004=DIRECTION('ref_axis',(-1.22464679914735E-16,1.,0.));
#36005=DIRECTION('center_axis',(1.,1.22464679914735E-16,0.));
#36006=DIRECTION('ref_axis',(-1.22464679914735E-16,1.,0.));
#36007=DIRECTION('',(-1.,-1.22464679914735E-16,0.));
#36008=DIRECTION('center_axis',(1.,1.22464679914735E-16,0.));
#36009=DIRECTION('ref_axis',(-1.22464679914735E-16,1.,0.));
#36010=DIRECTION('center_axis',(1.,1.22464679914735E-16,0.));
#36011=DIRECTION('ref_axis',(-1.22464679914735E-16,1.,0.));
#36012=DIRECTION('',(-0.707106781186546,0.707106781186549,8.65956056235495E-17));
#36013=DIRECTION('center_axis',(1.,1.22464679914735E-16,0.));
#36014=DIRECTION('ref_axis',(-1.22464679914735E-16,1.,0.));
#36015=DIRECTION('center_axis',(-1.,-1.22464679914735E-16,0.));
#36016=DIRECTION('ref_axis',(1.22464679914735E-16,-1.,0.));
#36017=DIRECTION('center_axis',(1.,1.22464679914735E-16,0.));
#36018=DIRECTION('ref_axis',(-1.22464679914735E-16,1.,0.));
#36019=DIRECTION('',(0.707106781186552,-0.707106781186543,8.65956056235488E-17));
#36020=DIRECTION('center_axis',(1.,1.22464679914735E-16,0.));
#36021=DIRECTION('ref_axis',(-1.22464679914735E-16,1.,0.));
#36022=DIRECTION('center_axis',(1.,1.22464679914735E-16,0.));
#36023=DIRECTION('ref_axis',(-1.22464679914735E-16,1.,0.));
#36024=DIRECTION('center_axis',(1.,1.22464679914735E-16,0.));
#36025=DIRECTION('ref_axis',(-1.22464679914735E-16,1.,0.));
#36026=DIRECTION('',(-1.,-1.22464679914735E-16,0.));
#36027=DIRECTION('center_axis',(1.,1.22464679914735E-16,0.));
#36028=DIRECTION('ref_axis',(-1.22464679914735E-16,1.,0.));
#36029=DIRECTION('center_axis',(1.,1.22464679914735E-16,0.));
#36030=DIRECTION('ref_axis',(-1.22464679914735E-16,1.,0.));
#36031=DIRECTION('center_axis',(-1.,-1.22464679914735E-16,0.));
#36032=DIRECTION('ref_axis',(1.22464679914735E-16,-1.,0.));
#36033=DIRECTION('',(0.,0.5,-0.866025403784439));
#36034=DIRECTION('',(0.,1.,0.));
#36035=DIRECTION('',(0.,0.5,0.866025403784439));
#36036=DIRECTION('',(0.,-0.5,0.866025403784438));
#36037=DIRECTION('',(0.,-1.,-1.50231459873716E-16));
#36038=DIRECTION('',(0.,-0.5,-0.866025403784439));
#36039=DIRECTION('center_axis',(1.,1.22464679914735E-16,0.));
#36040=DIRECTION('ref_axis',(-1.22464679914735E-16,1.,0.));
#36041=DIRECTION('center_axis',(-1.06057523872491E-16,0.866025403784439,
0.5));
#36042=DIRECTION('ref_axis',(-5.09861652542584E-33,-0.5,0.866025403784439));
#36043=DIRECTION('',(-1.,-1.22464679914735E-16,0.));
#36044=DIRECTION('',(0.,0.5,-0.866025403784439));
#36045=DIRECTION('',(-1.,-1.22464679914735E-16,0.));
#36046=DIRECTION('center_axis',(0.,0.,1.));
#36047=DIRECTION('ref_axis',(1.,0.,0.));
#36048=DIRECTION('',(0.,1.,0.));
#36049=DIRECTION('',(-1.,-1.22464679914735E-16,0.));
#36050=DIRECTION('center_axis',(1.06057523872491E-16,-0.866025403784439,
0.5));
#36051=DIRECTION('ref_axis',(-8.4117933897259E-34,-0.5,-0.866025403784439));
#36052=DIRECTION('',(0.,0.5,0.866025403784439));
#36053=DIRECTION('',(-1.,-1.22464679914735E-16,0.));
#36054=DIRECTION('center_axis',(1.06057523872491E-16,-0.866025403784439,
-0.5));
#36055=DIRECTION('ref_axis',(-5.93979586439842E-33,0.5,-0.866025403784439));
#36056=DIRECTION('',(0.,-0.5,0.866025403784438));
#36057=DIRECTION('',(-1.,-1.22464679914735E-16,0.));
#36058=DIRECTION('center_axis',(-1.8398047646558E-32,1.50231459873716E-16,
-1.));
#36059=DIRECTION('ref_axis',(0.,1.,1.50231459873716E-16));
#36060=DIRECTION('',(0.,-1.,-1.50231459873716E-16));
#36061=DIRECTION('',(-1.,-1.22464679914735E-16,0.));
#36062=DIRECTION('center_axis',(-1.06057523872491E-16,0.866025403784439,
-0.5));
#36063=DIRECTION('ref_axis',(2.96989793219921E-33,0.5,0.866025403784439));
#36064=DIRECTION('',(0.,-0.5,-0.866025403784439));
#36065=DIRECTION('center_axis',(-1.,0.,0.));
#36066=DIRECTION('ref_axis',(0.,0.,1.));
#36067=DIRECTION('',(3.7997243633268E-32,-1.,-2.07461678770476E-19));
#36068=DIRECTION('',(1.,3.7997243633268E-32,1.7233846398661E-50));
#36069=DIRECTION('',(-1.,0.,0.));
#36070=DIRECTION('',(0.,0.,1.));
#36071=DIRECTION('',(-7.49068216750752E-96,1.23259516440783E-32,1.));
#36072=DIRECTION('',(-1.,-1.23259516440783E-32,1.51929083932157E-64));
#36073=DIRECTION('',(-2.70504103045227E-16,-1.,1.62437906768329E-18));
#36074=DIRECTION('',(1.,-2.70504103045227E-16,-1.11022302462516E-16));
#36075=DIRECTION('',(0.,0.,1.));
#36076=DIRECTION('',(1.,0.,0.));
#36077=DIRECTION('',(1.,2.77555756156289E-17,4.33010681256471E-29));
#36078=DIRECTION('',(-2.77555756156289E-17,1.,1.22464679914694E-16));
#36079=DIRECTION('',(1.22464679914735E-16,-1.,0.));
#36080=DIRECTION('',(1.,1.22464679914735E-16,-1.22464679914735E-16));
#36081=DIRECTION('',(-7.49068216750752E-96,1.23259516440783E-32,1.));
#36082=DIRECTION('',(-1.,-1.23259516440783E-32,1.51929083932157E-64));
#36083=DIRECTION('',(0.979426759612045,-0.20179995677861,-2.15172294370209E-17));
#36084=DIRECTION('',(3.47582008981007E-18,1.23496263539437E-16,-1.));
#36085=DIRECTION('',(-0.265256786227996,-4.18033547102838E-31,-0.964177803810063));
#36086=DIRECTION('',(-1.18077726124492E-16,1.,3.24845874206225E-17));
#36087=DIRECTION('',(-2.26878616403346E-16,1.,-1.07552855510562E-16));
#36088=DIRECTION('',(4.94957829021997E-16,1.07552855510562E-16,1.));
#36089=DIRECTION('',(1.,-8.42181142532428E-16,-6.07153216591882E-16));
#36090=DIRECTION('',(6.07153216591882E-16,2.28983498828938E-16,1.));
#36091=DIRECTION('',(1.,-2.77555756156289E-16,-4.71844785465694E-16));
#36092=DIRECTION('',(4.71844785465694E-16,-5.55111512312584E-17,1.));
#36093=DIRECTION('',(-5.55111512312578E-17,-1.,5.94074006973841E-17));
#36094=DIRECTION('',(1.,-5.55111512312578E-17,-2.60436363482795E-16));
#36095=DIRECTION('',(0.906448174427449,0.422317069365121,-4.47188413866496E-16));
#36096=DIRECTION('',(-4.94957829021997E-16,3.46944695195347E-18,-1.));
#36097=DIRECTION('',(2.46519032881566E-32,-1.,1.23259516440783E-32));
#36098=DIRECTION('',(1.,2.46519032881566E-32,-2.46519032881566E-32));
#36099=DIRECTION('',(-0.568493171869113,-0.822687980669582,-2.65648809440325E-32));
#36100=DIRECTION('',(-1.00750220222401E-16,6.96203343266639E-17,-1.));
#36101=DIRECTION('',(-1.,0.,0.));
#36102=DIRECTION('',(0.,0.,1.));
#36103=DIRECTION('',(-0.970260862360484,-0.2420616842284,-2.97224983181783E-17));
#36104=DIRECTION('',(-1.01167001938177E-18,1.26844040772007E-16,-1.));
#36105=DIRECTION('',(-0.125965052119064,0.992034679658247,1.21810889615265E-16));
#36106=DIRECTION('',(4.14609915197138E-18,1.23315399874103E-16,-1.));
#36107=DIRECTION('',(-0.265256786227996,-4.18033547102838E-31,-0.964177803810063));
#36108=DIRECTION('',(-1.18077726124492E-16,1.,3.24845874206225E-17));
#36109=DIRECTION('',(-0.265256786227996,-4.18033547102838E-31,-0.964177803810063));
#36110=DIRECTION('',(-1.18077726124492E-16,1.,3.24845874206225E-17));
#36111=DIRECTION('',(-0.265256786227996,-4.18033547102838E-31,-0.964177803810063));
#36112=DIRECTION('',(-1.18077726124492E-16,1.,3.24845874206225E-17));
#36113=DIRECTION('',(-0.265256786227996,-4.18033547102838E-31,-0.964177803810063));
#36114=DIRECTION('',(-1.18077726124492E-16,1.,3.24845874206225E-17));
#36115=DIRECTION('',(-0.265256786227996,-4.18033547102838E-31,-0.964177803810063));
#36116=DIRECTION('',(-1.18077726124492E-16,1.,3.24845874206225E-17));
#36117=DIRECTION('',(-0.265256786227996,-4.18033547102838E-31,-0.964177803810063));
#36118=DIRECTION('',(-1.18077726124492E-16,1.,3.24845874206225E-17));
#36119=DIRECTION('',(-0.265256786227996,-4.18033547102838E-31,-0.964177803810063));
#36120=DIRECTION('',(-1.18077726124492E-16,1.,3.24845874206225E-17));
#36121=DIRECTION('',(-0.265256786227996,-4.18033547102838E-31,-0.964177803810063));
#36122=DIRECTION('',(-1.18077726124492E-16,1.,3.24845874206225E-17));
#36123=DIRECTION('',(-0.265256786227996,-4.18033547102838E-31,-0.964177803810063));
#36124=DIRECTION('',(-1.18077726124492E-16,1.,3.24845874206225E-17));
#36125=DIRECTION('',(-0.265256786227996,-4.18033547102838E-31,-0.964177803810063));
#36126=DIRECTION('',(-1.18077726124492E-16,1.,3.24845874206225E-17));
#36127=DIRECTION('',(-0.265256786227996,-4.18033547102838E-31,-0.964177803810063));
#36128=DIRECTION('',(-1.18077726124492E-16,1.,3.24845874206225E-17));
#36129=DIRECTION('',(-0.265256786227996,-4.18033547102838E-31,-0.964177803810063));
#36130=DIRECTION('',(-1.18077726124492E-16,1.,3.24845874206225E-17));
#36131=DIRECTION('',(-0.265256786227996,-4.18033547102838E-31,-0.964177803810063));
#36132=DIRECTION('',(-1.18077726124492E-16,1.,3.24845874206225E-17));
#36133=DIRECTION('',(-0.265256786227996,-4.18033547102838E-31,-0.964177803810063));
#36134=DIRECTION('',(-1.18077726124492E-16,1.,3.24845874206225E-17));
#36135=DIRECTION('',(-0.265256786227996,-4.18033547102838E-31,-0.964177803810063));
#36136=DIRECTION('',(-1.18077726124492E-16,1.,3.24845874206225E-17));
#36137=DIRECTION('',(-0.265256786227996,-4.18033547102838E-31,-0.964177803810063));
#36138=DIRECTION('',(-1.18077726124492E-16,1.,3.24845874206225E-17));
#36139=DIRECTION('',(-0.265256786227996,-4.18033547102838E-31,-0.964177803810063));
#36140=DIRECTION('',(-1.18077726124492E-16,1.,3.24845874206225E-17));
#36141=DIRECTION('',(-0.265256786227996,-4.18033547102838E-31,-0.964177803810063));
#36142=DIRECTION('',(-1.18077726124492E-16,1.,3.24845874206225E-17));
#36143=DIRECTION('',(-0.265256786227996,-4.18033547102838E-31,-0.964177803810063));
#36144=DIRECTION('',(-1.18077726124492E-16,1.,3.24845874206225E-17));
#36145=DIRECTION('',(-0.265256786227996,-4.18033547102838E-31,-0.964177803810063));
#36146=DIRECTION('',(-1.18077726124492E-16,1.,3.24845874206225E-17));
#36147=DIRECTION('',(-0.265256786227996,-4.18033547102838E-31,-0.964177803810063));
#36148=DIRECTION('',(-1.18077726124492E-16,1.,3.24845874206225E-17));
#36149=DIRECTION('',(-0.265256786227996,-4.18033547102838E-31,-0.964177803810063));
#36150=DIRECTION('',(-1.18077726124492E-16,1.,3.24845874206225E-17));
#36151=DIRECTION('',(-0.508300275208059,-0.861179905840476,-7.77639997832587E-32));
#36152=DIRECTION('',(-1.05464121517756E-16,6.22488305039272E-17,-1.));
#36153=DIRECTION('',(-0.979426759612045,-0.20179995677861,-2.15172294371058E-17));
#36154=DIRECTION('',(-3.47582008972345E-18,1.23496263539437E-16,-1.));
#36155=DIRECTION('',(0.970260862360484,-0.2420616842284,-2.97224983180942E-17));
#36156=DIRECTION('',(1.01167001946839E-18,1.26844040772007E-16,-1.));
#36157=DIRECTION('',(0.125965052119064,0.992034679658247,1.21810889615276E-16));
#36158=DIRECTION('',(-4.14609915188478E-18,1.23315399874103E-16,-1.));
#36159=DIRECTION('',(-0.265256786227996,-4.18033547102838E-31,-0.964177803810063));
#36160=DIRECTION('',(-1.18077726124492E-16,1.,3.24845874206225E-17));
#36161=DIRECTION('',(-2.46519032881566E-32,-1.,1.23259516440783E-32));
#36162=DIRECTION('',(-1.,2.46519032881566E-32,-2.46519032881566E-32));
#36163=DIRECTION('',(-0.265256786227996,-4.18033547102838E-31,-0.964177803810063));
#36164=DIRECTION('',(-1.18077726124492E-16,1.,3.24845874206225E-17));
#36165=DIRECTION('',(-0.265256786227996,-4.18033547102838E-31,-0.964177803810063));
#36166=DIRECTION('',(-1.18077726124492E-16,1.,3.24845874206225E-17));
#36167=DIRECTION('',(-0.265256786227996,-4.18033547102838E-31,-0.964177803810063));
#36168=DIRECTION('',(-1.18077726124492E-16,1.,3.24845874206225E-17));
#36169=DIRECTION('',(-0.265256786227996,-4.18033547102838E-31,-0.964177803810063));
#36170=DIRECTION('',(-1.18077726124492E-16,1.,3.24845874206225E-17));
#36171=DIRECTION('',(-0.265256786227996,-4.18033547102838E-31,-0.964177803810063));
#36172=DIRECTION('',(-1.18077726124492E-16,1.,3.24845874206225E-17));
#36173=DIRECTION('',(-0.265256786227996,-4.18033547102838E-31,-0.964177803810063));
#36174=DIRECTION('',(-1.18077726124492E-16,1.,3.24845874206225E-17));
#36175=CARTESIAN_POINT('',(0.,0.,0.));
#36176=CARTESIAN_POINT('',(0.,0.,0.));
#36177=CARTESIAN_POINT('Origin',(-26.,396.,7.5));
#36178=CARTESIAN_POINT('',(-29.4,396.,-7.5));
#36179=CARTESIAN_POINT('Origin',(-26.,396.,-7.5));
#36180=CARTESIAN_POINT('',(-29.4,396.,7.5));
#36181=CARTESIAN_POINT('',(-29.4,396.,7.5));
#36182=CARTESIAN_POINT('Origin',(-26.,396.,7.5));
#36183=CARTESIAN_POINT('Origin',(26.,396.,7.5));
#36184=CARTESIAN_POINT('',(22.6,396.,-7.5));
#36185=CARTESIAN_POINT('Origin',(26.,396.,-7.5));
#36186=CARTESIAN_POINT('',(22.6,396.,7.5));
#36187=CARTESIAN_POINT('',(22.6,396.,7.5));
#36188=CARTESIAN_POINT('Origin',(26.,396.,7.5));
#36189=CARTESIAN_POINT('Origin',(-12.5,396.,7.5));
#36190=CARTESIAN_POINT('',(-15.5,396.,-7.5));
#36191=CARTESIAN_POINT('Origin',(-12.5,396.,-7.5));
#36192=CARTESIAN_POINT('',(-15.5,396.,7.5));
#36193=CARTESIAN_POINT('',(-15.5,396.,7.5));
#36194=CARTESIAN_POINT('Origin',(-12.5,396.,7.5));
#36195=CARTESIAN_POINT('Origin',(12.5,396.,7.5));
#36196=CARTESIAN_POINT('',(9.50000000000001,396.,-7.5));
#36197=CARTESIAN_POINT('Origin',(12.5,396.,-7.5));
#36198=CARTESIAN_POINT('',(9.50000000000001,396.,7.5));
#36199=CARTESIAN_POINT('',(9.50000000000001,396.,7.5));
#36200=CARTESIAN_POINT('Origin',(12.5,396.,7.5));
#36201=CARTESIAN_POINT('Origin',(150.,-545.,7.5));
#36202=CARTESIAN_POINT('',(150.,-545.,-7.5));
#36203=CARTESIAN_POINT('',(150.,545.,-7.5));
#36204=CARTESIAN_POINT('',(150.,-545.,-7.5));
#36205=CARTESIAN_POINT('',(150.,545.,7.5));
#36206=CARTESIAN_POINT('',(150.,545.,7.5));
#36207=CARTESIAN_POINT('',(150.,-545.,7.5));
#36208=CARTESIAN_POINT('',(150.,-545.,7.5));
#36209=CARTESIAN_POINT('',(150.,-545.,7.5));
#36210=CARTESIAN_POINT('Origin',(-150.,545.,7.5));
#36211=CARTESIAN_POINT('',(-150.,545.,-7.5));
#36212=CARTESIAN_POINT('',(-150.,545.,-7.5));
#36213=CARTESIAN_POINT('',(-150.,545.,7.5));
#36214=CARTESIAN_POINT('',(-150.,545.,7.5));
#36215=CARTESIAN_POINT('',(-150.,545.,7.5));
#36216=CARTESIAN_POINT('Origin',(-150.,-545.,7.5));
#36217=CARTESIAN_POINT('',(-150.,-545.,-7.5));
#36218=CARTESIAN_POINT('',(-150.,-545.,-7.5));
#36219=CARTESIAN_POINT('',(-150.,-545.,7.5));
#36220=CARTESIAN_POINT('',(-150.,-545.,7.5));
#36221=CARTESIAN_POINT('',(-150.,-545.,7.5));
#36222=CARTESIAN_POINT('Origin',(-150.,-545.,7.5));
#36223=CARTESIAN_POINT('',(-150.,-545.,-7.5));
#36224=CARTESIAN_POINT('',(-150.,-545.,7.5));
#36225=CARTESIAN_POINT('Origin',(0.,0.,7.5));
#36226=CARTESIAN_POINT('',(-80.,-300.,7.5));
#36227=CARTESIAN_POINT('',(80.,-300.,7.5));
#36228=CARTESIAN_POINT('',(-80.,-300.,7.5));
#36229=CARTESIAN_POINT('',(-80.,-100.,7.5));
#36230=CARTESIAN_POINT('',(-80.,-100.,7.5));
#36231=CARTESIAN_POINT('',(80.,-100.,7.5));
#36232=CARTESIAN_POINT('',(-80.,-100.,7.5));
#36233=CARTESIAN_POINT('',(80.,-100.,7.5));
#36234=CARTESIAN_POINT('',(-80.,99.9999999999999,7.5));
#36235=CARTESIAN_POINT('',(80.,99.9999999999999,7.5));
#36236=CARTESIAN_POINT('',(-80.,99.9999999999999,7.5));
#36237=CARTESIAN_POINT('',(-80.0000000000001,300.,7.5));
#36238=CARTESIAN_POINT('',(-80.0000000000001,300.,7.5));
#36239=CARTESIAN_POINT('',(79.9999999999999,300.,7.5));
#36240=CARTESIAN_POINT('',(-80.0000000000001,300.,7.5));
#36241=CARTESIAN_POINT('',(79.9999999999999,300.,7.5));
#36242=CARTESIAN_POINT('Origin',(0.,0.,-7.5));
#36243=CARTESIAN_POINT('',(-80.,-100.,-7.5));
#36244=CARTESIAN_POINT('',(-80.,-300.,-7.5));
#36245=CARTESIAN_POINT('',(-80.,-100.,-7.5));
#36246=CARTESIAN_POINT('',(80.,-300.,-7.5));
#36247=CARTESIAN_POINT('',(-80.,-300.,-7.5));
#36248=CARTESIAN_POINT('',(80.,-100.,-7.5));
#36249=CARTESIAN_POINT('',(80.,-100.,-7.5));
#36250=CARTESIAN_POINT('',(-80.,-100.,-7.5));
#36251=CARTESIAN_POINT('',(-80.0000000000001,300.,-7.5));
#36252=CARTESIAN_POINT('',(-80.,99.9999999999999,-7.5));
#36253=CARTESIAN_POINT('',(-80.0000000000001,300.,-7.5));
#36254=CARTESIAN_POINT('',(80.,99.9999999999999,-7.5));
#36255=CARTESIAN_POINT('',(-80.,99.9999999999999,-7.5));
#36256=CARTESIAN_POINT('',(79.9999999999999,300.,-7.5));
#36257=CARTESIAN_POINT('',(79.9999999999999,300.,-7.5));
#36258=CARTESIAN_POINT('',(-80.0000000000001,300.,-7.5));
#36259=CARTESIAN_POINT('Origin',(-80.0000000000001,300.,-7.5));
#36260=CARTESIAN_POINT('',(-80.,99.9999999999999,-7.5));
#36261=CARTESIAN_POINT('',(-80.0000000000001,300.,-7.5));
#36262=CARTESIAN_POINT('Origin',(-80.0000000000001,300.,-7.5));
#36263=CARTESIAN_POINT('',(79.9999999999999,300.,-7.5));
#36264=CARTESIAN_POINT('Origin',(79.9999999999999,300.,-7.5));
#36265=CARTESIAN_POINT('',(80.,99.9999999999999,-7.5));
#36266=CARTESIAN_POINT('Origin',(-80.,99.9999999999999,-7.5));
#36267=CARTESIAN_POINT('Origin',(-80.,-100.,-7.5));
#36268=CARTESIAN_POINT('',(-80.,-300.,-7.5));
#36269=CARTESIAN_POINT('',(-80.,-100.,-7.5));
#36270=CARTESIAN_POINT('Origin',(-80.,-100.,-7.5));
#36271=CARTESIAN_POINT('',(80.,-100.,-7.5));
#36272=CARTESIAN_POINT('Origin',(80.,-100.,-7.5));
#36273=CARTESIAN_POINT('',(80.,-300.,-7.5));
#36274=CARTESIAN_POINT('Origin',(-80.,-300.,-7.5));
#36275=CARTESIAN_POINT('',(0.,0.,0.));
#36276=CARTESIAN_POINT('',(0.,0.,0.));
#36277=CARTESIAN_POINT('Origin',(-13.5,0.5,1.));
#36278=CARTESIAN_POINT('',(-16.5,0.5,-4.));
#36279=CARTESIAN_POINT('Origin',(-13.5,0.5,-4.));
#36280=CARTESIAN_POINT('',(-16.5,0.5,1.));
#36281=CARTESIAN_POINT('',(-16.5,0.5,1.));
#36282=CARTESIAN_POINT('Origin',(-13.5,0.5,1.));
#36283=CARTESIAN_POINT('Origin',(11.5,0.5,1.));
#36284=CARTESIAN_POINT('',(8.5,0.5,-4.));
#36285=CARTESIAN_POINT('Origin',(11.5,0.5,-4.));
#36286=CARTESIAN_POINT('',(8.5,0.5,1.));
#36287=CARTESIAN_POINT('',(8.5,0.5,1.));
#36288=CARTESIAN_POINT('Origin',(11.5,0.5,1.));
#36289=CARTESIAN_POINT('Origin',(-27.,0.5,-4.));
#36290=CARTESIAN_POINT('',(-31.25,0.499999999999999,-4.));
#36291=CARTESIAN_POINT('Origin',(-27.,0.5,-4.));
#36292=CARTESIAN_POINT('',(-31.25,0.499999999999999,1.));
#36293=CARTESIAN_POINT('',(-31.25,0.499999999999999,-4.));
#36294=CARTESIAN_POINT('Origin',(-27.,0.5,1.));
#36295=CARTESIAN_POINT('Origin',(25.,0.5,-4.));
#36296=CARTESIAN_POINT('',(20.75,0.499999999999999,-4.));
#36297=CARTESIAN_POINT('Origin',(25.,0.5,-4.));
#36298=CARTESIAN_POINT('',(20.75,0.499999999999999,1.));
#36299=CARTESIAN_POINT('',(20.75,0.499999999999999,-4.));
#36300=CARTESIAN_POINT('Origin',(25.,0.5,1.));
#36301=CARTESIAN_POINT('Origin',(0.,0.,4.));
#36302=CARTESIAN_POINT('',(34.,-1.5,4.));
#36303=CARTESIAN_POINT('',(34.,11.5,4.));
#36304=CARTESIAN_POINT('',(34.,11.5,4.));
#36305=CARTESIAN_POINT('',(36.5,-1.5,4.));
#36306=CARTESIAN_POINT('',(34.,-1.5,4.));
#36307=CARTESIAN_POINT('',(36.5,11.5,4.));
#36308=CARTESIAN_POINT('',(36.5,11.5,4.));
#36309=CARTESIAN_POINT('',(-36.5,11.5,4.));
#36310=CARTESIAN_POINT('Origin',(36.5,11.5,4.));
#36311=CARTESIAN_POINT('',(36.5,-1.5,1.));
#36312=CARTESIAN_POINT('',(36.5,-1.5,1.));
#36313=CARTESIAN_POINT('',(36.5,-11.5,1.));
#36314=CARTESIAN_POINT('',(36.5,-11.5,1.));
#36315=CARTESIAN_POINT('',(36.5,-11.5,-4.));
#36316=CARTESIAN_POINT('',(36.5,-11.5,4.));
#36317=CARTESIAN_POINT('',(36.5,11.5,-4.));
#36318=CARTESIAN_POINT('',(36.5,11.5,-4.));
#36319=CARTESIAN_POINT('',(36.5,11.5,4.));
#36320=CARTESIAN_POINT('Origin',(-36.5,11.5,4.));
#36321=CARTESIAN_POINT('',(34.,11.5,1.));
#36322=CARTESIAN_POINT('',(-36.5,11.5,1.));
#36323=CARTESIAN_POINT('',(-36.5,11.5,1.));
#36324=CARTESIAN_POINT('',(34.,11.5,1.));
#36325=CARTESIAN_POINT('',(-36.5,11.5,-4.));
#36326=CARTESIAN_POINT('',(-36.5,11.5,-4.));
#36327=CARTESIAN_POINT('',(-36.5,11.5,4.));
#36328=CARTESIAN_POINT('Origin',(-36.5,11.5,4.));
#36329=CARTESIAN_POINT('',(-36.5,-9.5,4.));
#36330=CARTESIAN_POINT('',(-36.5,-11.5,4.));
#36331=CARTESIAN_POINT('',(-36.5,11.5,4.));
#36332=CARTESIAN_POINT('',(-36.5,-9.5,1.));
#36333=CARTESIAN_POINT('',(-36.5,-9.5,1.));
#36334=CARTESIAN_POINT('',(-36.5,11.5,1.));
#36335=CARTESIAN_POINT('',(-36.5,-11.5,-4.));
#36336=CARTESIAN_POINT('',(-36.5,11.5,-4.));
#36337=CARTESIAN_POINT('',(-36.5,-11.5,4.));
#36338=CARTESIAN_POINT('Origin',(-36.5,-11.5,4.));
#36339=CARTESIAN_POINT('',(16.5,-11.5,1.));
#36340=CARTESIAN_POINT('',(16.5,-11.5,1.));
#36341=CARTESIAN_POINT('',(16.5,-11.5,4.));
#36342=CARTESIAN_POINT('',(16.5,-11.5,1.));
#36343=CARTESIAN_POINT('',(-36.5,-11.5,4.));
#36344=CARTESIAN_POINT('',(-36.5,-11.5,-4.));
#36345=CARTESIAN_POINT('Origin',(0.,0.,4.));
#36346=CARTESIAN_POINT('',(16.5,-9.5,4.));
#36347=CARTESIAN_POINT('',(16.5,-9.5,4.));
#36348=CARTESIAN_POINT('',(-36.5,-9.5,4.));
#36349=CARTESIAN_POINT('Origin',(0.,0.,-4.));
#36350=CARTESIAN_POINT('Origin',(34.,11.5,1.));
#36351=CARTESIAN_POINT('',(34.,-1.5,1.));
#36352=CARTESIAN_POINT('',(34.,11.5,1.));
#36353=CARTESIAN_POINT('',(34.,-1.5,1.));
#36354=CARTESIAN_POINT('Origin',(34.,-1.5,1.));
#36355=CARTESIAN_POINT('',(34.,-1.5,1.));
#36356=CARTESIAN_POINT('Origin',(16.5,-9.5,1.));
#36357=CARTESIAN_POINT('',(16.5,-9.5,1.));
#36358=CARTESIAN_POINT('',(16.5,-9.5,1.));
#36359=CARTESIAN_POINT('',(16.5,-9.5,1.));
#36360=CARTESIAN_POINT('Origin',(-36.5,-9.5,1.));
#36361=CARTESIAN_POINT('',(-36.5,-9.5,1.));
#36362=CARTESIAN_POINT('Origin',(0.,0.,1.));
#36363=CARTESIAN_POINT('',(0.,0.,0.));
#36364=CARTESIAN_POINT('Origin',(31.819805153395,29.3198051533945,5.));
#36365=CARTESIAN_POINT('',(29.719805153395,29.3198051533945,-5.));
#36366=CARTESIAN_POINT('Origin',(31.819805153395,29.3198051533945,-5.));
#36367=CARTESIAN_POINT('',(29.719805153395,29.3198051533945,5.));
#36368=CARTESIAN_POINT('',(29.719805153395,29.3198051533945,5.));
#36369=CARTESIAN_POINT('Origin',(31.819805153395,29.3198051533945,5.));
#36370=CARTESIAN_POINT('Origin',(-31.8198051533946,29.319805153395,5.));
#36371=CARTESIAN_POINT('',(-33.9198051533946,29.319805153395,-5.));
#36372=CARTESIAN_POINT('Origin',(-31.8198051533946,29.319805153395,-5.));
#36373=CARTESIAN_POINT('',(-33.9198051533946,29.319805153395,5.));
#36374=CARTESIAN_POINT('',(-33.9198051533946,29.319805153395,5.));
#36375=CARTESIAN_POINT('Origin',(-31.8198051533946,29.319805153395,5.));
#36376=CARTESIAN_POINT('Origin',(-31.8198051533948,-34.3198051533942,5.));
#36377=CARTESIAN_POINT('',(-33.9198051533948,-34.3198051533942,-5.));
#36378=CARTESIAN_POINT('Origin',(-31.8198051533948,-34.3198051533942,-5.));
#36379=CARTESIAN_POINT('',(-33.9198051533948,-34.3198051533942,5.));
#36380=CARTESIAN_POINT('',(-33.9198051533948,-34.3198051533942,5.));
#36381=CARTESIAN_POINT('Origin',(-31.8198051533948,-34.3198051533942,5.));
#36382=CARTESIAN_POINT('Origin',(31.8198051533946,-34.3198051533944,5.));
#36383=CARTESIAN_POINT('',(29.7198051533946,-34.3198051533944,-5.));
#36384=CARTESIAN_POINT('Origin',(31.8198051533946,-34.3198051533944,-5.));
#36385=CARTESIAN_POINT('',(29.7198051533946,-34.3198051533944,5.));
#36386=CARTESIAN_POINT('',(29.7198051533946,-34.3198051533944,5.));
#36387=CARTESIAN_POINT('Origin',(31.8198051533946,-34.3198051533944,5.));
#36388=CARTESIAN_POINT('Origin',(-10.,35.,5.));
#36389=CARTESIAN_POINT('',(-13.,35.,-5.));
#36390=CARTESIAN_POINT('Origin',(-10.,35.,-5.));
#36391=CARTESIAN_POINT('',(-13.,35.,5.));
#36392=CARTESIAN_POINT('',(-13.,35.,5.));
#36393=CARTESIAN_POINT('Origin',(-10.,35.,5.));
#36394=CARTESIAN_POINT('Origin',(10.,35.,5.));
#36395=CARTESIAN_POINT('',(7.,35.,-5.));
#36396=CARTESIAN_POINT('Origin',(10.,35.,-5.));
#36397=CARTESIAN_POINT('',(7.,35.,5.));
#36398=CARTESIAN_POINT('',(7.,35.,5.));
#36399=CARTESIAN_POINT('Origin',(10.,35.,5.));
#36400=CARTESIAN_POINT('Origin',(-24.,35.,5.));
#36401=CARTESIAN_POINT('',(-29.5,35.,-1.4));
#36402=CARTESIAN_POINT('Origin',(-24.,35.,-1.4));
#36403=CARTESIAN_POINT('',(-29.5,35.,5.));
#36404=CARTESIAN_POINT('',(-29.5,35.,5.));
#36405=CARTESIAN_POINT('Origin',(-24.,35.,5.));
#36406=CARTESIAN_POINT('Origin',(-24.,35.,5.));
#36407=CARTESIAN_POINT('',(-27.3,35.,-5.));
#36408=CARTESIAN_POINT('Origin',(-24.,35.,-5.));
#36409=CARTESIAN_POINT('',(-27.3,35.,-1.4));
#36410=CARTESIAN_POINT('',(-27.3,35.,5.));
#36411=CARTESIAN_POINT('Origin',(-24.,35.,-1.4));
#36412=CARTESIAN_POINT('Origin',(24.,35.,5.));
#36413=CARTESIAN_POINT('',(18.5,35.,-1.4));
#36414=CARTESIAN_POINT('Origin',(24.,35.,-1.4));
#36415=CARTESIAN_POINT('',(18.5,35.,5.));
#36416=CARTESIAN_POINT('',(18.5,35.,5.));
#36417=CARTESIAN_POINT('Origin',(24.,35.,5.));
#36418=CARTESIAN_POINT('Origin',(24.,35.,5.));
#36419=CARTESIAN_POINT('',(20.7,35.,-5.));
#36420=CARTESIAN_POINT('Origin',(24.,35.,-5.));
#36421=CARTESIAN_POINT('',(20.7,35.,-1.4));
#36422=CARTESIAN_POINT('',(20.7,35.,5.));
#36423=CARTESIAN_POINT('Origin',(24.,35.,-1.4));
#36424=CARTESIAN_POINT('Origin',(-1.20882209737476E-14,-2.49999999999972,
-5.));
#36425=CARTESIAN_POINT('',(-17.5,-2.49999999999972,-5.));
#36426=CARTESIAN_POINT('Origin',(-1.20882209737476E-14,-2.49999999999972,
-5.));
#36427=CARTESIAN_POINT('',(-17.5,-2.49999999999972,1.));
#36428=CARTESIAN_POINT('',(-17.5,-2.49999999999972,-5.));
#36429=CARTESIAN_POINT('Origin',(-1.20882209737476E-14,-2.49999999999972,
1.));
#36430=CARTESIAN_POINT('Origin',(-1.20882209737476E-14,-2.49999999999972,
1.));
#36431=CARTESIAN_POINT('',(-35.,-2.49999999999972,1.));
#36432=CARTESIAN_POINT('Origin',(-1.20882209737476E-14,-2.49999999999972,
1.));
#36433=CARTESIAN_POINT('',(-35.,-2.49999999999972,5.));
#36434=CARTESIAN_POINT('',(-35.,-2.49999999999972,1.));
#36435=CARTESIAN_POINT('Origin',(-1.20882209737476E-14,-2.49999999999972,
5.));
#36436=CARTESIAN_POINT('Origin',(0.,0.,-5.));
#36437=CARTESIAN_POINT('',(52.5,-55.,-5.));
#36438=CARTESIAN_POINT('',(52.5,55.,-5.));
#36439=CARTESIAN_POINT('',(52.5,-55.,-5.));
#36440=CARTESIAN_POINT('',(-52.5,-55.,-5.));
#36441=CARTESIAN_POINT('',(-52.5,-55.,-5.));
#36442=CARTESIAN_POINT('',(-52.5,55.,-5.));
#36443=CARTESIAN_POINT('',(-52.5,-55.,-5.));
#36444=CARTESIAN_POINT('',(-52.5,55.,-5.));
#36445=CARTESIAN_POINT('Origin',(52.5,-55.,5.));
#36446=CARTESIAN_POINT('',(52.5,55.,5.));
#36447=CARTESIAN_POINT('',(52.5,55.,5.));
#36448=CARTESIAN_POINT('',(52.5,-55.,5.));
#36449=CARTESIAN_POINT('',(52.5,-55.,5.));
#36450=CARTESIAN_POINT('',(52.5,-55.,5.));
#36451=CARTESIAN_POINT('Origin',(-52.5,55.,5.));
#36452=CARTESIAN_POINT('',(-52.5,55.,5.));
#36453=CARTESIAN_POINT('',(-52.5,55.,5.));
#36454=CARTESIAN_POINT('',(-52.5,55.,5.));
#36455=CARTESIAN_POINT('Origin',(-52.5,-55.,5.));
#36456=CARTESIAN_POINT('',(-52.5,-55.,5.));
#36457=CARTESIAN_POINT('',(-52.5,-55.,5.));
#36458=CARTESIAN_POINT('',(-52.5,-55.,5.));
#36459=CARTESIAN_POINT('Origin',(-52.5,-55.,5.));
#36460=CARTESIAN_POINT('',(-52.5,-55.,5.));
#36461=CARTESIAN_POINT('Origin',(0.,0.,5.));
#36462=CARTESIAN_POINT('Origin',(-1.20882209737476E-14,-2.49999999999972,
1.));
#36463=CARTESIAN_POINT('Origin',(27.3,35.,-1.4));
#36464=CARTESIAN_POINT('Origin',(-20.7,35.,-1.4));
#36465=CARTESIAN_POINT('',(0.,0.,0.));
#36466=CARTESIAN_POINT('',(0.,0.,0.));
#36467=CARTESIAN_POINT('Origin',(-6.61700935788389,-7.,16.6170093578838));
#36468=CARTESIAN_POINT('',(-6.61700935788389,7.,18.7170093578838));
#36469=CARTESIAN_POINT('Origin',(-6.61700935788389,7.,16.6170093578838));
#36470=CARTESIAN_POINT('',(-6.61700935788389,-7.,18.7170093578838));
#36471=CARTESIAN_POINT('',(-6.61700935788389,-7.,18.7170093578838));
#36472=CARTESIAN_POINT('Origin',(-6.61700935788389,-7.,16.6170093578838));
#36473=CARTESIAN_POINT('Origin',(10.,-7.,23.5));
#36474=CARTESIAN_POINT('',(10.,7.,25.6));
#36475=CARTESIAN_POINT('Origin',(10.,7.,23.5));
#36476=CARTESIAN_POINT('',(10.,-7.,25.6));
#36477=CARTESIAN_POINT('',(10.,-7.,25.6));
#36478=CARTESIAN_POINT('Origin',(10.,-7.,23.5));
#36479=CARTESIAN_POINT('Origin',(26.6170093578838,-7.,16.617009357884));
#36480=CARTESIAN_POINT('',(26.6170093578838,7.,18.7170093578839));
#36481=CARTESIAN_POINT('Origin',(26.6170093578838,7.,16.617009357884));
#36482=CARTESIAN_POINT('',(26.6170093578838,-7.,18.7170093578839));
#36483=CARTESIAN_POINT('',(26.6170093578838,-7.,18.7170093578839));
#36484=CARTESIAN_POINT('Origin',(26.6170093578838,-7.,16.617009357884));
#36485=CARTESIAN_POINT('Origin',(-6.61700935788389,-7.,-16.6170093578838));
#36486=CARTESIAN_POINT('',(-6.61700935788389,7.,-14.5170093578838));
#36487=CARTESIAN_POINT('Origin',(-6.61700935788389,7.,-16.6170093578838));
#36488=CARTESIAN_POINT('',(-6.61700935788389,-7.,-14.5170093578838));
#36489=CARTESIAN_POINT('',(-6.61700935788389,-7.,-14.5170093578838));
#36490=CARTESIAN_POINT('Origin',(-6.61700935788389,-7.,-16.6170093578838));
#36491=CARTESIAN_POINT('Origin',(10.,-7.,-23.5));
#36492=CARTESIAN_POINT('',(10.,7.,-21.4));
#36493=CARTESIAN_POINT('Origin',(10.,7.,-23.5));
#36494=CARTESIAN_POINT('',(10.,-7.,-21.4));
#36495=CARTESIAN_POINT('',(10.,-7.,-21.4));
#36496=CARTESIAN_POINT('Origin',(10.,-7.,-23.5));
#36497=CARTESIAN_POINT('Origin',(26.6170093578838,-7.,-16.617009357884));
#36498=CARTESIAN_POINT('',(26.6170093578838,7.,-14.517009357884));
#36499=CARTESIAN_POINT('Origin',(26.6170093578838,7.,-16.617009357884));
#36500=CARTESIAN_POINT('',(26.6170093578838,-7.,-14.517009357884));
#36501=CARTESIAN_POINT('',(26.6170093578838,-7.,-14.517009357884));
#36502=CARTESIAN_POINT('Origin',(26.6170093578838,-7.,-16.617009357884));
#36503=CARTESIAN_POINT('Origin',(10.,7.,0.));
#36504=CARTESIAN_POINT('',(10.,7.,18.));
#36505=CARTESIAN_POINT('Origin',(10.,7.,0.));
#36506=CARTESIAN_POINT('',(10.,-7.,18.));
#36507=CARTESIAN_POINT('',(10.,7.,18.));
#36508=CARTESIAN_POINT('Origin',(10.,-7.,0.));
#36509=CARTESIAN_POINT('Origin',(-32.,-7.,27.5));
#36510=CARTESIAN_POINT('',(32.,-7.,17.5));
#36511=CARTESIAN_POINT('',(32.,-7.,-17.5));
#36512=CARTESIAN_POINT('',(32.,-7.,27.5));
#36513=CARTESIAN_POINT('',(22.,-7.,27.5));
#36514=CARTESIAN_POINT('Origin',(22.,-7.,17.5));
#36515=CARTESIAN_POINT('',(-32.,-7.,27.5));
#36516=CARTESIAN_POINT('',(-32.,-7.,27.5));
#36517=CARTESIAN_POINT('',(-32.,-7.,-27.5));
#36518=CARTESIAN_POINT('',(-32.,-7.,27.5));
#36519=CARTESIAN_POINT('',(22.,-7.,-27.5));
#36520=CARTESIAN_POINT('',(-32.,-7.,-27.5));
#36521=CARTESIAN_POINT('Origin',(22.,-7.,-17.5));
#36522=CARTESIAN_POINT('Origin',(32.,-7.,27.5));
#36523=CARTESIAN_POINT('',(32.,7.,17.5));
#36524=CARTESIAN_POINT('',(32.,7.,-17.5));
#36525=CARTESIAN_POINT('',(32.,7.,27.5));
#36526=CARTESIAN_POINT('',(32.,-7.,17.5));
#36527=CARTESIAN_POINT('',(32.,7.,-17.5));
#36528=CARTESIAN_POINT('Origin',(-32.,7.,27.5));
#36529=CARTESIAN_POINT('',(22.,7.,27.5));
#36530=CARTESIAN_POINT('',(-32.,7.,27.5));
#36531=CARTESIAN_POINT('',(-32.,7.,27.5));
#36532=CARTESIAN_POINT('Origin',(22.,7.,17.5));
#36533=CARTESIAN_POINT('',(22.,7.,-27.5));
#36534=CARTESIAN_POINT('Origin',(22.,7.,-17.5));
#36535=CARTESIAN_POINT('',(-32.,7.,-27.5));
#36536=CARTESIAN_POINT('',(-32.,7.,-27.5));
#36537=CARTESIAN_POINT('',(-32.,7.,27.5));
#36538=CARTESIAN_POINT('Origin',(-32.,-7.,27.5));
#36539=CARTESIAN_POINT('',(-32.,-7.,-27.5));
#36540=CARTESIAN_POINT('',(-32.,-7.,27.5));
#36541=CARTESIAN_POINT('Origin',(0.,0.,27.5));
#36542=CARTESIAN_POINT('',(22.,0.,27.5));
#36543=CARTESIAN_POINT('Origin',(0.,0.,-27.5));
#36544=CARTESIAN_POINT('',(22.,-7.,-27.5));
#36545=CARTESIAN_POINT('Origin',(22.,0.,17.5));
#36546=CARTESIAN_POINT('Origin',(22.,-7.,-17.5));
#36547=CARTESIAN_POINT('',(0.,0.,0.));
#36548=CARTESIAN_POINT('Origin',(-20.,33.,5.));
#36549=CARTESIAN_POINT('',(-23.,33.,-5.));
#36550=CARTESIAN_POINT('Origin',(-20.,33.,-5.));
#36551=CARTESIAN_POINT('',(-23.,33.,5.));
#36552=CARTESIAN_POINT('',(-23.,33.,5.));
#36553=CARTESIAN_POINT('Origin',(-20.,33.,5.));
#36554=CARTESIAN_POINT('Origin',(20.,-33.,5.));
#36555=CARTESIAN_POINT('',(17.,-33.,-5.));
#36556=CARTESIAN_POINT('Origin',(20.,-33.,-5.));
#36557=CARTESIAN_POINT('',(17.,-33.,5.));
#36558=CARTESIAN_POINT('',(17.,-33.,5.));
#36559=CARTESIAN_POINT('Origin',(20.,-33.,5.));
#36560=CARTESIAN_POINT('Origin',(40.,33.,5.));
#36561=CARTESIAN_POINT('',(36.7,33.,-5.));
#36562=CARTESIAN_POINT('Origin',(40.,33.,-5.));
#36563=CARTESIAN_POINT('',(36.7,33.,5.));
#36564=CARTESIAN_POINT('',(36.7,33.,5.));
#36565=CARTESIAN_POINT('Origin',(40.,33.,5.));
#36566=CARTESIAN_POINT('Origin',(-40.,33.,5.));
#36567=CARTESIAN_POINT('',(-43.3,33.,-5.));
#36568=CARTESIAN_POINT('Origin',(-40.,33.,-5.));
#36569=CARTESIAN_POINT('',(-43.3,33.,5.));
#36570=CARTESIAN_POINT('',(-43.3,33.,5.));
#36571=CARTESIAN_POINT('Origin',(-40.,33.,5.));
#36572=CARTESIAN_POINT('Origin',(-40.,-33.,5.));
#36573=CARTESIAN_POINT('',(-43.3,-33.,-5.));
#36574=CARTESIAN_POINT('Origin',(-40.,-33.,-5.));
#36575=CARTESIAN_POINT('',(-43.3,-33.,5.));
#36576=CARTESIAN_POINT('',(-43.3,-33.,5.));
#36577=CARTESIAN_POINT('Origin',(-40.,-33.,5.));
#36578=CARTESIAN_POINT('Origin',(40.,-33.,5.));
#36579=CARTESIAN_POINT('',(36.7,-33.,-5.));
#36580=CARTESIAN_POINT('Origin',(40.,-33.,-5.));
#36581=CARTESIAN_POINT('',(36.7,-33.,5.));
#36582=CARTESIAN_POINT('',(36.7,-33.,5.));
#36583=CARTESIAN_POINT('Origin',(40.,-33.,5.));
#36584=CARTESIAN_POINT('Origin',(55.,47.5,5.));
#36585=CARTESIAN_POINT('',(55.,-47.5,-5.));
#36586=CARTESIAN_POINT('',(55.,47.5,-5.));
#36587=CARTESIAN_POINT('',(55.,47.5,-5.));
#36588=CARTESIAN_POINT('',(55.,47.5,5.));
#36589=CARTESIAN_POINT('',(55.,47.5,5.));
#36590=CARTESIAN_POINT('',(55.,-47.5,5.));
#36591=CARTESIAN_POINT('',(55.,47.5,5.));
#36592=CARTESIAN_POINT('',(55.,-47.5,5.));
#36593=CARTESIAN_POINT('Origin',(-55.,47.5,5.));
#36594=CARTESIAN_POINT('',(-55.,47.5,-5.));
#36595=CARTESIAN_POINT('',(-55.,47.5,-5.));
#36596=CARTESIAN_POINT('',(-55.,47.5,5.));
#36597=CARTESIAN_POINT('',(-55.,47.5,5.));
#36598=CARTESIAN_POINT('',(-55.,47.5,5.));
#36599=CARTESIAN_POINT('Origin',(-55.,47.5,5.));
#36600=CARTESIAN_POINT('',(-55.,-47.5,-5.));
#36601=CARTESIAN_POINT('',(-55.,47.5,-5.));
#36602=CARTESIAN_POINT('',(-55.,-47.5,5.));
#36603=CARTESIAN_POINT('',(-55.,-47.5,5.));
#36604=CARTESIAN_POINT('',(-55.,47.5,5.));
#36605=CARTESIAN_POINT('Origin',(-55.,-47.5,5.));
#36606=CARTESIAN_POINT('',(-55.,-47.5,-5.));
#36607=CARTESIAN_POINT('',(-55.,-47.5,5.));
#36608=CARTESIAN_POINT('Origin',(0.,0.,5.));
#36609=CARTESIAN_POINT('Origin',(0.,0.,-5.));
#36610=CARTESIAN_POINT('',(0.,0.,0.));
#36611=CARTESIAN_POINT('',(-37.,1.38777878078145E-14,4.73545521495534E-16));
#36612=CARTESIAN_POINT('',(0.,0.,0.));
#36613=CARTESIAN_POINT('Origin',(40.,33.,2.5));
#36614=CARTESIAN_POINT('',(36.7,33.,-2.5));
#36615=CARTESIAN_POINT('Origin',(40.,33.,-2.5));
#36616=CARTESIAN_POINT('',(36.7,33.,2.5));
#36617=CARTESIAN_POINT('',(36.7,33.,2.5));
#36618=CARTESIAN_POINT('Origin',(40.,33.,2.5));
#36619=CARTESIAN_POINT('Origin',(-40.,33.,2.5));
#36620=CARTESIAN_POINT('',(-43.3,33.,-2.5));
#36621=CARTESIAN_POINT('Origin',(-40.,33.,-2.5));
#36622=CARTESIAN_POINT('',(-43.3,33.,2.5));
#36623=CARTESIAN_POINT('',(-43.3,33.,2.5));
#36624=CARTESIAN_POINT('Origin',(-40.,33.,2.5));
#36625=CARTESIAN_POINT('Origin',(-40.,-33.,2.5));
#36626=CARTESIAN_POINT('',(-43.3,-33.,-2.5));
#36627=CARTESIAN_POINT('Origin',(-40.,-33.,-2.5));
#36628=CARTESIAN_POINT('',(-43.3,-33.,2.5));
#36629=CARTESIAN_POINT('',(-43.3,-33.,2.5));
#36630=CARTESIAN_POINT('Origin',(-40.,-33.,2.5));
#36631=CARTESIAN_POINT('Origin',(40.,-33.,2.5));
#36632=CARTESIAN_POINT('',(36.7,-33.,-2.5));
#36633=CARTESIAN_POINT('Origin',(40.,-33.,-2.5));
#36634=CARTESIAN_POINT('',(36.7,-33.,2.5));
#36635=CARTESIAN_POINT('',(36.7,-33.,2.5));
#36636=CARTESIAN_POINT('Origin',(40.,-33.,2.5));
#36637=CARTESIAN_POINT('Origin',(-20.,33.,2.5));
#36638=CARTESIAN_POINT('',(-23.3,33.,-2.5));
#36639=CARTESIAN_POINT('Origin',(-20.,33.,-2.5));
#36640=CARTESIAN_POINT('',(-23.3,33.,2.5));
#36641=CARTESIAN_POINT('',(-23.3,33.,2.5));
#36642=CARTESIAN_POINT('Origin',(-20.,33.,2.5));
#36643=CARTESIAN_POINT('Origin',(20.,-33.,2.5));
#36644=CARTESIAN_POINT('',(16.7,-33.,-2.5));
#36645=CARTESIAN_POINT('Origin',(20.,-33.,-2.5));
#36646=CARTESIAN_POINT('',(16.7,-33.,2.5));
#36647=CARTESIAN_POINT('',(16.7,-33.,2.5));
#36648=CARTESIAN_POINT('Origin',(20.,-33.,2.5));
#36649=CARTESIAN_POINT('Origin',(65.,55.,2.5));
#36650=CARTESIAN_POINT('',(65.,-55.,-2.5));
#36651=CARTESIAN_POINT('',(65.,55.,-2.5));
#36652=CARTESIAN_POINT('',(65.,55.,-2.5));
#36653=CARTESIAN_POINT('',(65.,55.,2.5));
#36654=CARTESIAN_POINT('',(65.,55.,2.5));
#36655=CARTESIAN_POINT('',(65.,-55.,2.5));
#36656=CARTESIAN_POINT('',(65.,55.,2.5));
#36657=CARTESIAN_POINT('',(65.,-55.,2.5));
#36658=CARTESIAN_POINT('Origin',(-65.,55.,2.5));
#36659=CARTESIAN_POINT('',(-65.,55.,-2.5));
#36660=CARTESIAN_POINT('',(-65.,55.,-2.5));
#36661=CARTESIAN_POINT('',(-65.,55.,2.5));
#36662=CARTESIAN_POINT('',(-65.,55.,2.5));
#36663=CARTESIAN_POINT('',(-65.,55.,2.5));
#36664=CARTESIAN_POINT('Origin',(-65.,55.,2.5));
#36665=CARTESIAN_POINT('',(-65.,-55.,-2.5));
#36666=CARTESIAN_POINT('',(-65.,55.,-2.5));
#36667=CARTESIAN_POINT('',(-65.,-55.,2.5));
#36668=CARTESIAN_POINT('',(-65.,-55.,2.5));
#36669=CARTESIAN_POINT('',(-65.,55.,2.5));
#36670=CARTESIAN_POINT('Origin',(-65.,-55.,2.5));
#36671=CARTESIAN_POINT('',(-65.,-55.,-2.5));
#36672=CARTESIAN_POINT('',(-65.,-55.,2.5));
#36673=CARTESIAN_POINT('Origin',(0.,0.,2.5));
#36674=CARTESIAN_POINT('Origin',(0.,0.,-2.5));
#36675=CARTESIAN_POINT('',(0.,0.,0.));
#36676=CARTESIAN_POINT('',(0.,0.,0.));
#36677=CARTESIAN_POINT('Origin',(0.,22.,-840.));
#36678=CARTESIAN_POINT('',(-6.73555739531038E-16,13.,-845.5));
#36679=CARTESIAN_POINT('Origin',(0.,13.,-840.));
#36680=CARTESIAN_POINT('',(-6.73555739531038E-16,22.,-845.5));
#36681=CARTESIAN_POINT('',(-6.73555739531038E-16,22.,-845.5));
#36682=CARTESIAN_POINT('Origin',(0.,22.,-840.));
#36683=CARTESIAN_POINT('Origin',(0.,22.,-840.));
#36684=CARTESIAN_POINT('',(-1.75,0.500000000000001,-836.968911086755));
#36685=CARTESIAN_POINT('',(1.75,0.5,-836.968911086755));
#36686=CARTESIAN_POINT('Origin',(0.,0.5,-840.));
#36687=CARTESIAN_POINT('',(-2.25000000000004,0.,-837.319048676309));
#36688=CARTESIAN_POINT('Origin',(-6.72148608993339E-8,2.24999993278898,
-839.999999903682));
#36689=CARTESIAN_POINT('',(-2.25000000000004,0.,-842.680951323691));
#36690=CARTESIAN_POINT('Origin',(0.,0.,-840.));
#36691=CARTESIAN_POINT('',(-1.75,0.500000000000001,-843.031088913246));
#36692=CARTESIAN_POINT('Origin',(1.20611344800459E-7,2.25000012061502,-839.999999826881));
#36693=CARTESIAN_POINT('',(-4.28626379701574E-16,0.499999999999998,-843.5));
#36694=CARTESIAN_POINT('Origin',(0.,0.5,-840.));
#36695=CARTESIAN_POINT('',(-4.28626379701567E-16,13.,-843.5));
#36696=CARTESIAN_POINT('',(-4.28626379701567E-16,22.,-843.5));
#36697=CARTESIAN_POINT('Origin',(0.,13.,-840.));
#36698=CARTESIAN_POINT('',(1.75,0.5,-843.031088913246));
#36699=CARTESIAN_POINT('Origin',(0.,0.5,-840.));
#36700=CARTESIAN_POINT('',(2.25,0.,-842.680951323691));
#36701=CARTESIAN_POINT('Origin',(4.35037561530294E-10,2.24999999956476,
-840.000000000521));
#36702=CARTESIAN_POINT('',(2.24999999999995,0.,-837.319048676309));
#36703=CARTESIAN_POINT('Origin',(0.,0.,-840.));
#36704=CARTESIAN_POINT('Origin',(1.82089687772446E-8,2.24999998178678,-839.999999973692));
#36705=CARTESIAN_POINT('Origin',(0.,22.,-780.));
#36706=CARTESIAN_POINT('',(-6.73555739531038E-16,13.,-785.5));
#36707=CARTESIAN_POINT('Origin',(0.,13.,-780.));
#36708=CARTESIAN_POINT('',(-6.73555739531038E-16,22.,-785.5));
#36709=CARTESIAN_POINT('',(-6.73555739531038E-16,22.,-785.5));
#36710=CARTESIAN_POINT('Origin',(0.,22.,-780.));
#36711=CARTESIAN_POINT('Origin',(0.,22.,-780.));
#36712=CARTESIAN_POINT('',(-1.75,0.500000000000001,-776.968911086755));
#36713=CARTESIAN_POINT('',(1.75,0.5,-776.968911086755));
#36714=CARTESIAN_POINT('Origin',(0.,0.5,-780.));
#36715=CARTESIAN_POINT('',(-2.25000000000004,0.,-777.319048676309));
#36716=CARTESIAN_POINT('Origin',(-2.60525212514295E-9,2.24999999739851,
-779.99999999796));
#36717=CARTESIAN_POINT('',(-2.25000000000004,0.,-782.680951323691));
#36718=CARTESIAN_POINT('Origin',(0.,0.,-780.));
#36719=CARTESIAN_POINT('',(-1.75,0.500000000000001,-783.031088913246));
#36720=CARTESIAN_POINT('Origin',(8.94748081181618E-8,2.25000008947852,-779.999999871003));
#36721=CARTESIAN_POINT('',(-4.28626379701574E-16,0.499999999999998,-783.5));
#36722=CARTESIAN_POINT('Origin',(0.,0.5,-780.));
#36723=CARTESIAN_POINT('',(-4.28626379701567E-16,13.,-783.5));
#36724=CARTESIAN_POINT('',(-4.28626379701567E-16,22.,-783.5));
#36725=CARTESIAN_POINT('Origin',(0.,13.,-780.));
#36726=CARTESIAN_POINT('',(1.75,0.5,-783.031088913246));
#36727=CARTESIAN_POINT('Origin',(0.,0.5,-780.));
#36728=CARTESIAN_POINT('',(2.25,0.,-782.680951323691));
#36729=CARTESIAN_POINT('Origin',(-2.84421083907027E-8,2.2500000284419,-779.999999958075));
#36730=CARTESIAN_POINT('',(2.24999999999995,0.,-777.319048676309));
#36731=CARTESIAN_POINT('Origin',(0.,0.,-780.));
#36732=CARTESIAN_POINT('Origin',(7.35978125665504E-8,2.24999992639779,-779.99999989504));
#36733=CARTESIAN_POINT('Origin',(0.,22.,-720.));
#36734=CARTESIAN_POINT('',(-6.73555739531038E-16,13.,-725.5));
#36735=CARTESIAN_POINT('Origin',(0.,13.,-720.));
#36736=CARTESIAN_POINT('',(-6.73555739531038E-16,22.,-725.5));
#36737=CARTESIAN_POINT('',(-6.73555739531038E-16,22.,-725.5));
#36738=CARTESIAN_POINT('Origin',(0.,22.,-720.));
#36739=CARTESIAN_POINT('Origin',(0.,22.,-720.));
#36740=CARTESIAN_POINT('',(-1.75,0.500000000000001,-716.968911086754));
#36741=CARTESIAN_POINT('',(1.75,0.5,-716.968911086754));
#36742=CARTESIAN_POINT('Origin',(0.,0.5,-720.));
#36743=CARTESIAN_POINT('',(-2.25000000000004,0.,-717.319048676309));
#36744=CARTESIAN_POINT('Origin',(-5.15937745304562E-8,2.24999994841004,
-719.999999928058));
#36745=CARTESIAN_POINT('',(-2.25000000000004,0.,-722.680951323691));
#36746=CARTESIAN_POINT('Origin',(0.,0.,-720.));
#36747=CARTESIAN_POINT('',(-1.75,0.500000000000001,-723.031088913246));
#36748=CARTESIAN_POINT('Origin',(5.95435789563226E-8,2.25000005954729,-719.999999914124));
#36749=CARTESIAN_POINT('',(-4.28626379701574E-16,0.499999999999998,-723.5));
#36750=CARTESIAN_POINT('Origin',(0.,0.5,-720.));
#36751=CARTESIAN_POINT('',(-4.28626379701567E-16,13.,-723.5));
#36752=CARTESIAN_POINT('',(-4.28626379701567E-16,22.,-723.5));
#36753=CARTESIAN_POINT('Origin',(0.,13.,-720.));
#36754=CARTESIAN_POINT('',(1.75,0.5,-723.031088913246));
#36755=CARTESIAN_POINT('Origin',(0.,0.5,-720.));
#36756=CARTESIAN_POINT('',(2.25,0.,-722.680951323691));
#36757=CARTESIAN_POINT('Origin',(-9.57767809506294E-9,2.25000000957741,
-719.9999999846));
#36758=CARTESIAN_POINT('',(2.24999999999995,0.,-717.319048676309));
#36759=CARTESIAN_POINT('Origin',(0.,0.,-720.));
#36760=CARTESIAN_POINT('Origin',(3.69489749907359E-8,2.24999996304662,-719.999999947332));
#36761=CARTESIAN_POINT('Origin',(0.,22.,-660.));
#36762=CARTESIAN_POINT('',(-6.73555739531038E-16,13.,-665.5));
#36763=CARTESIAN_POINT('Origin',(0.,13.,-660.));
#36764=CARTESIAN_POINT('',(-6.73555739531038E-16,22.,-665.5));
#36765=CARTESIAN_POINT('',(-6.73555739531038E-16,22.,-665.5));
#36766=CARTESIAN_POINT('Origin',(0.,22.,-660.));
#36767=CARTESIAN_POINT('Origin',(0.,22.,-660.));
#36768=CARTESIAN_POINT('',(-1.75,0.500000000000001,-656.968911086754));
#36769=CARTESIAN_POINT('',(1.75,0.5,-656.968911086754));
#36770=CARTESIAN_POINT('Origin',(0.,0.5,-660.));
#36771=CARTESIAN_POINT('',(-2.25000000000004,0.,-657.319048676309));
#36772=CARTESIAN_POINT('Origin',(-7.48657963400845E-8,2.24999992513803,
-659.999999894045));
#36773=CARTESIAN_POINT('',(-2.25000000000004,0.,-662.680951323691));
#36774=CARTESIAN_POINT('Origin',(0.,0.,-660.));
#36775=CARTESIAN_POINT('',(-1.75,0.500000000000001,-663.031088913246));
#36776=CARTESIAN_POINT('Origin',(2.28832450210881E-8,2.25000002288697,-659.999999966479));
#36777=CARTESIAN_POINT('',(-4.28626379701574E-16,0.499999999999998,-663.5));
#36778=CARTESIAN_POINT('Origin',(0.,0.5,-660.));
#36779=CARTESIAN_POINT('',(-4.28626379701567E-16,13.,-663.5));
#36780=CARTESIAN_POINT('',(-4.28626379701567E-16,22.,-663.5));
#36781=CARTESIAN_POINT('Origin',(0.,13.,-660.));
#36782=CARTESIAN_POINT('',(1.75,0.5,-663.031088913246));
#36783=CARTESIAN_POINT('Origin',(0.,0.5,-660.));
#36784=CARTESIAN_POINT('',(2.25,0.,-662.680951323691));
#36785=CARTESIAN_POINT('Origin',(-1.19103271689625E-8,2.25000001191003,
-659.999999982899));
#36786=CARTESIAN_POINT('',(2.24999999999995,0.,-657.319048676309));
#36787=CARTESIAN_POINT('Origin',(0.,0.,-660.));
#36788=CARTESIAN_POINT('Origin',(1.36341934964257E-8,2.24999998636149,-659.999999981457));
#36789=CARTESIAN_POINT('Origin',(0.,22.,-600.));
#36790=CARTESIAN_POINT('',(-6.73555739531038E-16,13.,-605.5));
#36791=CARTESIAN_POINT('Origin',(0.,13.,-600.));
#36792=CARTESIAN_POINT('',(-6.73555739531038E-16,22.,-605.5));
#36793=CARTESIAN_POINT('',(-6.73555739531038E-16,22.,-605.5));
#36794=CARTESIAN_POINT('Origin',(0.,22.,-600.));
#36795=CARTESIAN_POINT('Origin',(0.,22.,-600.));
#36796=CARTESIAN_POINT('',(-1.75,0.500000000000001,-596.968911086754));
#36797=CARTESIAN_POINT('',(1.75,0.5,-596.968911086754));
#36798=CARTESIAN_POINT('Origin',(0.,0.5,-600.));
#36799=CARTESIAN_POINT('',(-2.25000000000004,0.,-597.319048676309));
#36800=CARTESIAN_POINT('Origin',(1.7384990669278E-8,2.25000001738872,-600.000000025331));
#36801=CARTESIAN_POINT('',(-2.25000000000004,0.,-602.680951323691));
#36802=CARTESIAN_POINT('Origin',(0.,0.,-600.));
#36803=CARTESIAN_POINT('',(-1.75,0.500000000000001,-603.031088913246));
#36804=CARTESIAN_POINT('Origin',(2.39434153059825E-8,2.25000002394707,-599.999999965723));
#36805=CARTESIAN_POINT('',(-4.28626379701574E-16,0.499999999999998,-603.5));
#36806=CARTESIAN_POINT('Origin',(0.,0.5,-600.));
#36807=CARTESIAN_POINT('',(-4.28626379701567E-16,13.,-603.5));
#36808=CARTESIAN_POINT('',(-4.28626379701567E-16,22.,-603.5));
#36809=CARTESIAN_POINT('Origin',(0.,13.,-600.));
#36810=CARTESIAN_POINT('',(1.75,0.5,-603.031088913246));
#36811=CARTESIAN_POINT('Origin',(0.,0.5,-600.));
#36812=CARTESIAN_POINT('',(2.25,0.,-602.680951323691));
#36813=CARTESIAN_POINT('Origin',(-2.74330147487234E-8,2.25000002743268,
-599.999999960943));
#36814=CARTESIAN_POINT('',(2.24999999999995,0.,-597.319048676309));
#36815=CARTESIAN_POINT('Origin',(0.,0.,-600.));
#36816=CARTESIAN_POINT('Origin',(2.99699681738375E-9,2.24999999699866,-599.999999995609));
#36817=CARTESIAN_POINT('Origin',(0.,22.,-540.));
#36818=CARTESIAN_POINT('',(-6.73555739531038E-16,13.,-545.5));
#36819=CARTESIAN_POINT('Origin',(0.,13.,-540.));
#36820=CARTESIAN_POINT('',(-6.73555739531038E-16,22.,-545.5));
#36821=CARTESIAN_POINT('',(-6.73555739531038E-16,22.,-545.5));
#36822=CARTESIAN_POINT('Origin',(0.,22.,-540.));
#36823=CARTESIAN_POINT('Origin',(0.,22.,-540.));
#36824=CARTESIAN_POINT('',(-1.75,0.500000000000001,-536.968911086754));
#36825=CARTESIAN_POINT('',(1.75,0.5,-536.968911086754));
#36826=CARTESIAN_POINT('Origin',(0.,0.5,-540.));
#36827=CARTESIAN_POINT('',(-2.25000000000004,0.,-537.319048676309));
#36828=CARTESIAN_POINT('Origin',(1.84421247717559E-8,2.25000001844588,-540.000000026007));
#36829=CARTESIAN_POINT('',(-2.25000000000004,0.,-542.680951323691));
#36830=CARTESIAN_POINT('Origin',(0.,0.,-540.));
#36831=CARTESIAN_POINT('',(-1.75,0.500000000000001,-543.031088913246));
#36832=CARTESIAN_POINT('Origin',(6.61566706972039E-8,2.25000006616034,-539.999999905105));
#36833=CARTESIAN_POINT('',(-4.28626379701574E-16,0.499999999999998,-543.5));
#36834=CARTESIAN_POINT('Origin',(0.,0.5,-540.));
#36835=CARTESIAN_POINT('',(-4.28626379701567E-16,13.,-543.5));
#36836=CARTESIAN_POINT('',(-4.28626379701567E-16,22.,-543.5));
#36837=CARTESIAN_POINT('Origin',(0.,13.,-540.));
#36838=CARTESIAN_POINT('',(1.75,0.5,-543.031088913246));
#36839=CARTESIAN_POINT('Origin',(0.,0.5,-540.));
#36840=CARTESIAN_POINT('',(2.25,0.,-542.680951323691));
#36841=CARTESIAN_POINT('Origin',(-7.42096994965635E-9,2.25000000742066,
-539.999999990521));
#36842=CARTESIAN_POINT('',(2.24999999999995,0.,-537.319048676309));
#36843=CARTESIAN_POINT('Origin',(0.,0.,-540.));
#36844=CARTESIAN_POINT('Origin',(4.35878827476088E-8,2.24999995640769,-539.999999938266));
#36845=CARTESIAN_POINT('Origin',(0.,22.,-480.));
#36846=CARTESIAN_POINT('',(-6.73555739531045E-16,13.,-485.5));
#36847=CARTESIAN_POINT('Origin',(0.,13.,-480.));
#36848=CARTESIAN_POINT('',(-6.73555739531045E-16,22.,-485.5));
#36849=CARTESIAN_POINT('',(-6.73555739531045E-16,22.,-485.5));
#36850=CARTESIAN_POINT('Origin',(0.,22.,-480.));
#36851=CARTESIAN_POINT('Origin',(0.,22.,-480.));
#36852=CARTESIAN_POINT('',(-1.75,0.500000000000001,-476.968911086754));
#36853=CARTESIAN_POINT('',(1.75,0.5,-476.968911086754));
#36854=CARTESIAN_POINT('Origin',(0.,0.5,-480.));
#36855=CARTESIAN_POINT('',(-2.25,0.,-477.319048676309));
#36856=CARTESIAN_POINT('Origin',(1.90741897276858E-8,2.2500000190738,-480.000000026514));
#36857=CARTESIAN_POINT('',(-2.25,0.,-482.680951323691));
#36858=CARTESIAN_POINT('Origin',(0.,0.,-480.));
#36859=CARTESIAN_POINT('',(-1.75,0.500000000000001,-483.031088913246));
#36860=CARTESIAN_POINT('Origin',(-1.93385135682789E-8,2.24999998066101,
-480.000000027097));
#36861=CARTESIAN_POINT('',(-4.28626379701572E-16,0.499999999999998,-483.5));
#36862=CARTESIAN_POINT('Origin',(0.,0.5,-480.));
#36863=CARTESIAN_POINT('',(-4.28626379701574E-16,13.,-483.5));
#36864=CARTESIAN_POINT('',(-4.28626379701574E-16,22.,-483.5));
#36865=CARTESIAN_POINT('Origin',(0.,13.,-480.));
#36866=CARTESIAN_POINT('',(1.75,0.5,-483.031088913246));
#36867=CARTESIAN_POINT('Origin',(0.,0.5,-480.));
#36868=CARTESIAN_POINT('',(2.25,0.,-482.680951323691));
#36869=CARTESIAN_POINT('Origin',(-4.27040211525842E-8,2.25000004270368,
-479.99999993896));
#36870=CARTESIAN_POINT('',(2.25,0.,-477.319048676309));
#36871=CARTESIAN_POINT('Origin',(0.,0.,-480.));
#36872=CARTESIAN_POINT('Origin',(-2.40762548786577E-9,2.25000000240756,
-480.000000003701));
#36873=CARTESIAN_POINT('Origin',(0.,22.,-420.));
#36874=CARTESIAN_POINT('',(-6.73555739531045E-16,13.,-425.5));
#36875=CARTESIAN_POINT('Origin',(0.,13.,-420.));
#36876=CARTESIAN_POINT('',(-6.73555739531045E-16,22.,-425.5));
#36877=CARTESIAN_POINT('',(-6.73555739531045E-16,22.,-425.5));
#36878=CARTESIAN_POINT('Origin',(0.,22.,-420.));
#36879=CARTESIAN_POINT('Origin',(0.,22.,-420.));
#36880=CARTESIAN_POINT('',(-1.75,0.500000000000001,-416.968911086754));
#36881=CARTESIAN_POINT('',(1.75,0.5,-416.968911086754));
#36882=CARTESIAN_POINT('Origin',(0.,0.5,-420.));
#36883=CARTESIAN_POINT('',(-2.25,0.,-417.319048676309));
#36884=CARTESIAN_POINT('Origin',(1.23725557577004E-8,2.25000001237209,-420.000000017334));
#36885=CARTESIAN_POINT('',(-2.25,0.,-422.680951323691));
#36886=CARTESIAN_POINT('Origin',(0.,0.,-420.));
#36887=CARTESIAN_POINT('',(-1.75,0.500000000000001,-423.031088913246));
#36888=CARTESIAN_POINT('Origin',(-3.09946213139511E-8,2.24999996900483,
-420.000000044132));
#36889=CARTESIAN_POINT('',(-4.28626379701572E-16,0.499999999999998,-423.5));
#36890=CARTESIAN_POINT('Origin',(0.,0.5,-420.));
#36891=CARTESIAN_POINT('',(-4.28626379701574E-16,13.,-423.5));
#36892=CARTESIAN_POINT('',(-4.28626379701574E-16,22.,-423.5));
#36893=CARTESIAN_POINT('Origin',(0.,13.,-420.));
#36894=CARTESIAN_POINT('',(1.75,0.5,-423.031088913246));
#36895=CARTESIAN_POINT('Origin',(0.,0.5,-420.));
#36896=CARTESIAN_POINT('',(2.25,-2.16840434497101E-16,-422.680951323691));
#36897=CARTESIAN_POINT('Origin',(-1.4602281606102E-8,2.25000001460212,-419.999999978837));
#36898=CARTESIAN_POINT('',(2.25,-2.16840434497101E-16,-417.319048676309));
#36899=CARTESIAN_POINT('Origin',(0.,0.,-420.));
#36900=CARTESIAN_POINT('Origin',(5.91723503529096E-9,2.24999999408246,-419.999999991203));
#36901=CARTESIAN_POINT('Origin',(0.,22.,-360.));
#36902=CARTESIAN_POINT('',(-6.73555739531045E-16,13.,-365.5));
#36903=CARTESIAN_POINT('Origin',(0.,13.,-360.));
#36904=CARTESIAN_POINT('',(-6.73555739531045E-16,22.,-365.5));
#36905=CARTESIAN_POINT('',(-6.73555739531045E-16,22.,-365.5));
#36906=CARTESIAN_POINT('Origin',(0.,22.,-360.));
#36907=CARTESIAN_POINT('Origin',(0.,22.,-360.));
#36908=CARTESIAN_POINT('',(-1.75,0.500000000000001,-356.968911086754));
#36909=CARTESIAN_POINT('',(1.75,0.5,-356.968911086754));
#36910=CARTESIAN_POINT('Origin',(0.,0.5,-360.));
#36911=CARTESIAN_POINT('',(-2.25,0.,-357.319048676309));
#36912=CARTESIAN_POINT('Origin',(-1.82331699738469E-8,2.2499999817664,-359.999999973701));
#36913=CARTESIAN_POINT('',(-2.25,0.,-362.680951323691));
#36914=CARTESIAN_POINT('Origin',(0.,0.,-360.));
#36915=CARTESIAN_POINT('',(-1.75,0.500000000000001,-363.031088913246));
#36916=CARTESIAN_POINT('Origin',(-4.38715175299365E-10,2.2499999995608,
-360.000000000543));
#36917=CARTESIAN_POINT('',(-4.28626379701572E-16,0.499999999999998,-363.5));
#36918=CARTESIAN_POINT('Origin',(0.,0.5,-360.));
#36919=CARTESIAN_POINT('',(-4.28626379701574E-16,13.,-363.5));
#36920=CARTESIAN_POINT('',(-4.28626379701574E-16,22.,-363.5));
#36921=CARTESIAN_POINT('Origin',(0.,13.,-360.));
#36922=CARTESIAN_POINT('',(1.75,0.5,-363.031088913246));
#36923=CARTESIAN_POINT('Origin',(0.,0.5,-360.));
#36924=CARTESIAN_POINT('',(2.25,-2.16840434497101E-16,-362.680951323691));
#36925=CARTESIAN_POINT('Origin',(-1.45931708384062E-8,2.25000001459299,
-359.999999978876));
#36926=CARTESIAN_POINT('',(2.25,-2.16840434497101E-16,-357.319048676309));
#36927=CARTESIAN_POINT('Origin',(0.,0.,-360.));
#36928=CARTESIAN_POINT('Origin',(1.5377042417164E-8,2.24999998462267,-359.999999977933));
#36929=CARTESIAN_POINT('Origin',(0.,22.,-300.));
#36930=CARTESIAN_POINT('',(-6.73555739531045E-16,13.,-305.5));
#36931=CARTESIAN_POINT('Origin',(0.,13.,-300.));
#36932=CARTESIAN_POINT('',(-6.73555739531045E-16,22.,-305.5));
#36933=CARTESIAN_POINT('',(-6.73555739531045E-16,22.,-305.5));
#36934=CARTESIAN_POINT('Origin',(0.,22.,-300.));
#36935=CARTESIAN_POINT('Origin',(0.,22.,-300.));
#36936=CARTESIAN_POINT('',(-1.75,0.500000000000001,-296.968911086754));
#36937=CARTESIAN_POINT('',(1.75,0.5,-296.968911086754));
#36938=CARTESIAN_POINT('Origin',(0.,0.5,-300.));
#36939=CARTESIAN_POINT('',(-2.25,0.,-297.319048676309));
#36940=CARTESIAN_POINT('Origin',(-2.37414948811576E-9,2.24999999762542,
-299.999999997033));
#36941=CARTESIAN_POINT('',(-2.25,0.,-302.680951323691));
#36942=CARTESIAN_POINT('Origin',(0.,0.,-300.));
#36943=CARTESIAN_POINT('',(-1.75,0.500000000000001,-303.031088913246));
#36944=CARTESIAN_POINT('Origin',(-5.11385406243292E-9,2.24999999488564,
-300.000000007122));
#36945=CARTESIAN_POINT('',(-4.28626379701572E-16,0.499999999999998,-303.5));
#36946=CARTESIAN_POINT('Origin',(0.,0.5,-300.));
#36947=CARTESIAN_POINT('',(-4.28626379701574E-16,13.,-303.5));
#36948=CARTESIAN_POINT('',(-4.28626379701574E-16,22.,-303.5));
#36949=CARTESIAN_POINT('Origin',(0.,13.,-300.));
#36950=CARTESIAN_POINT('',(1.75,0.5,-303.031088913245));
#36951=CARTESIAN_POINT('Origin',(0.,0.5,-300.));
#36952=CARTESIAN_POINT('',(2.25,-2.16840434497101E-16,-302.680951323691));
#36953=CARTESIAN_POINT('Origin',(-1.07341244226511E-8,2.25000001073404,
-299.999999984895));
#36954=CARTESIAN_POINT('',(2.25,-2.16840434497101E-16,-297.319048676309));
#36955=CARTESIAN_POINT('Origin',(0.,0.,-300.));
#36956=CARTESIAN_POINT('Origin',(1.81055004322417E-9,2.24999999818928,-299.999999997399));
#36957=CARTESIAN_POINT('Origin',(0.,22.,-240.));
#36958=CARTESIAN_POINT('',(-6.73555739531045E-16,13.,-245.5));
#36959=CARTESIAN_POINT('Origin',(0.,13.,-240.));
#36960=CARTESIAN_POINT('',(-6.73555739531045E-16,22.,-245.5));
#36961=CARTESIAN_POINT('',(-6.73555739531045E-16,22.,-245.5));
#36962=CARTESIAN_POINT('Origin',(0.,22.,-240.));
#36963=CARTESIAN_POINT('Origin',(0.,22.,-240.));
#36964=CARTESIAN_POINT('',(-1.75,0.500000000000001,-236.968911086754));
#36965=CARTESIAN_POINT('',(1.75,0.5,-236.968911086754));
#36966=CARTESIAN_POINT('Origin',(0.,0.5,-240.));
#36967=CARTESIAN_POINT('',(-2.25,0.,-237.319048676309));
#36968=CARTESIAN_POINT('Origin',(1.47928452820523E-8,2.2500000147927,-240.000000021201));
#36969=CARTESIAN_POINT('',(-2.25,0.,-242.680951323691));
#36970=CARTESIAN_POINT('Origin',(0.,0.,-240.));
#36971=CARTESIAN_POINT('',(-1.75,0.500000000000001,-243.031088913246));
#36972=CARTESIAN_POINT('Origin',(-1.55246204780468E-9,2.24999999844734,
-240.000000002442));
#36973=CARTESIAN_POINT('',(-4.28626379701572E-16,0.499999999999998,-243.5));
#36974=CARTESIAN_POINT('Origin',(0.,0.5,-240.));
#36975=CARTESIAN_POINT('',(-4.28626379701574E-16,13.,-243.5));
#36976=CARTESIAN_POINT('',(-4.28626379701574E-16,22.,-243.5));
#36977=CARTESIAN_POINT('Origin',(0.,13.,-240.));
#36978=CARTESIAN_POINT('',(1.75,0.5,-243.031088913246));
#36979=CARTESIAN_POINT('Origin',(0.,0.5,-240.));
#36980=CARTESIAN_POINT('',(2.25,-2.16840434497101E-16,-242.680951323691));
#36981=CARTESIAN_POINT('Origin',(-7.64266927522073E-9,2.25000000764248,
-239.99999998931));
#36982=CARTESIAN_POINT('',(2.25,-2.16840434497101E-16,-237.319048676309));
#36983=CARTESIAN_POINT('Origin',(0.,0.,-240.));
#36984=CARTESIAN_POINT('Origin',(3.72062075593149E-9,2.24999999627917,-239.999999994952));
#36985=CARTESIAN_POINT('Origin',(0.,22.,-180.));
#36986=CARTESIAN_POINT('',(-6.73555739531045E-16,13.,-185.5));
#36987=CARTESIAN_POINT('Origin',(0.,13.,-180.));
#36988=CARTESIAN_POINT('',(-6.73555739531045E-16,22.,-185.5));
#36989=CARTESIAN_POINT('',(-6.73555739531045E-16,22.,-185.5));
#36990=CARTESIAN_POINT('Origin',(0.,22.,-180.));
#36991=CARTESIAN_POINT('Origin',(0.,22.,-180.));
#36992=CARTESIAN_POINT('',(-1.75,0.500000000000001,-176.968911086754));
#36993=CARTESIAN_POINT('',(1.75,0.5,-176.968911086755));
#36994=CARTESIAN_POINT('Origin',(0.,0.5,-180.));
#36995=CARTESIAN_POINT('',(-2.25000000000001,0.,-177.319048676309));
#36996=CARTESIAN_POINT('Origin',(8.34885383049766E-9,2.25000000834883,-180.000000012206));
#36997=CARTESIAN_POINT('',(-2.25000000000001,0.,-182.680951323691));
#36998=CARTESIAN_POINT('Origin',(0.,0.,-180.));
#36999=CARTESIAN_POINT('',(-1.75,0.500000000000001,-183.031088913246));
#37000=CARTESIAN_POINT('Origin',(-1.07031097873467E-8,2.24999998929679,
-180.00000001549));
#37001=CARTESIAN_POINT('',(-4.28626379701572E-16,0.499999999999998,-183.5));
#37002=CARTESIAN_POINT('Origin',(0.,0.5,-180.));
#37003=CARTESIAN_POINT('',(-4.28626379701574E-16,13.,-183.5));
#37004=CARTESIAN_POINT('',(-4.28626379701574E-16,22.,-183.5));
#37005=CARTESIAN_POINT('Origin',(0.,13.,-180.));
#37006=CARTESIAN_POINT('',(1.75,0.5,-183.031088913246));
#37007=CARTESIAN_POINT('Origin',(0.,0.5,-180.));
#37008=CARTESIAN_POINT('',(2.25,-2.16840434497101E-16,-182.680951323691));
#37009=CARTESIAN_POINT('Origin',(6.25733659331829E-9,2.24999999374259,-180.000000009063));
#37010=CARTESIAN_POINT('',(2.25,-2.16840434497101E-16,-177.319048676309));
#37011=CARTESIAN_POINT('Origin',(0.,0.,-180.));
#37012=CARTESIAN_POINT('Origin',(3.19985427044145E-9,2.24999999679997,-179.999999995321));
#37013=CARTESIAN_POINT('Origin',(0.,22.,-120.));
#37014=CARTESIAN_POINT('',(-6.73555739531045E-16,13.,-125.5));
#37015=CARTESIAN_POINT('Origin',(0.,13.,-120.));
#37016=CARTESIAN_POINT('',(-6.73555739531045E-16,22.,-125.5));
#37017=CARTESIAN_POINT('',(-6.73555739531045E-16,22.,-125.5));
#37018=CARTESIAN_POINT('Origin',(0.,22.,-120.));
#37019=CARTESIAN_POINT('Origin',(0.,22.,-120.));
#37020=CARTESIAN_POINT('',(-1.75,0.500000000000001,-116.968911086754));
#37021=CARTESIAN_POINT('',(1.75,0.5,-116.968911086754));
#37022=CARTESIAN_POINT('Origin',(0.,0.5,-120.));
#37023=CARTESIAN_POINT('',(-2.25000000000001,0.,-117.319048676309));
#37024=CARTESIAN_POINT('Origin',(-4.79071532444308E-9,2.24999999520912,
-119.999999993143));
#37025=CARTESIAN_POINT('',(-2.25000000000001,0.,-122.680951323691));
#37026=CARTESIAN_POINT('Origin',(0.,0.,-120.));
#37027=CARTESIAN_POINT('',(-1.75,0.500000000000001,-123.031088913246));
#37028=CARTESIAN_POINT('Origin',(-5.64915392242682E-9,2.2499999943508,-120.000000008031));
#37029=CARTESIAN_POINT('',(-4.28626379701574E-16,0.499999999999998,-123.5));
#37030=CARTESIAN_POINT('Origin',(0.,0.5,-120.));
#37031=CARTESIAN_POINT('',(-4.28626379701574E-16,13.,-123.5));
#37032=CARTESIAN_POINT('',(-4.28626379701574E-16,22.,-123.5));
#37033=CARTESIAN_POINT('Origin',(0.,13.,-120.));
#37034=CARTESIAN_POINT('',(1.75,0.5,-123.031088913246));
#37035=CARTESIAN_POINT('Origin',(0.,0.5,-120.));
#37036=CARTESIAN_POINT('',(2.25,-2.16840434497101E-16,-122.680951323691));
#37037=CARTESIAN_POINT('Origin',(-1.26511134901364E-9,2.25000000126489,
-119.99999999821));
#37038=CARTESIAN_POINT('',(2.25,-2.16840434497101E-16,-117.319048676309));
#37039=CARTESIAN_POINT('Origin',(0.,0.,-120.));
#37040=CARTESIAN_POINT('Origin',(-1.13244302824E-9,2.25000000113215,-120.000000001689));
#37041=CARTESIAN_POINT('Origin',(0.,22.,-60.));
#37042=CARTESIAN_POINT('',(-6.73555739531044E-16,13.,-65.5));
#37043=CARTESIAN_POINT('Origin',(0.,13.,-60.));
#37044=CARTESIAN_POINT('',(-6.73555739531044E-16,22.,-65.5));
#37045=CARTESIAN_POINT('',(-6.73555739531044E-16,22.,-65.5));
#37046=CARTESIAN_POINT('Origin',(0.,22.,-60.));
#37047=CARTESIAN_POINT('Origin',(0.,22.,-60.));
#37048=CARTESIAN_POINT('',(-1.75,0.500000000000001,-56.9689110867545));
#37049=CARTESIAN_POINT('',(1.75,0.5,-56.9689110867544));
#37050=CARTESIAN_POINT('Origin',(0.,0.5,-60.));
#37051=CARTESIAN_POINT('',(-2.25000000000001,0.,-57.3190486763091));
#37052=CARTESIAN_POINT('Origin',(-1.35908062581791E-9,2.24999999864092,
-59.9999999980204));
#37053=CARTESIAN_POINT('',(-2.25,0.,-62.6809513236909));
#37054=CARTESIAN_POINT('Origin',(0.,0.,-60.));
#37055=CARTESIAN_POINT('',(-1.75,0.500000000000001,-63.0310889132455));
#37056=CARTESIAN_POINT('Origin',(-9.11769826306141E-10,2.24999999908773,
-60.0000000013664));
#37057=CARTESIAN_POINT('',(-4.28626379701573E-16,0.499999999999998,-63.5));
#37058=CARTESIAN_POINT('Origin',(0.,0.5,-60.));
#37059=CARTESIAN_POINT('',(-4.28626379701573E-16,13.,-63.5));
#37060=CARTESIAN_POINT('',(-4.28626379701573E-16,22.,-63.5));
#37061=CARTESIAN_POINT('Origin',(0.,13.,-60.));
#37062=CARTESIAN_POINT('',(1.75,0.5,-63.0310889132455));
#37063=CARTESIAN_POINT('Origin',(0.,0.5,-60.));
#37064=CARTESIAN_POINT('',(2.25,-2.16840434497101E-16,-62.6809513236909));
#37065=CARTESIAN_POINT('Origin',(2.79500866895432E-10,2.24999999972038,
-60.0000000003599));
#37066=CARTESIAN_POINT('',(2.25,-2.16840434497101E-16,-57.3190486763091));
#37067=CARTESIAN_POINT('Origin',(0.,0.,-60.));
#37068=CARTESIAN_POINT('Origin',(-1.95772009714545E-10,2.25000000019565,
-60.0000000001797));
#37069=CARTESIAN_POINT('Origin',(0.,22.,0.));
#37070=CARTESIAN_POINT('',(-6.73555739531044E-16,13.,-5.5));
#37071=CARTESIAN_POINT('Origin',(0.,13.,0.));
#37072=CARTESIAN_POINT('',(-6.73555739531044E-16,22.,-5.5));
#37073=CARTESIAN_POINT('',(-6.73555739531044E-16,22.,-5.5));
#37074=CARTESIAN_POINT('Origin',(0.,22.,0.));
#37075=CARTESIAN_POINT('Origin',(0.,22.,0.));
#37076=CARTESIAN_POINT('',(-1.75,0.500000000000001,3.03108891324553));
#37077=CARTESIAN_POINT('',(1.75,0.5,3.03108891324555));
#37078=CARTESIAN_POINT('Origin',(0.,0.5,0.));
#37079=CARTESIAN_POINT('',(-2.25,0.,2.68095132369089));
#37080=CARTESIAN_POINT('Origin',(1.37767852681492E-10,2.25000000013748,
-1.96202498692344E-10));
#37081=CARTESIAN_POINT('',(-2.25,0.,-2.68095132369089));
#37082=CARTESIAN_POINT('Origin',(0.,0.,0.));
#37083=CARTESIAN_POINT('',(-1.75,0.500000000000001,-3.03108891324553));
#37084=CARTESIAN_POINT('Origin',(1.01115227302273E-10,2.25000000010099,
1.42931222413267E-10));
#37085=CARTESIAN_POINT('',(-4.28626379701573E-16,0.499999999999998,-3.5));
#37086=CARTESIAN_POINT('Origin',(0.,0.5,0.));
#37087=CARTESIAN_POINT('',(-4.28626379701573E-16,13.,-3.5));
#37088=CARTESIAN_POINT('',(-4.28626379701573E-16,22.,-3.5));
#37089=CARTESIAN_POINT('Origin',(0.,13.,0.));
#37090=CARTESIAN_POINT('',(1.75,0.5,-3.03108891324555));
#37091=CARTESIAN_POINT('Origin',(0.,0.5,0.));
#37092=CARTESIAN_POINT('',(2.25,-2.16840434497101E-16,-2.6809513236909));
#37093=CARTESIAN_POINT('Origin',(-2.64255839432792E-10,2.25000000026401,
3.62936902753574E-10));
#37094=CARTESIAN_POINT('',(2.25,-2.16840434497101E-16,2.6809513236909));
#37095=CARTESIAN_POINT('Origin',(0.,0.,0.));
#37096=CARTESIAN_POINT('Origin',(-2.17712237127188E-10,2.25000000021748,
-2.98289171141164E-10));
#37097=CARTESIAN_POINT('Origin',(-2.25,-1.4389599889981E-16,-870.));
#37098=CARTESIAN_POINT('',(-1.75,0.5,-870.));
#37099=CARTESIAN_POINT('',(-1.75,0.5,-870.));
#37100=CARTESIAN_POINT('',(-2.25,-1.4389599889981E-16,-870.));
#37101=CARTESIAN_POINT('',(-2.25,-1.4389599889981E-16,-870.));
#37102=CARTESIAN_POINT('',(-2.25,-1.4389599889981E-16,-870.));
#37103=CARTESIAN_POINT('Origin',(1.75,0.5,-870.));
#37104=CARTESIAN_POINT('',(1.75,0.5,-870.));
#37105=CARTESIAN_POINT('',(2.25,-1.30104260698261E-15,-870.));
#37106=CARTESIAN_POINT('Origin',(0.,0.,-870.));
#37107=CARTESIAN_POINT('',(-2.25,-1.4389599889981E-16,-870.));
#37108=CARTESIAN_POINT('',(-2.25,-1.4389599889981E-16,-870.));
#37109=CARTESIAN_POINT('',(-2.25,-1.4389599889981E-16,-870.));
#37110=CARTESIAN_POINT('',(-2.25,-1.4389599889981E-16,-870.));
#37111=CARTESIAN_POINT('',(-2.25,-1.4389599889981E-16,-870.));
#37112=CARTESIAN_POINT('',(-2.25,-1.4389599889981E-16,-870.));
#37113=CARTESIAN_POINT('',(-2.25,-1.4389599889981E-16,-870.));
#37114=CARTESIAN_POINT('',(-2.25,-1.4389599889981E-16,-870.));
#37115=CARTESIAN_POINT('',(-2.25,-1.4389599889981E-16,-870.));
#37116=CARTESIAN_POINT('',(-2.25,-1.4389599889981E-16,-870.));
#37117=CARTESIAN_POINT('',(-2.25,-1.4389599889981E-16,-870.));
#37118=CARTESIAN_POINT('',(-2.25,-1.4389599889981E-16,-870.));
#37119=CARTESIAN_POINT('',(-2.25,-1.4389599889981E-16,-870.));
#37120=CARTESIAN_POINT('',(-2.25,-1.4389599889981E-16,-870.));
#37121=CARTESIAN_POINT('',(-2.25,-1.4389599889981E-16,30.));
#37122=CARTESIAN_POINT('',(-2.25,-1.4389599889981E-16,-870.));
#37123=CARTESIAN_POINT('',(-10.5,-1.28587913910472E-15,30.));
#37124=CARTESIAN_POINT('',(0.,0.,30.));
#37125=CARTESIAN_POINT('',(-10.5,-1.28587913910472E-15,-870.));
#37126=CARTESIAN_POINT('',(-10.5,-1.28587913910472E-15,-870.));
#37127=CARTESIAN_POINT('',(0.,0.,-870.));
#37128=CARTESIAN_POINT('Origin',(-1.75,0.5,-870.));
#37129=CARTESIAN_POINT('',(-1.75,0.5,-870.));
#37130=CARTESIAN_POINT('Origin',(0.,0.,-870.));
#37131=CARTESIAN_POINT('',(2.24999999999999,2.75545529808154E-16,-870.));
#37132=CARTESIAN_POINT('',(2.25,-1.30104260698261E-15,-870.));
#37133=CARTESIAN_POINT('',(10.5,-1.28587913910472E-15,-870.));
#37134=CARTESIAN_POINT('',(0.,0.,-870.));
#37135=CARTESIAN_POINT('',(10.5,-1.28587913910472E-15,30.));
#37136=CARTESIAN_POINT('',(10.5,-1.28587913910472E-15,-870.));
#37137=CARTESIAN_POINT('',(2.25,-1.30104260698261E-15,30.));
#37138=CARTESIAN_POINT('',(0.,0.,30.));
#37139=CARTESIAN_POINT('',(2.25,-1.30104260698261E-15,-870.));
#37140=CARTESIAN_POINT('',(2.25,-1.30104260698261E-15,-870.));
#37141=CARTESIAN_POINT('',(2.25,-1.30104260698261E-15,-870.));
#37142=CARTESIAN_POINT('',(2.25,-1.30104260698261E-15,-870.));
#37143=CARTESIAN_POINT('',(2.25,-1.30104260698261E-15,-870.));
#37144=CARTESIAN_POINT('',(2.25,-1.30104260698261E-15,-870.));
#37145=CARTESIAN_POINT('',(2.25,-1.30104260698261E-15,-870.));
#37146=CARTESIAN_POINT('',(2.25,-1.30104260698261E-15,-870.));
#37147=CARTESIAN_POINT('',(2.25,-1.30104260698261E-15,-870.));
#37148=CARTESIAN_POINT('',(2.25,-1.30104260698261E-15,-870.));
#37149=CARTESIAN_POINT('',(2.25,-1.30104260698261E-15,-870.));
#37150=CARTESIAN_POINT('',(2.25,-1.30104260698261E-15,-870.));
#37151=CARTESIAN_POINT('',(2.25,-1.30104260698261E-15,-870.));
#37152=CARTESIAN_POINT('',(2.25,-1.30104260698261E-15,-870.));
#37153=CARTESIAN_POINT('Origin',(-2.25,-1.4389599889981E-16,-870.));
#37154=CARTESIAN_POINT('Origin',(-1.75,0.5,-870.));
#37155=CARTESIAN_POINT('',(-1.75,0.5,-870.));
#37156=CARTESIAN_POINT('',(1.75,0.5,-870.));
#37157=CARTESIAN_POINT('Origin',(1.75,0.5,-870.));
#37158=CARTESIAN_POINT('Origin',(-2.25,-1.4389599889981E-16,-870.));
#37159=CARTESIAN_POINT('Origin',(-1.75,0.5,-870.));
#37160=CARTESIAN_POINT('',(-1.75,0.5,-870.));
#37161=CARTESIAN_POINT('',(1.75,0.5,-870.));
#37162=CARTESIAN_POINT('Origin',(1.75,0.5,-870.));
#37163=CARTESIAN_POINT('Origin',(-2.25,-1.4389599889981E-16,-870.));
#37164=CARTESIAN_POINT('Origin',(-1.75,0.5,-870.));
#37165=CARTESIAN_POINT('',(-1.75,0.5,-870.));
#37166=CARTESIAN_POINT('',(1.75,0.5,-870.));
#37167=CARTESIAN_POINT('Origin',(1.75,0.5,-870.));
#37168=CARTESIAN_POINT('Origin',(-2.25,-1.4389599889981E-16,-870.));
#37169=CARTESIAN_POINT('Origin',(-1.75,0.5,-870.));
#37170=CARTESIAN_POINT('',(-1.75,0.5,-870.));
#37171=CARTESIAN_POINT('',(1.75,0.5,-870.));
#37172=CARTESIAN_POINT('Origin',(1.75,0.5,-870.));
#37173=CARTESIAN_POINT('Origin',(-2.25,-1.4389599889981E-16,-870.));
#37174=CARTESIAN_POINT('Origin',(-1.75,0.5,-870.));
#37175=CARTESIAN_POINT('',(-1.75,0.5,-870.));
#37176=CARTESIAN_POINT('',(1.75,0.5,-870.));
#37177=CARTESIAN_POINT('Origin',(1.75,0.5,-870.));
#37178=CARTESIAN_POINT('Origin',(-2.25,-1.4389599889981E-16,-870.));
#37179=CARTESIAN_POINT('Origin',(-1.75,0.5,-870.));
#37180=CARTESIAN_POINT('',(-1.75,0.5,-870.));
#37181=CARTESIAN_POINT('',(1.75,0.5,-870.));
#37182=CARTESIAN_POINT('Origin',(1.75,0.5,-870.));
#37183=CARTESIAN_POINT('Origin',(-2.25,-1.4389599889981E-16,-870.));
#37184=CARTESIAN_POINT('Origin',(-1.75,0.5,-870.));
#37185=CARTESIAN_POINT('',(-1.75,0.5,-870.));
#37186=CARTESIAN_POINT('',(1.75,0.5,-870.));
#37187=CARTESIAN_POINT('Origin',(1.75,0.5,-870.));
#37188=CARTESIAN_POINT('Origin',(-2.25,-1.4389599889981E-16,-870.));
#37189=CARTESIAN_POINT('Origin',(-1.75,0.5,-870.));
#37190=CARTESIAN_POINT('',(-1.75,0.5,-870.));
#37191=CARTESIAN_POINT('',(1.75,0.5,-870.));
#37192=CARTESIAN_POINT('Origin',(1.75,0.5,-870.));
#37193=CARTESIAN_POINT('Origin',(-2.25,-1.4389599889981E-16,-870.));
#37194=CARTESIAN_POINT('Origin',(-1.75,0.5,-870.));
#37195=CARTESIAN_POINT('',(-1.75,0.5,-870.));
#37196=CARTESIAN_POINT('',(1.75,0.5,-870.));
#37197=CARTESIAN_POINT('Origin',(1.75,0.5,-870.));
#37198=CARTESIAN_POINT('Origin',(-1.75,0.5,-870.));
#37199=CARTESIAN_POINT('',(-1.75,0.5,-870.));
#37200=CARTESIAN_POINT('',(1.75,0.5,-870.));
#37201=CARTESIAN_POINT('Origin',(-2.25,-1.4389599889981E-16,-870.));
#37202=CARTESIAN_POINT('Origin',(1.75,0.5,-870.));
#37203=CARTESIAN_POINT('Origin',(-2.25,-1.4389599889981E-16,-870.));
#37204=CARTESIAN_POINT('Origin',(-1.75,0.5,-870.));
#37205=CARTESIAN_POINT('',(-1.75,0.5,-870.));
#37206=CARTESIAN_POINT('',(1.75,0.5,-870.));
#37207=CARTESIAN_POINT('Origin',(1.75,0.5,-870.));
#37208=CARTESIAN_POINT('Origin',(-2.25,-1.4389599889981E-16,-870.));
#37209=CARTESIAN_POINT('Origin',(-1.75,0.5,-870.));
#37210=CARTESIAN_POINT('',(-1.75,0.5,-870.));
#37211=CARTESIAN_POINT('',(1.75,0.5,-870.));
#37212=CARTESIAN_POINT('Origin',(1.75,0.5,-870.));
#37213=CARTESIAN_POINT('Origin',(-1.75,0.5,-870.));
#37214=CARTESIAN_POINT('',(-1.75,0.5,-870.));
#37215=CARTESIAN_POINT('',(1.75,0.5,-870.));
#37216=CARTESIAN_POINT('Origin',(-2.25,-1.4389599889981E-16,-870.));
#37217=CARTESIAN_POINT('Origin',(1.75,0.5,-870.));
#37218=CARTESIAN_POINT('Origin',(-1.75,0.5,-870.));
#37219=CARTESIAN_POINT('',(-1.75,0.5,30.));
#37220=CARTESIAN_POINT('',(-1.75,0.5,-870.));
#37221=CARTESIAN_POINT('',(1.75,0.5,30.));
#37222=CARTESIAN_POINT('',(1.75,0.5,-870.));
#37223=CARTESIAN_POINT('',(-1.75,0.5,30.));
#37224=CARTESIAN_POINT('Origin',(-2.25,-1.4389599889981E-16,-870.));
#37225=CARTESIAN_POINT('Origin',(1.75,0.5,-870.));
#37226=CARTESIAN_POINT('',(1.75,0.5,30.));
#37227=CARTESIAN_POINT('Origin',(0.,0.,-870.));
#37228=CARTESIAN_POINT('',(-11.5,1.00000000000001,-870.));
#37229=CARTESIAN_POINT('',(-10.5,-1.28587913910472E-15,-870.));
#37230=CARTESIAN_POINT('',(-11.5,5.8257864376269,-870.));
#37231=CARTESIAN_POINT('',(-11.5,1.00000000000001,-870.));
#37232=CARTESIAN_POINT('',(-11.2071067811865,6.53289321881345,-870.));
#37233=CARTESIAN_POINT('Origin',(-10.5,5.8257864376269,-870.));
#37234=CARTESIAN_POINT('',(-8.19644660940673,9.54355339059324,-870.));
#37235=CARTESIAN_POINT('',(-11.5,6.24,-870.));
#37236=CARTESIAN_POINT('',(-8.05,9.89710678118652,-870.));
#37237=CARTESIAN_POINT('Origin',(-8.55,9.89710678118652,-870.));
#37238=CARTESIAN_POINT('',(-8.05,13.5928932188135,-870.));
#37239=CARTESIAN_POINT('',(-8.05,9.68999999999997,-870.));
#37240=CARTESIAN_POINT('',(-8.19644660940672,13.9464466094067,-870.));
#37241=CARTESIAN_POINT('Origin',(-8.55,13.5928932188135,-870.));
#37242=CARTESIAN_POINT('',(-8.57259699813414,14.3225969981341,-870.));
#37243=CARTESIAN_POINT('',(-8.05,13.8,-870.));
#37244=CARTESIAN_POINT('',(-8.71475010619428,14.6107663907404,-870.));
#37245=CARTESIAN_POINT('Origin',(-8.21904360754086,14.6761503887274,-870.));
#37246=CARTESIAN_POINT('',(-10.6942336092596,16.5902498938057,-870.));
#37247=CARTESIAN_POINT('Origin',(-10.995,14.31,-870.));
#37248=CARTESIAN_POINT('',(-10.9824030018658,16.7324030018659,-870.));
#37249=CARTESIAN_POINT('Origin',(-10.6288496112726,17.0859563924591,-870.));
#37250=CARTESIAN_POINT('',(-11.3535533905933,17.1035533905933,-870.));
#37251=CARTESIAN_POINT('',(-8.05,13.8,-870.));
#37252=CARTESIAN_POINT('',(-11.5,17.4571067811866,-870.));
#37253=CARTESIAN_POINT('Origin',(-11.,17.4571067811866,-870.));
#37254=CARTESIAN_POINT('',(-11.5,18.3428932188135,-870.));
#37255=CARTESIAN_POINT('',(-11.5,18.55,-870.));
#37256=CARTESIAN_POINT('',(-11.3535533905933,18.6964466094068,-870.));
#37257=CARTESIAN_POINT('Origin',(-11.,18.3428932188135,-870.));
#37258=CARTESIAN_POINT('',(-10.9824030018659,19.0675969981341,-870.));
#37259=CARTESIAN_POINT('',(-8.05,22.,-870.));
#37260=CARTESIAN_POINT('',(-10.6942336092596,19.2097501061943,-870.));
#37261=CARTESIAN_POINT('Origin',(-10.6288496112726,18.7140436075409,-870.));
#37262=CARTESIAN_POINT('',(-8.71475010619428,21.1892336092596,-870.));
#37263=CARTESIAN_POINT('Origin',(-10.995,21.49,-870.));
#37264=CARTESIAN_POINT('',(-8.57259699813413,21.4774030018659,-870.));
#37265=CARTESIAN_POINT('Origin',(-8.21904360754086,21.1238496112726,-870.));
#37266=CARTESIAN_POINT('',(-8.05,22.,-870.));
#37267=CARTESIAN_POINT('',(-8.05,22.,-870.));
#37268=CARTESIAN_POINT('',(8.05,22.,-870.));
#37269=CARTESIAN_POINT('',(-8.05,22.,-870.));
#37270=CARTESIAN_POINT('',(8.57259699813413,21.4774030018659,-870.));
#37271=CARTESIAN_POINT('',(8.05,22.,-870.));
#37272=CARTESIAN_POINT('',(8.71475010619428,21.1892336092596,-870.));
#37273=CARTESIAN_POINT('Origin',(8.21904360754086,21.1238496112726,-870.));
#37274=CARTESIAN_POINT('',(10.6942336092596,19.2097501061943,-870.));
#37275=CARTESIAN_POINT('Origin',(10.995,21.49,-870.));
#37276=CARTESIAN_POINT('',(10.9824030018659,19.0675969981341,-870.));
#37277=CARTESIAN_POINT('Origin',(10.6288496112726,18.7140436075409,-870.));
#37278=CARTESIAN_POINT('',(11.3535533905933,18.6964466094068,-870.));
#37279=CARTESIAN_POINT('',(8.05,22.,-870.));
#37280=CARTESIAN_POINT('',(11.5,18.3428932188135,-870.));
#37281=CARTESIAN_POINT('Origin',(11.,18.3428932188135,-870.));
#37282=CARTESIAN_POINT('',(11.5,17.4571067811866,-870.));
#37283=CARTESIAN_POINT('',(11.5,18.55,-870.));
#37284=CARTESIAN_POINT('',(11.3535533905933,17.1035533905933,-870.));
#37285=CARTESIAN_POINT('Origin',(11.,17.4571067811866,-870.));
#37286=CARTESIAN_POINT('',(10.9824030018658,16.7324030018659,-870.));
#37287=CARTESIAN_POINT('',(8.05,13.8,-870.));
#37288=CARTESIAN_POINT('',(10.6942336092596,16.5902498938057,-870.));
#37289=CARTESIAN_POINT('Origin',(10.6288496112726,17.0859563924591,-870.));
#37290=CARTESIAN_POINT('',(8.71475010619428,14.6107663907404,-870.));
#37291=CARTESIAN_POINT('Origin',(10.995,14.31,-870.));
#37292=CARTESIAN_POINT('',(8.57259699813414,14.3225969981341,-870.));
#37293=CARTESIAN_POINT('Origin',(8.21904360754086,14.6761503887274,-870.));
#37294=CARTESIAN_POINT('',(8.19644660940672,13.9464466094067,-870.));
#37295=CARTESIAN_POINT('',(8.05,13.8,-870.));
#37296=CARTESIAN_POINT('',(8.05,13.5928932188135,-870.));
#37297=CARTESIAN_POINT('Origin',(8.55,13.5928932188135,-870.));
#37298=CARTESIAN_POINT('',(8.05,9.89710678118651,-870.));
#37299=CARTESIAN_POINT('',(8.05,9.68999999999997,-870.));
#37300=CARTESIAN_POINT('',(8.19644660940673,9.54355339059324,-870.));
#37301=CARTESIAN_POINT('Origin',(8.55,9.89710678118651,-870.));
#37302=CARTESIAN_POINT('',(11.2071067811865,6.53289321881345,-870.));
#37303=CARTESIAN_POINT('',(11.5,6.24,-870.));
#37304=CARTESIAN_POINT('',(11.5,5.8257864376269,-870.));
#37305=CARTESIAN_POINT('Origin',(10.5,5.8257864376269,-870.));
#37306=CARTESIAN_POINT('',(11.5,1.00000000000001,-870.));
#37307=CARTESIAN_POINT('',(11.5,1.00000000000001,-870.));
#37308=CARTESIAN_POINT('',(10.5,-1.28587913910472E-15,-870.));
#37309=CARTESIAN_POINT('',(1.75,0.5,-870.));
#37310=CARTESIAN_POINT('',(1.75,0.5,-870.));
#37311=CARTESIAN_POINT('',(-1.75,0.5,-870.));
#37312=CARTESIAN_POINT('Origin',(0.,0.,30.));
#37313=CARTESIAN_POINT('',(-2.25,-1.4389599889981E-16,30.));
#37314=CARTESIAN_POINT('',(11.5,1.00000000000001,30.));
#37315=CARTESIAN_POINT('',(10.5,-1.28587913910472E-15,30.));
#37316=CARTESIAN_POINT('',(11.5,5.8257864376269,30.));
#37317=CARTESIAN_POINT('',(11.5,1.00000000000001,30.));
#37318=CARTESIAN_POINT('',(11.2071067811865,6.53289321881345,30.));
#37319=CARTESIAN_POINT('Origin',(10.5,5.8257864376269,30.));
#37320=CARTESIAN_POINT('',(8.19644660940673,9.54355339059324,30.));
#37321=CARTESIAN_POINT('',(11.5,6.24,30.));
#37322=CARTESIAN_POINT('',(8.05,9.89710678118651,30.));
#37323=CARTESIAN_POINT('Origin',(8.55,9.89710678118651,30.));
#37324=CARTESIAN_POINT('',(8.05,13.5928932188135,30.));
#37325=CARTESIAN_POINT('',(8.05,9.68999999999997,30.));
#37326=CARTESIAN_POINT('',(8.19644660940672,13.9464466094067,30.));
#37327=CARTESIAN_POINT('Origin',(8.55,13.5928932188135,30.));
#37328=CARTESIAN_POINT('',(8.57259699813414,14.3225969981341,30.));
#37329=CARTESIAN_POINT('',(8.05,13.8,30.));
#37330=CARTESIAN_POINT('',(8.71475010619428,14.6107663907404,30.));
#37331=CARTESIAN_POINT('Origin',(8.21904360754086,14.6761503887274,30.));
#37332=CARTESIAN_POINT('',(10.6942336092596,16.5902498938057,30.));
#37333=CARTESIAN_POINT('Origin',(10.995,14.31,30.));
#37334=CARTESIAN_POINT('',(10.9824030018658,16.7324030018659,30.));
#37335=CARTESIAN_POINT('Origin',(10.6288496112726,17.0859563924591,30.));
#37336=CARTESIAN_POINT('',(11.3535533905933,17.1035533905933,30.));
#37337=CARTESIAN_POINT('',(8.05,13.8,30.));
#37338=CARTESIAN_POINT('',(11.5,17.4571067811866,30.));
#37339=CARTESIAN_POINT('Origin',(11.,17.4571067811866,30.));
#37340=CARTESIAN_POINT('',(11.5,18.3428932188135,30.));
#37341=CARTESIAN_POINT('',(11.5,18.55,30.));
#37342=CARTESIAN_POINT('',(11.3535533905933,18.6964466094068,30.));
#37343=CARTESIAN_POINT('Origin',(11.,18.3428932188135,30.));
#37344=CARTESIAN_POINT('',(10.9824030018659,19.0675969981341,30.));
#37345=CARTESIAN_POINT('',(8.05,22.,30.));
#37346=CARTESIAN_POINT('',(10.6942336092596,19.2097501061943,30.));
#37347=CARTESIAN_POINT('Origin',(10.6288496112726,18.7140436075409,30.));
#37348=CARTESIAN_POINT('',(8.71475010619428,21.1892336092596,30.));
#37349=CARTESIAN_POINT('Origin',(10.995,21.49,30.));
#37350=CARTESIAN_POINT('',(8.57259699813413,21.4774030018659,30.));
#37351=CARTESIAN_POINT('Origin',(8.21904360754086,21.1238496112726,30.));
#37352=CARTESIAN_POINT('',(8.05,22.,30.));
#37353=CARTESIAN_POINT('',(8.05,22.,30.));
#37354=CARTESIAN_POINT('',(-8.05,22.,30.));
#37355=CARTESIAN_POINT('',(-8.05,22.,30.));
#37356=CARTESIAN_POINT('',(-8.57259699813413,21.4774030018659,30.));
#37357=CARTESIAN_POINT('',(-8.05,22.,30.));
#37358=CARTESIAN_POINT('',(-8.71475010619428,21.1892336092596,30.));
#37359=CARTESIAN_POINT('Origin',(-8.21904360754086,21.1238496112726,30.));
#37360=CARTESIAN_POINT('',(-10.6942336092596,19.2097501061943,30.));
#37361=CARTESIAN_POINT('Origin',(-10.995,21.49,30.));
#37362=CARTESIAN_POINT('',(-10.9824030018659,19.0675969981341,30.));
#37363=CARTESIAN_POINT('Origin',(-10.6288496112726,18.7140436075409,30.));
#37364=CARTESIAN_POINT('',(-11.3535533905933,18.6964466094068,30.));
#37365=CARTESIAN_POINT('',(-8.05,22.,30.));
#37366=CARTESIAN_POINT('',(-11.5,18.3428932188135,30.));
#37367=CARTESIAN_POINT('Origin',(-11.,18.3428932188135,30.));
#37368=CARTESIAN_POINT('',(-11.5,17.4571067811866,30.));
#37369=CARTESIAN_POINT('',(-11.5,18.55,30.));
#37370=CARTESIAN_POINT('',(-11.3535533905933,17.1035533905933,30.));
#37371=CARTESIAN_POINT('Origin',(-11.,17.4571067811866,30.));
#37372=CARTESIAN_POINT('',(-10.9824030018658,16.7324030018659,30.));
#37373=CARTESIAN_POINT('',(-8.05,13.8,30.));
#37374=CARTESIAN_POINT('',(-10.6942336092596,16.5902498938057,30.));
#37375=CARTESIAN_POINT('Origin',(-10.6288496112726,17.0859563924591,30.));
#37376=CARTESIAN_POINT('',(-8.71475010619428,14.6107663907404,30.));
#37377=CARTESIAN_POINT('Origin',(-10.995,14.31,30.));
#37378=CARTESIAN_POINT('',(-8.57259699813414,14.3225969981341,30.));
#37379=CARTESIAN_POINT('Origin',(-8.21904360754086,14.6761503887274,30.));
#37380=CARTESIAN_POINT('',(-8.19644660940672,13.9464466094067,30.));
#37381=CARTESIAN_POINT('',(-8.05,13.8,30.));
#37382=CARTESIAN_POINT('',(-8.05,13.5928932188135,30.));
#37383=CARTESIAN_POINT('Origin',(-8.55,13.5928932188135,30.));
#37384=CARTESIAN_POINT('',(-8.05,9.89710678118652,30.));
#37385=CARTESIAN_POINT('',(-8.05,9.68999999999997,30.));
#37386=CARTESIAN_POINT('',(-8.19644660940673,9.54355339059324,30.));
#37387=CARTESIAN_POINT('Origin',(-8.55,9.89710678118652,30.));
#37388=CARTESIAN_POINT('',(-11.2071067811865,6.53289321881345,30.));
#37389=CARTESIAN_POINT('',(-11.5,6.24,30.));
#37390=CARTESIAN_POINT('',(-11.5,5.8257864376269,30.));
#37391=CARTESIAN_POINT('Origin',(-10.5,5.8257864376269,30.));
#37392=CARTESIAN_POINT('',(-11.5,1.00000000000001,30.));
#37393=CARTESIAN_POINT('',(-11.5,1.00000000000001,30.));
#37394=CARTESIAN_POINT('',(-10.5,-1.28587913910472E-15,30.));
#37395=CARTESIAN_POINT('Origin',(8.05,13.8,-870.));
#37396=CARTESIAN_POINT('',(8.19644660940672,13.9464466094067,-870.));
#37397=CARTESIAN_POINT('',(8.57259699813414,14.3225969981341,30.));
#37398=CARTESIAN_POINT('Origin',(8.05,13.8,-870.));
#37399=CARTESIAN_POINT('',(11.3535533905933,17.1035533905933,-870.));
#37400=CARTESIAN_POINT('',(10.9824030018658,16.7324030018659,-870.));
#37401=CARTESIAN_POINT('Origin',(8.05,22.,-870.));
#37402=CARTESIAN_POINT('',(10.9824030018659,19.0675969981341,30.));
#37403=CARTESIAN_POINT('',(11.3535533905933,18.6964466094068,-870.));
#37404=CARTESIAN_POINT('Origin',(8.05,22.,-870.));
#37405=CARTESIAN_POINT('',(8.57259699813413,21.4774030018659,-870.));
#37406=CARTESIAN_POINT('',(8.05,22.,-870.));
#37407=CARTESIAN_POINT('Origin',(-8.05,13.8,-870.));
#37408=CARTESIAN_POINT('',(-8.19644660940672,13.9464466094067,30.));
#37409=CARTESIAN_POINT('',(-8.57259699813414,14.3225969981341,-870.));
#37410=CARTESIAN_POINT('Origin',(-8.05,22.,-870.));
#37411=CARTESIAN_POINT('',(-10.9824030018659,19.0675969981341,-870.));
#37412=CARTESIAN_POINT('',(-11.3535533905933,18.6964466094068,-870.));
#37413=CARTESIAN_POINT('Origin',(-8.05,22.,-870.));
#37414=CARTESIAN_POINT('',(-8.05,22.,-870.));
#37415=CARTESIAN_POINT('Origin',(-10.5,-1.28587913910472E-15,-870.));
#37416=CARTESIAN_POINT('',(-11.5,1.00000000000001,-870.));
#37417=CARTESIAN_POINT('Origin',(-11.5,1.00000000000001,-870.));
#37418=CARTESIAN_POINT('',(-11.5,5.8257864376269,-870.));
#37419=CARTESIAN_POINT('Origin',(-11.5,6.24,-870.));
#37420=CARTESIAN_POINT('',(-11.2071067811865,6.53289321881345,-870.));
#37421=CARTESIAN_POINT('',(-8.19644660940673,9.54355339059324,-870.));
#37422=CARTESIAN_POINT('Origin',(-8.05,9.68999999999997,-870.));
#37423=CARTESIAN_POINT('',(-8.05,9.89710678118652,30.));
#37424=CARTESIAN_POINT('',(-8.05,13.5928932188135,-870.));
#37425=CARTESIAN_POINT('Origin',(-8.05,13.8,-870.));
#37426=CARTESIAN_POINT('',(-11.3535533905933,17.1035533905933,-870.));
#37427=CARTESIAN_POINT('',(-10.9824030018658,16.7324030018659,30.));
#37428=CARTESIAN_POINT('Origin',(-11.5,18.55,-870.));
#37429=CARTESIAN_POINT('',(-11.5,18.3428932188135,-870.));
#37430=CARTESIAN_POINT('',(-11.5,17.4571067811866,-870.));
#37431=CARTESIAN_POINT('Origin',(-8.05,22.,-870.));
#37432=CARTESIAN_POINT('',(-8.57259699813413,21.4774030018659,30.));
#37433=CARTESIAN_POINT('Origin',(-10.995,21.49,-870.));
#37434=CARTESIAN_POINT('',(-10.6942336092596,19.2097501061943,-870.));
#37435=CARTESIAN_POINT('',(-8.71475010619428,21.1892336092596,-870.));
#37436=CARTESIAN_POINT('Origin',(-10.995,14.31,-870.));
#37437=CARTESIAN_POINT('',(-10.6942336092596,16.5902498938057,-870.));
#37438=CARTESIAN_POINT('',(-8.71475010619428,14.6107663907404,-870.));
#37439=CARTESIAN_POINT('Origin',(-10.6288496112726,18.7140436075409,-870.));
#37440=CARTESIAN_POINT('Origin',(-11.,18.3428932188135,-870.));
#37441=CARTESIAN_POINT('Origin',(-11.,17.4571067811866,-870.));
#37442=CARTESIAN_POINT('Origin',(-10.6288496112726,17.0859563924591,-870.));
#37443=CARTESIAN_POINT('Origin',(-8.55,9.89710678118652,-870.));
#37444=CARTESIAN_POINT('Origin',(-8.55,13.5928932188135,-870.));
#37445=CARTESIAN_POINT('Origin',(-8.21904360754086,14.6761503887274,-870.));
#37446=CARTESIAN_POINT('Origin',(-8.21904360754086,21.1238496112726,-870.));
#37447=CARTESIAN_POINT('Origin',(-10.5,5.8257864376269,-870.));
#37448=CARTESIAN_POINT('Origin',(11.5,18.55,-870.));
#37449=CARTESIAN_POINT('',(11.5,18.3428932188135,-870.));
#37450=CARTESIAN_POINT('',(11.5,17.4571067811866,-870.));
#37451=CARTESIAN_POINT('Origin',(8.05,9.68999999999997,-870.));
#37452=CARTESIAN_POINT('',(8.05,9.89710678118651,-870.));
#37453=CARTESIAN_POINT('',(8.05,13.5928932188135,30.));
#37454=CARTESIAN_POINT('Origin',(11.5,6.24,-870.));
#37455=CARTESIAN_POINT('',(11.2071067811865,6.53289321881345,-870.));
#37456=CARTESIAN_POINT('',(8.19644660940673,9.54355339059324,30.));
#37457=CARTESIAN_POINT('Origin',(11.5,1.00000000000001,-870.));
#37458=CARTESIAN_POINT('',(11.5,5.8257864376269,-870.));
#37459=CARTESIAN_POINT('',(11.5,1.00000000000001,-870.));
#37460=CARTESIAN_POINT('Origin',(10.5,-1.28587913910472E-15,-870.));
#37461=CARTESIAN_POINT('Origin',(10.995,21.49,-870.));
#37462=CARTESIAN_POINT('',(10.6942336092596,19.2097501061943,-870.));
#37463=CARTESIAN_POINT('',(8.71475010619428,21.1892336092596,-870.));
#37464=CARTESIAN_POINT('Origin',(10.995,14.31,-870.));
#37465=CARTESIAN_POINT('',(10.6942336092596,16.5902498938057,-870.));
#37466=CARTESIAN_POINT('',(8.71475010619428,14.6107663907404,-870.));
#37467=CARTESIAN_POINT('Origin',(10.6288496112726,18.7140436075409,-870.));
#37468=CARTESIAN_POINT('Origin',(11.,18.3428932188135,-870.));
#37469=CARTESIAN_POINT('Origin',(11.,17.4571067811866,-870.));
#37470=CARTESIAN_POINT('Origin',(10.6288496112726,17.0859563924591,-870.));
#37471=CARTESIAN_POINT('Origin',(8.55,9.89710678118651,-870.));
#37472=CARTESIAN_POINT('Origin',(8.55,13.5928932188135,-870.));
#37473=CARTESIAN_POINT('Origin',(8.21904360754086,14.6761503887274,-870.));
#37474=CARTESIAN_POINT('Origin',(8.21904360754086,21.1238496112726,-870.));
#37475=CARTESIAN_POINT('Origin',(10.5,5.8257864376269,-870.));
#37476=CARTESIAN_POINT('Origin',(-2.25,-1.4389599889981E-16,-870.));
#37477=CARTESIAN_POINT('Origin',(-1.75,0.5,-870.));
#37478=CARTESIAN_POINT('',(1.75,0.5,-870.));
#37479=CARTESIAN_POINT('Origin',(1.75,0.5,-870.));
#37480=CARTESIAN_POINT('Origin',(3.5,13.,0.));
#37481=CARTESIAN_POINT('Origin',(3.5,13.,-60.));
#37482=CARTESIAN_POINT('Origin',(3.5,13.,-120.));
#37483=CARTESIAN_POINT('Origin',(3.5,13.,-180.));
#37484=CARTESIAN_POINT('Origin',(3.5,13.,-240.));
#37485=CARTESIAN_POINT('Origin',(3.5,13.,-300.));
#37486=CARTESIAN_POINT('Origin',(3.5,13.,-360.));
#37487=CARTESIAN_POINT('Origin',(3.5,13.,-420.));
#37488=CARTESIAN_POINT('Origin',(3.5,13.,-480.));
#37489=CARTESIAN_POINT('Origin',(3.5,13.,-540.));
#37490=CARTESIAN_POINT('Origin',(3.5,13.,-600.));
#37491=CARTESIAN_POINT('Origin',(3.5,13.,-660.));
#37492=CARTESIAN_POINT('Origin',(3.5,13.,-720.));
#37493=CARTESIAN_POINT('Origin',(3.5,13.,-780.));
#37494=CARTESIAN_POINT('Origin',(3.5,13.,-840.));
#37495=CARTESIAN_POINT('',(0.,0.,0.));
#37496=CARTESIAN_POINT('Origin',(23.2,9.00000000000001,-77.4));
#37497=CARTESIAN_POINT('',(17.28,9.00000000000001,-74.9));
#37498=CARTESIAN_POINT('Origin',(17.28,9.00000000000001,-77.4));
#37499=CARTESIAN_POINT('',(23.2,9.00000000000001,-74.9));
#37500=CARTESIAN_POINT('',(23.2,9.00000000000001,-74.9));
#37501=CARTESIAN_POINT('Origin',(23.2,9.00000000000001,-77.4));
#37502=CARTESIAN_POINT('Origin',(-23.2,9.00000000000001,-77.4));
#37503=CARTESIAN_POINT('',(-17.28,9.00000000000001,-79.9));
#37504=CARTESIAN_POINT('Origin',(-17.28,9.00000000000001,-77.4));
#37505=CARTESIAN_POINT('',(-23.2,9.00000000000001,-79.9));
#37506=CARTESIAN_POINT('',(-23.2,9.00000000000001,-79.9));
#37507=CARTESIAN_POINT('Origin',(-23.2,9.00000000000001,-77.4));
#37508=CARTESIAN_POINT('Origin',(-1.54689479616415E-14,13.,-76.7));
#37509=CARTESIAN_POINT('',(3.64999999999998,13.,-76.7));
#37510=CARTESIAN_POINT('Origin',(-1.54689479616415E-14,13.,-76.7));
#37511=CARTESIAN_POINT('',(3.64999999999998,13.8,-76.7));
#37512=CARTESIAN_POINT('',(3.64999999999998,13.,-76.7));
#37513=CARTESIAN_POINT('Origin',(-1.65097820472275E-14,13.8,-76.7));
#37514=CARTESIAN_POINT('Origin',(17.28,9.00000000000001,-77.4));
#37515=CARTESIAN_POINT('',(15.7778484524311,9.,-77.4));
#37516=CARTESIAN_POINT('',(17.28,9.00000000000001,-74.9));
#37517=CARTESIAN_POINT('Origin',(-17.28,9.00000000000001,-77.4));
#37518=CARTESIAN_POINT('',(-15.7778484524311,9.,-77.4));
#37519=CARTESIAN_POINT('',(-17.28,9.00000000000001,-79.9));
#37520=CARTESIAN_POINT('Origin',(28.5,14.,-64.9));
#37521=CARTESIAN_POINT('',(28.5,0.500000000000005,-68.2235));
#37522=CARTESIAN_POINT('Origin',(28.5,0.500000000000006,-64.9));
#37523=CARTESIAN_POINT('',(28.5,14.,-68.2235));
#37524=CARTESIAN_POINT('',(28.5,14.,-68.2235));
#37525=CARTESIAN_POINT('Origin',(28.5,14.,-64.9));
#37526=CARTESIAN_POINT('Origin',(28.5,14.,-19.9));
#37527=CARTESIAN_POINT('',(28.5,0.500000000000005,-23.2235));
#37528=CARTESIAN_POINT('Origin',(28.5,0.500000000000006,-19.9));
#37529=CARTESIAN_POINT('',(28.5,14.,-23.2235));
#37530=CARTESIAN_POINT('',(28.5,14.,-23.2235));
#37531=CARTESIAN_POINT('Origin',(28.5,14.,-19.9));
#37532=CARTESIAN_POINT('Origin',(-28.5,14.,-64.9));
#37533=CARTESIAN_POINT('',(-28.5,0.500000000000005,-68.2235));
#37534=CARTESIAN_POINT('Origin',(-28.5,0.500000000000006,-64.9));
#37535=CARTESIAN_POINT('',(-28.5,14.,-68.2235));
#37536=CARTESIAN_POINT('',(-28.5,14.,-68.2235));
#37537=CARTESIAN_POINT('Origin',(-28.5,14.,-64.9));
#37538=CARTESIAN_POINT('Origin',(-28.5,14.,-19.9));
#37539=CARTESIAN_POINT('',(-28.5,0.500000000000003,-23.2235));
#37540=CARTESIAN_POINT('Origin',(-28.5,0.500000000000004,-19.9));
#37541=CARTESIAN_POINT('',(-28.5,14.,-23.2235));
#37542=CARTESIAN_POINT('',(-28.5,14.,-23.2235));
#37543=CARTESIAN_POINT('Origin',(-28.5,14.,-19.9));
#37544=CARTESIAN_POINT('Origin',(-23.2,9.00000000000001,-7.4));
#37545=CARTESIAN_POINT('',(-17.28,9.00000000000001,-9.9));
#37546=CARTESIAN_POINT('Origin',(-17.28,9.00000000000001,-7.4));
#37547=CARTESIAN_POINT('',(-23.2,9.00000000000001,-9.9));
#37548=CARTESIAN_POINT('',(-23.2,9.00000000000001,-9.9));
#37549=CARTESIAN_POINT('Origin',(-23.2,9.00000000000001,-7.4));
#37550=CARTESIAN_POINT('Origin',(23.2,9.00000000000001,-7.4));
#37551=CARTESIAN_POINT('',(17.28,9.00000000000001,-4.90000000000001));
#37552=CARTESIAN_POINT('Origin',(17.28,9.00000000000001,-7.4));
#37553=CARTESIAN_POINT('',(23.2,9.00000000000001,-4.90000000000001));
#37554=CARTESIAN_POINT('',(23.2,9.00000000000001,-4.90000000000001));
#37555=CARTESIAN_POINT('Origin',(23.2,9.00000000000001,-7.4));
#37556=CARTESIAN_POINT('Origin',(-1.54689479616415E-14,13.,-8.1));
#37557=CARTESIAN_POINT('',(3.64999999999998,13.,-8.1));
#37558=CARTESIAN_POINT('Origin',(-1.54689479616415E-14,13.,-8.1));
#37559=CARTESIAN_POINT('',(3.64999999999998,13.8,-8.1));
#37560=CARTESIAN_POINT('',(3.64999999999998,13.,-8.1));
#37561=CARTESIAN_POINT('Origin',(-1.65097820472275E-14,13.8,-8.1));
#37562=CARTESIAN_POINT('Origin',(-1.90276438129354E-14,12.7,-74.2));
#37563=CARTESIAN_POINT('',(0.499999999999987,12.5,-74.2));
#37564=CARTESIAN_POINT('Origin',(-1.87674352915389E-14,12.5,-74.2));
#37565=CARTESIAN_POINT('',(0.499999999999987,12.7,-74.2));
#37566=CARTESIAN_POINT('',(0.499999999999987,12.7,-74.2));
#37567=CARTESIAN_POINT('',(-0.500000000000023,12.7,-74.2));
#37568=CARTESIAN_POINT('Origin',(-1.90276438129354E-14,12.7,-74.2));
#37569=CARTESIAN_POINT('',(-0.500000000000025,13.,-74.2));
#37570=CARTESIAN_POINT('',(-0.500000000000025,12.7,-74.2));
#37571=CARTESIAN_POINT('',(0.499999999999986,13.,-74.2));
#37572=CARTESIAN_POINT('Origin',(-1.94179565950302E-14,13.,-74.2));
#37573=CARTESIAN_POINT('',(0.499999999999987,12.7,-74.2));
#37574=CARTESIAN_POINT('Origin',(-17.28,9.00000000000001,-7.4));
#37575=CARTESIAN_POINT('',(-15.7778484524311,9.,-7.4));
#37576=CARTESIAN_POINT('',(-17.28,9.00000000000001,-9.9));
#37577=CARTESIAN_POINT('Origin',(17.28,9.00000000000001,-7.4));
#37578=CARTESIAN_POINT('',(15.7778484524311,9.,-7.4));
#37579=CARTESIAN_POINT('',(17.28,9.00000000000001,-4.90000000000001));
#37580=CARTESIAN_POINT('Origin',(-1.65232411086791E-14,12.7,-10.6));
#37581=CARTESIAN_POINT('',(0.499999999999984,12.5,-10.6));
#37582=CARTESIAN_POINT('Origin',(-1.62630325872826E-14,12.5,-10.6));
#37583=CARTESIAN_POINT('',(0.499999999999984,12.7,-10.6));
#37584=CARTESIAN_POINT('',(0.499999999999984,12.7,-10.6));
#37585=CARTESIAN_POINT('',(0.499999999999983,13.,-10.6));
#37586=CARTESIAN_POINT('',(0.499999999999984,12.7,-10.6));
#37587=CARTESIAN_POINT('',(-0.500000000000017,13.,-10.6));
#37588=CARTESIAN_POINT('Origin',(-1.69135538907739E-14,13.,-10.6));
#37589=CARTESIAN_POINT('',(-0.500000000000017,12.7,-10.6));
#37590=CARTESIAN_POINT('',(-0.500000000000017,12.7,-10.6));
#37591=CARTESIAN_POINT('Origin',(-1.65232411086791E-14,12.7,-10.6));
#37592=CARTESIAN_POINT('Ctrl Pts',(4.,8.,-84.5));
#37593=CARTESIAN_POINT('Ctrl Pts',(4.,4.,-84.5));
#37594=CARTESIAN_POINT('Ctrl Pts',(0.,4.,-84.5));
#37595=CARTESIAN_POINT('Ctrl Pts',(-4.,4.,-84.5));
#37596=CARTESIAN_POINT('Ctrl Pts',(-4.,8.,-84.5));
#37597=CARTESIAN_POINT('Ctrl Pts',(-4.,12.,-84.5));
#37598=CARTESIAN_POINT('Ctrl Pts',(0.,12.,-84.5));
#37599=CARTESIAN_POINT('Ctrl Pts',(4.,12.,-84.5));
#37600=CARTESIAN_POINT('Ctrl Pts',(4.,8.,-84.5));
#37601=CARTESIAN_POINT('Ctrl Pts',(4.,8.,-86.5172334444062));
#37602=CARTESIAN_POINT('Ctrl Pts',(4.,4.,-86.5172334444062));
#37603=CARTESIAN_POINT('Ctrl Pts',(0.,4.,-86.5172334444062));
#37604=CARTESIAN_POINT('Ctrl Pts',(-4.,4.,-86.5172334444062));
#37605=CARTESIAN_POINT('Ctrl Pts',(-4.,8.,-86.5172334444062));
#37606=CARTESIAN_POINT('Ctrl Pts',(-4.,12.,-86.5172334444062));
#37607=CARTESIAN_POINT('Ctrl Pts',(0.,12.,-86.5172334444062));
#37608=CARTESIAN_POINT('Ctrl Pts',(4.,12.,-86.5172334444062));
#37609=CARTESIAN_POINT('Ctrl Pts',(4.,8.,-86.5172334444062));
#37610=CARTESIAN_POINT('Ctrl Pts',(2.,8.,-86.7803508501983));
#37611=CARTESIAN_POINT('Ctrl Pts',(2.,6.,-86.7803508501983));
#37612=CARTESIAN_POINT('Ctrl Pts',(0.,6.,-86.7803508501983));
#37613=CARTESIAN_POINT('Ctrl Pts',(-2.,6.,-86.7803508501983));
#37614=CARTESIAN_POINT('Ctrl Pts',(-2.,8.,-86.7803508501983));
#37615=CARTESIAN_POINT('Ctrl Pts',(-2.,10.,-86.7803508501983));
#37616=CARTESIAN_POINT('Ctrl Pts',(0.,10.,-86.7803508501983));
#37617=CARTESIAN_POINT('Ctrl Pts',(2.,10.,-86.7803508501983));
#37618=CARTESIAN_POINT('Ctrl Pts',(2.,8.,-86.7803508501983));
#37619=CARTESIAN_POINT('',(-1.15470053837925,6.,-86.7177985317981));
#37620=CARTESIAN_POINT('',(-2.3094010767585,8.,-86.7177985317981));
#37621=CARTESIAN_POINT('Ctrl Pts',(-1.15470053837925,6.,-86.7177985317981));
#37622=CARTESIAN_POINT('Ctrl Pts',(-1.16052376017366,6.01008611601166,-86.7193986219689));
#37623=CARTESIAN_POINT('Ctrl Pts',(-1.16635206467311,6.02018103552669,-86.7209572835343));
#37624=CARTESIAN_POINT('Ctrl Pts',(-1.36167110655042,6.35848353974387,-86.7717992509189));
#37625=CARTESIAN_POINT('Ctrl Pts',(-1.5557141858025,6.69457601186558,-86.7803508501983));
#37626=CARTESIAN_POINT('Ctrl Pts',(-1.90838742933526,7.30542398813443,-86.7803508501983));
#37627=CARTESIAN_POINT('Ctrl Pts',(-2.10243050858733,7.64151646025614,-86.7717992509189));
#37628=CARTESIAN_POINT('Ctrl Pts',(-2.29774955046464,7.97981896447331,-86.7209572835343));
#37629=CARTESIAN_POINT('Ctrl Pts',(-2.3035778549641,7.98991388398835,-86.7193986219689));
#37630=CARTESIAN_POINT('Ctrl Pts',(-2.30940107675851,8.00000000000001,-86.7177985317981));
#37631=CARTESIAN_POINT('',(1.15470053837925,6.,-86.7177985317981));
#37632=CARTESIAN_POINT('Ctrl Pts',(1.15470053837925,6.,-86.7177985317981));
#37633=CARTESIAN_POINT('Ctrl Pts',(1.14305409479044,6.,-86.7193986219689));
#37634=CARTESIAN_POINT('Ctrl Pts',(1.13139748579153,6.,-86.7209572835343));
#37635=CARTESIAN_POINT('Ctrl Pts',(0.740759402036912,6.,-86.7717992509189));
#37636=CARTESIAN_POINT('Ctrl Pts',(0.352673243532761,6.,-86.7803508501983));
#37637=CARTESIAN_POINT('Ctrl Pts',(-0.352673243532758,6.,-86.7803508501983));
#37638=CARTESIAN_POINT('Ctrl Pts',(-0.740759402036907,6.,-86.7717992509189));
#37639=CARTESIAN_POINT('Ctrl Pts',(-1.13139748579153,6.,-86.7209572835343));
#37640=CARTESIAN_POINT('Ctrl Pts',(-1.14305409479043,6.,-86.7193986219689));
#37641=CARTESIAN_POINT('Ctrl Pts',(-1.15470053837925,6.,-86.7177985317981));
#37642=CARTESIAN_POINT('',(2.3094010767585,8.,-86.7177985317981));
#37643=CARTESIAN_POINT('Ctrl Pts',(2.3094010767585,8.,-86.7177985317981));
#37644=CARTESIAN_POINT('Ctrl Pts',(2.30357785496409,7.98991388398834,-86.7193986219689));
#37645=CARTESIAN_POINT('Ctrl Pts',(2.29774955046465,7.97981896447331,-86.7209572835343));
#37646=CARTESIAN_POINT('Ctrl Pts',(2.10243050858733,7.64151646025614,-86.7717992509189));
#37647=CARTESIAN_POINT('Ctrl Pts',(1.90838742933526,7.30542398813443,-86.7803508501983));
#37648=CARTESIAN_POINT('Ctrl Pts',(1.5557141858025,6.69457601186558,-86.7803508501983));
#37649=CARTESIAN_POINT('Ctrl Pts',(1.36167110655042,6.35848353974387,-86.7717992509189));
#37650=CARTESIAN_POINT('Ctrl Pts',(1.16635206467311,6.02018103552669,-86.7209572835344));
#37651=CARTESIAN_POINT('Ctrl Pts',(1.16052376017366,6.01008611601166,-86.7193986219689));
#37652=CARTESIAN_POINT('Ctrl Pts',(1.15470053837925,6.00000000000001,-86.7177985317981));
#37653=CARTESIAN_POINT('',(4.,8.,-84.5));
#37654=CARTESIAN_POINT('Ctrl Pts',(2.3094010767585,8.,-86.7177985317981));
#37655=CARTESIAN_POINT('Ctrl Pts',(4.,8.,-86.2532600313803));
#37656=CARTESIAN_POINT('Ctrl Pts',(4.,8.,-84.5));
#37657=CARTESIAN_POINT('',(-4.,8.,-84.5));
#37658=CARTESIAN_POINT('Origin',(0.,8.,-84.5));
#37659=CARTESIAN_POINT('Origin',(0.,8.,-84.5));
#37660=CARTESIAN_POINT('',(1.15470053837925,10.,-86.7177985317981));
#37661=CARTESIAN_POINT('Ctrl Pts',(1.15470053837925,10.,-86.7177985317981));
#37662=CARTESIAN_POINT('Ctrl Pts',(1.16052376017366,9.98991388398835,-86.7193986219689));
#37663=CARTESIAN_POINT('Ctrl Pts',(1.16635206467311,9.97981896447332,-86.7209572835343));
#37664=CARTESIAN_POINT('Ctrl Pts',(1.36167110655042,9.64151646025614,-86.7717992509189));
#37665=CARTESIAN_POINT('Ctrl Pts',(1.5557141858025,9.30542398813443,-86.7803508501983));
#37666=CARTESIAN_POINT('Ctrl Pts',(1.90838742933526,8.69457601186558,-86.7803508501983));
#37667=CARTESIAN_POINT('Ctrl Pts',(2.10243050858733,8.35848353974387,-86.7717992509189));
#37668=CARTESIAN_POINT('Ctrl Pts',(2.29774955046465,8.02018103552669,-86.7209572835343));
#37669=CARTESIAN_POINT('Ctrl Pts',(2.3035778549641,8.01008611601166,-86.7193986219689));
#37670=CARTESIAN_POINT('Ctrl Pts',(2.30940107675851,8.,-86.7177985317981));
#37671=CARTESIAN_POINT('',(-1.15470053837925,10.,-86.7177985317981));
#37672=CARTESIAN_POINT('Ctrl Pts',(-1.15470053837925,10.,-86.7177985317981));
#37673=CARTESIAN_POINT('Ctrl Pts',(-1.14305409479043,10.,-86.7193986219689));
#37674=CARTESIAN_POINT('Ctrl Pts',(-1.13139748579153,10.,-86.7209572835343));
#37675=CARTESIAN_POINT('Ctrl Pts',(-0.740759402036911,10.,-86.7717992509189));
#37676=CARTESIAN_POINT('Ctrl Pts',(-0.352673243532759,10.,-86.7803508501983));
#37677=CARTESIAN_POINT('Ctrl Pts',(0.352673243532759,10.,-86.7803508501983));
#37678=CARTESIAN_POINT('Ctrl Pts',(0.740759402036911,10.,-86.7717992509189));
#37679=CARTESIAN_POINT('Ctrl Pts',(1.13139748579153,10.,-86.7209572835343));
#37680=CARTESIAN_POINT('Ctrl Pts',(1.14305409479044,10.,-86.7193986219689));
#37681=CARTESIAN_POINT('Ctrl Pts',(1.15470053837925,10.,-86.7177985317981));
#37682=CARTESIAN_POINT('Ctrl Pts',(-2.3094010767585,8.,-86.7177985317981));
#37683=CARTESIAN_POINT('Ctrl Pts',(-2.3035778549641,8.01008611601166,-86.7193986219689));
#37684=CARTESIAN_POINT('Ctrl Pts',(-2.29774955046464,8.02018103552669,-86.7209572835343));
#37685=CARTESIAN_POINT('Ctrl Pts',(-2.10243050858733,8.35848353974387,-86.7717992509189));
#37686=CARTESIAN_POINT('Ctrl Pts',(-1.90838742933526,8.69457601186558,-86.7803508501983));
#37687=CARTESIAN_POINT('Ctrl Pts',(-1.5557141858025,9.30542398813443,-86.7803508501983));
#37688=CARTESIAN_POINT('Ctrl Pts',(-1.36167110655042,9.64151646025614,-86.7717992509189));
#37689=CARTESIAN_POINT('Ctrl Pts',(-1.16635206467311,9.97981896447332,-86.7209572835343));
#37690=CARTESIAN_POINT('Ctrl Pts',(-1.16052376017366,9.98991388398835,-86.7193986219689));
#37691=CARTESIAN_POINT('Ctrl Pts',(-1.15470053837925,10.,-86.7177985317981));
#37692=CARTESIAN_POINT('Origin',(0.,8.,-86.8));
#37693=CARTESIAN_POINT('',(-4.,8.,-83.8));
#37694=CARTESIAN_POINT('Origin',(0.,8.,-83.8));
#37695=CARTESIAN_POINT('',(-4.,8.,-86.8));
#37696=CARTESIAN_POINT('Origin',(0.,8.,-83.8));
#37697=CARTESIAN_POINT('',(4.99995,8.,-83.8));
#37698=CARTESIAN_POINT('Origin',(0.,8.,-83.8));
#37699=CARTESIAN_POINT('',(4.99995,8.,-84.8));
#37700=CARTESIAN_POINT('',(4.99995,8.,-83.8));
#37701=CARTESIAN_POINT('Origin',(0.,8.,-84.8));
#37702=CARTESIAN_POINT('Origin',(25.4958861827765,-14.55,-104.175753233145));
#37703=CARTESIAN_POINT('',(23.,-16.5,-64.9));
#37704=CARTESIAN_POINT('',(25.4958861827765,-14.55,-69.5070923773207));
#37705=CARTESIAN_POINT('Origin',(28.4999999999971,-12.2029290542153,-64.9000000000014));
#37706=CARTESIAN_POINT('',(23.,-16.5,-71.4));
#37707=CARTESIAN_POINT('',(23.,-16.5,-84.8));
#37708=CARTESIAN_POINT('',(25.4958861827765,-14.55,-71.4));
#37709=CARTESIAN_POINT('',(25.4958861827765,-14.55,-71.4));
#37710=CARTESIAN_POINT('',(25.4958861827765,-14.55,-104.175753233145));
#37711=CARTESIAN_POINT('Origin',(25.4958861827765,-14.55,-104.175753233145));
#37712=CARTESIAN_POINT('',(25.4958861827765,-14.55,-60.2929076226793));
#37713=CARTESIAN_POINT('Origin',(28.5000000000002,-12.2029290542129,-64.9000000000003));
#37714=CARTESIAN_POINT('',(25.4958861827765,-14.55,-24.5070923773207));
#37715=CARTESIAN_POINT('',(25.4958861827765,-14.55,-104.175753233145));
#37716=CARTESIAN_POINT('',(23.,-16.5,-19.9));
#37717=CARTESIAN_POINT('Origin',(28.4999999999964,-12.2029290542158,-19.900000000002));
#37718=CARTESIAN_POINT('',(23.,-16.5,-84.8));
#37719=CARTESIAN_POINT('Origin',(-25.4958861827765,-14.55,-104.175753233145));
#37720=CARTESIAN_POINT('',(-23.,-16.5,-64.9));
#37721=CARTESIAN_POINT('',(-25.4958861827765,-14.55,-60.2929076226793));
#37722=CARTESIAN_POINT('Origin',(-28.5000000000003,-12.2029290542127,-64.9000000000003));
#37723=CARTESIAN_POINT('',(-23.,-16.5,-19.9));
#37724=CARTESIAN_POINT('',(-23.,-16.5,-84.8));
#37725=CARTESIAN_POINT('',(-25.4958861827765,-14.55,-24.5070923773207));
#37726=CARTESIAN_POINT('Origin',(-28.4999999999988,-12.2029290542139,-19.9000000000006));
#37727=CARTESIAN_POINT('',(-25.4958861827765,-14.55,-104.175753233145));
#37728=CARTESIAN_POINT('Origin',(-25.4958861827765,-14.55,-104.175753233145));
#37729=CARTESIAN_POINT('',(-25.4958861827765,-14.55,-15.2929076226793));
#37730=CARTESIAN_POINT('Origin',(-28.4999999999998,-12.2029290542132,-19.8999999999999));
#37731=CARTESIAN_POINT('',(-23.,-16.5,-13.4));
#37732=CARTESIAN_POINT('',(-23.,-16.5,-84.8));
#37733=CARTESIAN_POINT('',(-25.4958861827765,-14.55,-13.4));
#37734=CARTESIAN_POINT('',(-25.4958861827765,-14.55,-13.4));
#37735=CARTESIAN_POINT('',(-25.4958861827765,-14.55,-104.175753233145));
#37736=CARTESIAN_POINT('Origin',(8.05,-8.2,-84.8));
#37737=CARTESIAN_POINT('',(8.57259699813413,-7.67740300186587,-81.35));
#37738=CARTESIAN_POINT('',(8.19644660940673,-8.05355339059327,-81.35));
#37739=CARTESIAN_POINT('',(8.57259699813413,-7.67740300186587,-81.35));
#37740=CARTESIAN_POINT('',(8.57259699813413,-7.67740300186587,-84.8));
#37741=CARTESIAN_POINT('',(8.57259699813413,-7.67740300186587,-84.8));
#37742=CARTESIAN_POINT('',(8.19644660940673,-8.05355339059327,-84.8));
#37743=CARTESIAN_POINT('',(8.05,-8.2,-84.8));
#37744=CARTESIAN_POINT('',(8.19644660940673,-8.05355339059327,-84.8));
#37745=CARTESIAN_POINT('Origin',(8.05,3.67394039744206E-16,-84.8));
#37746=CARTESIAN_POINT('',(10.9824030018659,-2.93240300186586,-81.35));
#37747=CARTESIAN_POINT('',(11.3535533905933,-3.30355339059329,-81.35));
#37748=CARTESIAN_POINT('',(10.9824030018659,-2.93240300186586,-81.35));
#37749=CARTESIAN_POINT('',(10.9824030018659,-2.93240300186586,-84.8));
#37750=CARTESIAN_POINT('',(10.9824030018659,-2.93240300186586,-84.8));
#37751=CARTESIAN_POINT('',(11.3535533905933,-3.30355339059329,-84.8));
#37752=CARTESIAN_POINT('',(8.05,3.67394039744206E-16,-84.8));
#37753=CARTESIAN_POINT('',(11.3535533905933,-3.30355339059329,0.));
#37754=CARTESIAN_POINT('Origin',(-8.05,-8.2,-84.8));
#37755=CARTESIAN_POINT('',(-10.9824030018659,-5.26759699813413,-81.35));
#37756=CARTESIAN_POINT('',(-11.3535533905933,-4.89644660940674,-81.35));
#37757=CARTESIAN_POINT('',(-10.9824030018659,-5.26759699813413,-81.35));
#37758=CARTESIAN_POINT('',(-10.9824030018659,-5.26759699813413,-84.8));
#37759=CARTESIAN_POINT('',(-10.9824030018659,-5.26759699813413,-84.8));
#37760=CARTESIAN_POINT('',(-11.3535533905933,-4.89644660940674,-84.8));
#37761=CARTESIAN_POINT('',(-8.05,-8.2,-84.8));
#37762=CARTESIAN_POINT('',(-11.3535533905933,-4.89644660940674,0.));
#37763=CARTESIAN_POINT('Origin',(-8.05,-1.60428730688303E-15,-84.8));
#37764=CARTESIAN_POINT('',(-8.57259699813413,-0.522596998134137,-81.35));
#37765=CARTESIAN_POINT('',(-8.05,-1.60428730688303E-15,-81.35));
#37766=CARTESIAN_POINT('',(-8.57259699813413,-0.522596998134137,-81.35));
#37767=CARTESIAN_POINT('',(-8.57259699813413,-0.522596998134137,-84.8));
#37768=CARTESIAN_POINT('',(-8.57259699813413,-0.522596998134137,-84.8));
#37769=CARTESIAN_POINT('',(-8.05,-1.60428730688303E-15,-84.8));
#37770=CARTESIAN_POINT('',(-8.05,-1.60428730688303E-15,-84.8));
#37771=CARTESIAN_POINT('',(-8.05,-1.60428730688303E-15,-84.8));
#37772=CARTESIAN_POINT('Origin',(-8.05,-1.60428730688303E-15,-84.8));
#37773=CARTESIAN_POINT('',(-11.3535533905933,-3.30355339059329,-81.35));
#37774=CARTESIAN_POINT('',(-10.9824030018659,-2.93240300186587,-81.35));
#37775=CARTESIAN_POINT('',(-11.3535533905933,-3.30355339059329,-81.35));
#37776=CARTESIAN_POINT('',(-11.3535533905933,-3.30355339059329,-84.8));
#37777=CARTESIAN_POINT('',(-11.3535533905933,-3.30355339059329,-84.8));
#37778=CARTESIAN_POINT('',(-10.9824030018659,-2.93240300186587,-84.8));
#37779=CARTESIAN_POINT('',(-8.05,-1.60428730688303E-15,-84.8));
#37780=CARTESIAN_POINT('',(-10.9824030018659,-2.93240300186587,0.));
#37781=CARTESIAN_POINT('Origin',(-11.5,-4.75000000000001,-84.8));
#37782=CARTESIAN_POINT('',(-11.5,-4.54289321881346,-81.35));
#37783=CARTESIAN_POINT('',(-11.5,-3.65710678118656,-81.35));
#37784=CARTESIAN_POINT('',(-11.5,-4.54289321881346,-81.35));
#37785=CARTESIAN_POINT('',(-11.5,-4.54289321881346,-84.8));
#37786=CARTESIAN_POINT('',(-11.5,-4.54289321881346,-84.8));
#37787=CARTESIAN_POINT('',(-11.5,-3.65710678118656,-84.8));
#37788=CARTESIAN_POINT('',(-11.5,-4.75000000000001,-84.8));
#37789=CARTESIAN_POINT('',(-11.5,-3.65710678118656,0.));
#37790=CARTESIAN_POINT('Origin',(-8.05,-8.2,-84.8));
#37791=CARTESIAN_POINT('',(-8.19644660940673,-8.05355339059327,-81.35));
#37792=CARTESIAN_POINT('',(-8.57259699813413,-7.67740300186587,-81.35));
#37793=CARTESIAN_POINT('',(-8.19644660940673,-8.05355339059327,-81.35));
#37794=CARTESIAN_POINT('',(-8.19644660940673,-8.05355339059327,-84.8));
#37795=CARTESIAN_POINT('',(-8.19644660940673,-8.05355339059327,-84.8));
#37796=CARTESIAN_POINT('',(-8.57259699813413,-7.67740300186587,-84.8));
#37797=CARTESIAN_POINT('',(-8.05,-8.2,-84.8));
#37798=CARTESIAN_POINT('',(-8.57259699813413,-7.67740300186587,0.));
#37799=CARTESIAN_POINT('Origin',(-8.05,-12.24,-84.8));
#37800=CARTESIAN_POINT('',(-8.05,-12.0328932188134,-81.35));
#37801=CARTESIAN_POINT('',(-8.05,-8.40710678118654,-81.35));
#37802=CARTESIAN_POINT('',(-8.05,-12.0328932188134,-81.35));
#37803=CARTESIAN_POINT('',(-8.05,-12.0328932188134,-84.8));
#37804=CARTESIAN_POINT('',(-8.05,-12.0328932188134,-84.8));
#37805=CARTESIAN_POINT('',(-8.05,-8.40710678118654,-84.8));
#37806=CARTESIAN_POINT('',(-8.05,-12.24,-84.8));
#37807=CARTESIAN_POINT('',(-8.05,-8.40710678118654,-84.8));
#37808=CARTESIAN_POINT('Origin',(-12.31,-16.5,-84.8));
#37809=CARTESIAN_POINT('',(-12.31,-16.5,-81.35));
#37810=CARTESIAN_POINT('',(-8.19644660940672,-12.3864466094067,-81.35));
#37811=CARTESIAN_POINT('',(-12.31,-16.5,-81.35));
#37812=CARTESIAN_POINT('',(-12.31,-16.5,-84.8));
#37813=CARTESIAN_POINT('',(-12.31,-16.5,-84.8));
#37814=CARTESIAN_POINT('',(-8.19644660940672,-12.3864466094067,-84.8));
#37815=CARTESIAN_POINT('',(-12.31,-16.5,-84.8));
#37816=CARTESIAN_POINT('',(-8.19644660940672,-12.3864466094067,-84.8));
#37817=CARTESIAN_POINT('Origin',(-23.,-16.5,-84.8));
#37818=CARTESIAN_POINT('',(-22.2,-16.5,-81.35));
#37819=CARTESIAN_POINT('',(-22.2,-16.5,-81.35));
#37820=CARTESIAN_POINT('',(-22.2,-16.5,-84.8));
#37821=CARTESIAN_POINT('',(-22.2,-16.5,-84.8));
#37822=CARTESIAN_POINT('',(-23.,-16.5,-84.8));
#37823=CARTESIAN_POINT('Origin',(12.31,-16.5,-84.8));
#37824=CARTESIAN_POINT('',(12.31,-16.5,-81.35));
#37825=CARTESIAN_POINT('',(22.2,-16.5,-81.35));
#37826=CARTESIAN_POINT('',(12.31,-16.5,-81.35));
#37827=CARTESIAN_POINT('',(12.31,-16.5,-84.8));
#37828=CARTESIAN_POINT('',(12.31,-16.5,-84.8));
#37829=CARTESIAN_POINT('',(22.2,-16.5,-84.8));
#37830=CARTESIAN_POINT('',(12.31,-16.5,-84.8));
#37831=CARTESIAN_POINT('',(22.2,-16.5,-84.8));
#37832=CARTESIAN_POINT('Origin',(12.31,-16.5,-84.8));
#37833=CARTESIAN_POINT('',(8.19644660940673,-12.3864466094067,-81.35));
#37834=CARTESIAN_POINT('',(8.19644660940673,-12.3864466094067,-81.35));
#37835=CARTESIAN_POINT('',(8.19644660940673,-12.3864466094067,-84.8));
#37836=CARTESIAN_POINT('',(8.19644660940673,-12.3864466094067,-84.8));
#37837=CARTESIAN_POINT('',(12.31,-16.5,-84.8));
#37838=CARTESIAN_POINT('Origin',(8.05,-12.24,-84.8));
#37839=CARTESIAN_POINT('',(8.05,-8.40710678118654,-81.35));
#37840=CARTESIAN_POINT('',(8.05,-12.0328932188134,-81.35));
#37841=CARTESIAN_POINT('',(8.05,-8.40710678118654,-81.35));
#37842=CARTESIAN_POINT('',(8.05,-8.40710678118654,-84.8));
#37843=CARTESIAN_POINT('',(8.05,-8.40710678118654,-84.8));
#37844=CARTESIAN_POINT('',(8.05,-12.0328932188134,-84.8));
#37845=CARTESIAN_POINT('',(8.05,-12.24,-84.8));
#37846=CARTESIAN_POINT('',(8.05,-12.0328932188134,-84.8));
#37847=CARTESIAN_POINT('Origin',(8.05,-8.2,-84.8));
#37848=CARTESIAN_POINT('',(11.3535533905933,-4.89644660940673,-81.35));
#37849=CARTESIAN_POINT('',(10.9824030018659,-5.26759699813413,-81.35));
#37850=CARTESIAN_POINT('',(11.3535533905933,-4.89644660940673,-81.35));
#37851=CARTESIAN_POINT('',(11.3535533905933,-4.89644660940673,-84.8));
#37852=CARTESIAN_POINT('',(11.3535533905933,-4.89644660940673,-84.8));
#37853=CARTESIAN_POINT('',(10.9824030018659,-5.26759699813413,-84.8));
#37854=CARTESIAN_POINT('',(8.05,-8.2,-84.8));
#37855=CARTESIAN_POINT('',(10.9824030018659,-5.26759699813413,0.));
#37856=CARTESIAN_POINT('Origin',(11.5,-4.75000000000001,-84.8));
#37857=CARTESIAN_POINT('',(11.5,-3.65710678118656,-81.35));
#37858=CARTESIAN_POINT('',(11.5,-4.54289321881346,-81.35));
#37859=CARTESIAN_POINT('',(11.5,-3.65710678118656,-81.35));
#37860=CARTESIAN_POINT('',(11.5,-3.65710678118656,-84.8));
#37861=CARTESIAN_POINT('',(11.5,-3.65710678118656,-84.8));
#37862=CARTESIAN_POINT('',(11.5,-4.54289321881346,-84.8));
#37863=CARTESIAN_POINT('',(11.5,-4.75000000000001,-84.8));
#37864=CARTESIAN_POINT('',(11.5,-4.54289321881346,0.));
#37865=CARTESIAN_POINT('Origin',(8.05,3.67394039744206E-16,-84.8));
#37866=CARTESIAN_POINT('',(8.05,3.67394039744206E-16,-81.35));
#37867=CARTESIAN_POINT('',(8.57259699813413,-0.522596998134133,-81.35));
#37868=CARTESIAN_POINT('',(8.05,3.67394039744206E-16,-81.35));
#37869=CARTESIAN_POINT('',(8.05,3.67394039744206E-16,-84.8));
#37870=CARTESIAN_POINT('',(8.05,3.67394039744206E-16,-84.8));
#37871=CARTESIAN_POINT('',(8.57259699813413,-0.522596998134133,-84.8));
#37872=CARTESIAN_POINT('',(8.05,3.67394039744206E-16,-84.8));
#37873=CARTESIAN_POINT('',(8.57259699813413,-0.522596998134133,0.));
#37874=CARTESIAN_POINT('Origin',(8.05,3.67394039744206E-16,-84.8));
#37875=CARTESIAN_POINT('',(-8.05,-1.60428730688303E-15,-81.35));
#37876=CARTESIAN_POINT('',(8.05,3.67394039744206E-16,-84.8));
#37877=CARTESIAN_POINT('Origin',(-10.995,-0.510000000000002,-84.8));
#37878=CARTESIAN_POINT('',(-10.6942336092596,-2.79024989380572,-81.35));
#37879=CARTESIAN_POINT('',(-8.71475010619428,-0.810766390740372,-81.35));
#37880=CARTESIAN_POINT('Origin',(-10.995,-0.510000000000002,-81.35));
#37881=CARTESIAN_POINT('',(-10.6942336092596,-2.79024989380572,-84.8));
#37882=CARTESIAN_POINT('',(-10.6942336092596,-2.79024989380572,-84.8));
#37883=CARTESIAN_POINT('',(-8.71475010619428,-0.810766390740372,-84.8));
#37884=CARTESIAN_POINT('Origin',(-10.995,-0.510000000000002,-84.8));
#37885=CARTESIAN_POINT('',(-8.71475010619428,-0.810766390740372,-84.8));
#37886=CARTESIAN_POINT('Origin',(-10.995,-7.69,-84.8));
#37887=CARTESIAN_POINT('',(-8.71475010619428,-7.38923360925963,-81.35));
#37888=CARTESIAN_POINT('',(-10.6942336092596,-5.40975010619428,-81.35));
#37889=CARTESIAN_POINT('Origin',(-10.995,-7.69,-81.35));
#37890=CARTESIAN_POINT('',(-8.71475010619428,-7.38923360925963,-84.8));
#37891=CARTESIAN_POINT('',(-8.71475010619428,-7.38923360925963,-84.8));
#37892=CARTESIAN_POINT('',(-10.6942336092596,-5.40975010619428,-84.8));
#37893=CARTESIAN_POINT('Origin',(-10.995,-7.69,-84.8));
#37894=CARTESIAN_POINT('',(-10.6942336092596,-5.40975010619428,-84.8));
#37895=CARTESIAN_POINT('Origin',(10.995,-0.509999999999999,-84.8));
#37896=CARTESIAN_POINT('',(8.71475010619428,-0.81076639074037,-81.35));
#37897=CARTESIAN_POINT('',(10.6942336092596,-2.79024989380572,-81.35));
#37898=CARTESIAN_POINT('Origin',(10.995,-0.509999999999999,-81.35));
#37899=CARTESIAN_POINT('',(8.71475010619428,-0.81076639074037,-84.8));
#37900=CARTESIAN_POINT('',(8.71475010619428,-0.81076639074037,-84.8));
#37901=CARTESIAN_POINT('',(10.6942336092596,-2.79024989380572,-84.8));
#37902=CARTESIAN_POINT('Origin',(10.995,-0.509999999999999,-84.8));
#37903=CARTESIAN_POINT('',(10.6942336092596,-2.79024989380572,-84.8));
#37904=CARTESIAN_POINT('Origin',(10.995,-7.69,-84.8));
#37905=CARTESIAN_POINT('',(10.6942336092596,-5.40975010619428,-81.35));
#37906=CARTESIAN_POINT('',(8.71475010619428,-7.38923360925963,-81.35));
#37907=CARTESIAN_POINT('Origin',(10.995,-7.69,-81.35));
#37908=CARTESIAN_POINT('',(10.6942336092596,-5.40975010619428,-84.8));
#37909=CARTESIAN_POINT('',(10.6942336092596,-5.40975010619428,-84.8));
#37910=CARTESIAN_POINT('',(8.71475010619428,-7.38923360925963,-84.8));
#37911=CARTESIAN_POINT('Origin',(10.995,-7.69,-84.8));
#37912=CARTESIAN_POINT('',(8.71475010619428,-7.38923360925963,-84.8));
#37913=CARTESIAN_POINT('Origin',(8.55,-12.0328932188134,-84.8));
#37914=CARTESIAN_POINT('Origin',(8.55,-12.0328932188134,-81.35));
#37915=CARTESIAN_POINT('Origin',(8.55,-12.0328932188134,-84.8));
#37916=CARTESIAN_POINT('Origin',(-8.55,-12.0328932188134,-84.8));
#37917=CARTESIAN_POINT('Origin',(-8.55,-12.0328932188134,-81.35));
#37918=CARTESIAN_POINT('Origin',(-8.55,-12.0328932188134,-84.8));
#37919=CARTESIAN_POINT('Origin',(11.,-4.54289321881346,-84.8));
#37920=CARTESIAN_POINT('Origin',(11.,-4.54289321881346,-81.35));
#37921=CARTESIAN_POINT('Origin',(11.,-4.54289321881346,-84.8));
#37922=CARTESIAN_POINT('Origin',(11.,-3.65710678118656,-84.8));
#37923=CARTESIAN_POINT('Origin',(11.,-3.65710678118656,-81.35));
#37924=CARTESIAN_POINT('Origin',(11.,-3.65710678118656,-84.8));
#37925=CARTESIAN_POINT('Origin',(10.6288496112726,-3.28595639245914,-84.8));
#37926=CARTESIAN_POINT('Origin',(10.6288496112726,-3.28595639245914,-81.35));
#37927=CARTESIAN_POINT('Origin',(10.6288496112726,-3.28595639245914,-84.8));
#37928=CARTESIAN_POINT('Origin',(8.21904360754086,-0.876150388727407,-84.8));
#37929=CARTESIAN_POINT('Origin',(8.21904360754086,-0.876150388727407,-81.35));
#37930=CARTESIAN_POINT('Origin',(8.21904360754086,-0.876150388727407,-84.8));
#37931=CARTESIAN_POINT('Origin',(10.6288496112726,-4.91404360754086,-84.8));
#37932=CARTESIAN_POINT('Origin',(10.6288496112726,-4.91404360754086,-81.35));
#37933=CARTESIAN_POINT('Origin',(10.6288496112726,-4.91404360754086,-84.8));
#37934=CARTESIAN_POINT('Origin',(8.21904360754086,-7.32384961127259,-84.8));
#37935=CARTESIAN_POINT('Origin',(8.21904360754086,-7.32384961127259,-81.35));
#37936=CARTESIAN_POINT('Origin',(8.21904360754086,-7.32384961127259,-84.8));
#37937=CARTESIAN_POINT('Origin',(8.55,-8.40710678118654,-84.8));
#37938=CARTESIAN_POINT('Origin',(8.55,-8.40710678118654,-81.35));
#37939=CARTESIAN_POINT('Origin',(8.55,-8.40710678118654,-84.8));
#37940=CARTESIAN_POINT('Origin',(-8.55,-8.40710678118654,-84.8));
#37941=CARTESIAN_POINT('Origin',(-8.55,-8.40710678118654,-81.35));
#37942=CARTESIAN_POINT('Origin',(-8.55,-8.40710678118654,-84.8));
#37943=CARTESIAN_POINT('Origin',(-8.21904360754086,-7.32384961127259,-84.8));
#37944=CARTESIAN_POINT('Origin',(-8.21904360754086,-7.32384961127259,-81.35));
#37945=CARTESIAN_POINT('Origin',(-8.21904360754086,-7.32384961127259,-84.8));
#37946=CARTESIAN_POINT('Origin',(-10.6288496112726,-4.91404360754086,-84.8));
#37947=CARTESIAN_POINT('Origin',(-10.6288496112726,-4.91404360754086,-81.35));
#37948=CARTESIAN_POINT('Origin',(-10.6288496112726,-4.91404360754086,-84.8));
#37949=CARTESIAN_POINT('Origin',(-11.,-4.54289321881346,-84.8));
#37950=CARTESIAN_POINT('Origin',(-11.,-4.54289321881346,-81.35));
#37951=CARTESIAN_POINT('Origin',(-11.,-4.54289321881346,-84.8));
#37952=CARTESIAN_POINT('Origin',(-11.,-3.65710678118656,-84.8));
#37953=CARTESIAN_POINT('Origin',(-11.,-3.65710678118656,-81.35));
#37954=CARTESIAN_POINT('Origin',(-11.,-3.65710678118656,-84.8));
#37955=CARTESIAN_POINT('Origin',(-10.6288496112726,-3.28595639245914,-84.8));
#37956=CARTESIAN_POINT('Origin',(-10.6288496112726,-3.28595639245914,-81.35));
#37957=CARTESIAN_POINT('Origin',(-10.6288496112726,-3.28595639245914,-84.8));
#37958=CARTESIAN_POINT('Origin',(-8.21904360754086,-0.87615038872741,-84.8));
#37959=CARTESIAN_POINT('Origin',(-8.21904360754086,-0.87615038872741,-81.35));
#37960=CARTESIAN_POINT('Origin',(-8.21904360754086,-0.87615038872741,-84.8));
#37961=CARTESIAN_POINT('Origin',(0.,8.,-83.8));
#37962=CARTESIAN_POINT('Origin',(-22.2,13.,-84.8));
#37963=CARTESIAN_POINT('',(-22.2,13.,-84.8));
#37964=CARTESIAN_POINT('',(-22.2,13.,-81.35));
#37965=CARTESIAN_POINT('',(-22.2,13.,-84.8));
#37966=CARTESIAN_POINT('',(22.2,13.,-81.35));
#37967=CARTESIAN_POINT('',(22.2,13.,-81.35));
#37968=CARTESIAN_POINT('',(22.2,13.,-84.8));
#37969=CARTESIAN_POINT('',(22.2,13.,-84.8));
#37970=CARTESIAN_POINT('',(-22.2,13.,-84.8));
#37971=CARTESIAN_POINT('Origin',(0.,0.,-84.8));
#37972=CARTESIAN_POINT('',(-23.2,-15.5,-84.8));
#37973=CARTESIAN_POINT('',(-22.2,-16.5,-84.8));
#37974=CARTESIAN_POINT('',(-23.2,12.,-84.8));
#37975=CARTESIAN_POINT('',(-23.2,-15.5,-84.8));
#37976=CARTESIAN_POINT('',(-23.2,12.,-84.8));
#37977=CARTESIAN_POINT('',(23.2,12.,-84.8));
#37978=CARTESIAN_POINT('',(22.2,13.,-84.8));
#37979=CARTESIAN_POINT('',(23.2,-15.5,-84.8));
#37980=CARTESIAN_POINT('',(23.2,12.,-84.8));
#37981=CARTESIAN_POINT('',(23.2,-15.5,-84.8));
#37982=CARTESIAN_POINT('Origin',(-23.2,12.,-84.8));
#37983=CARTESIAN_POINT('',(-23.2,12.,-81.35));
#37984=CARTESIAN_POINT('',(-23.2,12.,-84.8));
#37985=CARTESIAN_POINT('',(-22.2,13.,-81.35));
#37986=CARTESIAN_POINT('Origin',(-23.2,-15.5,-84.8));
#37987=CARTESIAN_POINT('',(-23.2,-15.5,-81.35));
#37988=CARTESIAN_POINT('',(-23.2,-15.5,-84.8));
#37989=CARTESIAN_POINT('',(-23.2,12.,-81.35));
#37990=CARTESIAN_POINT('Origin',(-22.2,-16.5,-84.8));
#37991=CARTESIAN_POINT('',(-23.2,-15.5,-81.35));
#37992=CARTESIAN_POINT('Origin',(23.2,-15.5,-84.8));
#37993=CARTESIAN_POINT('',(23.2,-15.5,-81.35));
#37994=CARTESIAN_POINT('',(23.2,-15.5,-84.8));
#37995=CARTESIAN_POINT('',(22.2,-16.5,-81.35));
#37996=CARTESIAN_POINT('Origin',(23.2,12.,-84.8));
#37997=CARTESIAN_POINT('',(23.2,12.,-81.35));
#37998=CARTESIAN_POINT('',(23.2,12.,-84.8));
#37999=CARTESIAN_POINT('',(23.2,-15.5,-81.35));
#38000=CARTESIAN_POINT('Origin',(22.2,13.,-84.8));
#38001=CARTESIAN_POINT('',(23.2,12.,-81.35));
#38002=CARTESIAN_POINT('Origin',(-2.3094010767585,8.,-84.4));
#38003=CARTESIAN_POINT('',(-2.3094010767585,8.,-84.4));
#38004=CARTESIAN_POINT('',(-2.3094010767585,8.,-84.4));
#38005=CARTESIAN_POINT('',(-1.15470053837925,10.,-84.4));
#38006=CARTESIAN_POINT('',(-1.15470053837925,10.,-84.4));
#38007=CARTESIAN_POINT('',(-2.3094010767585,8.,-84.4));
#38008=CARTESIAN_POINT('Origin',(-1.15470053837925,6.,-84.4));
#38009=CARTESIAN_POINT('',(-1.15470053837925,6.,-84.4));
#38010=CARTESIAN_POINT('',(-1.15470053837925,6.,-84.4));
#38011=CARTESIAN_POINT('',(-1.15470053837925,6.,-84.4));
#38012=CARTESIAN_POINT('Origin',(1.15470053837925,6.,-84.4));
#38013=CARTESIAN_POINT('',(1.15470053837925,6.,-84.4));
#38014=CARTESIAN_POINT('',(1.15470053837925,6.,-84.4));
#38015=CARTESIAN_POINT('',(1.15470053837925,6.,-84.4));
#38016=CARTESIAN_POINT('Origin',(2.3094010767585,8.,-84.4));
#38017=CARTESIAN_POINT('',(2.3094010767585,8.,-84.4));
#38018=CARTESIAN_POINT('',(2.3094010767585,8.,-84.4));
#38019=CARTESIAN_POINT('',(2.3094010767585,8.,-84.4));
#38020=CARTESIAN_POINT('Origin',(1.15470053837925,10.,-84.4));
#38021=CARTESIAN_POINT('',(1.15470053837925,10.,-84.4));
#38022=CARTESIAN_POINT('',(1.15470053837925,10.,-84.4));
#38023=CARTESIAN_POINT('',(1.15470053837925,10.,-84.4));
#38024=CARTESIAN_POINT('Origin',(-1.15470053837925,10.,-84.4));
#38025=CARTESIAN_POINT('',(-1.15470053837925,10.,-84.4));
#38026=CARTESIAN_POINT('Origin',(0.,0.,-84.4));
#38027=CARTESIAN_POINT('Origin',(-8.55,-12.0328932188134,-81.35));
#38028=CARTESIAN_POINT('',(8.23180194846605,-12.3510912703474,-81.35));
#38029=CARTESIAN_POINT('',(12.3307106781187,-16.45,-81.35));
#38030=CARTESIAN_POINT('',(8.23180194846605,-12.3510912703474,-81.35));
#38031=CARTESIAN_POINT('',(8.1,-12.0328932188134,-81.35));
#38032=CARTESIAN_POINT('Origin',(8.55,-12.0328932188134,-81.35));
#38033=CARTESIAN_POINT('',(8.1,-8.40710678118654,-81.35));
#38034=CARTESIAN_POINT('',(8.1,-8.40710678118654,-81.35));
#38035=CARTESIAN_POINT('',(8.23180194846606,-8.08890872965259,-81.35));
#38036=CARTESIAN_POINT('Origin',(8.55,-8.40710678118654,-81.35));
#38037=CARTESIAN_POINT('',(8.60795233719346,-7.71275834092519,-81.35));
#38038=CARTESIAN_POINT('',(8.60795233719346,-7.71275834092519,-81.35));
#38039=CARTESIAN_POINT('',(8.76432075605962,-7.39577200905833,-81.35));
#38040=CARTESIAN_POINT('Origin',(8.21904360754086,-7.32384961127259,-81.35));
#38041=CARTESIAN_POINT('',(10.7007720090583,-5.45932075605962,-81.35));
#38042=CARTESIAN_POINT('Origin',(10.995,-7.69,-81.35));
#38043=CARTESIAN_POINT('',(11.0177583409252,-5.30295233719346,-81.35));
#38044=CARTESIAN_POINT('Origin',(10.6288496112726,-4.91404360754086,-81.35));
#38045=CARTESIAN_POINT('',(11.3889087296526,-4.93180194846606,-81.35));
#38046=CARTESIAN_POINT('',(11.3889087296526,-4.93180194846606,-81.35));
#38047=CARTESIAN_POINT('',(11.55,-4.54289321881346,-81.35));
#38048=CARTESIAN_POINT('Origin',(11.,-4.54289321881346,-81.35));
#38049=CARTESIAN_POINT('',(11.55,-3.65710678118656,-81.35));
#38050=CARTESIAN_POINT('',(11.55,-3.65710678118656,-81.35));
#38051=CARTESIAN_POINT('',(11.3889087296526,-3.26819805153396,-81.35));
#38052=CARTESIAN_POINT('Origin',(11.,-3.65710678118656,-81.35));
#38053=CARTESIAN_POINT('',(11.0177583409252,-2.89704766280654,-81.35));
#38054=CARTESIAN_POINT('',(11.0177583409252,-2.89704766280654,-81.35));
#38055=CARTESIAN_POINT('',(10.7007720090583,-2.74067924394038,-81.35));
#38056=CARTESIAN_POINT('Origin',(10.6288496112726,-3.28595639245914,-81.35));
#38057=CARTESIAN_POINT('',(8.76432075605962,-0.804227990941667,-81.35));
#38058=CARTESIAN_POINT('Origin',(10.995,-0.509999999999999,-81.35));
#38059=CARTESIAN_POINT('',(8.60795233719346,-0.487241659074806,-81.35));
#38060=CARTESIAN_POINT('Origin',(8.21904360754086,-0.876150388727407,-81.35));
#38061=CARTESIAN_POINT('',(8.07071067811865,0.0500000000000006,-81.35));
#38062=CARTESIAN_POINT('',(8.07071067811865,0.0500000000000006,-81.35));
#38063=CARTESIAN_POINT('',(-8.07071067811865,0.0499999999999998,-81.35));
#38064=CARTESIAN_POINT('',(-8.07071067811865,0.0499999999999998,-81.35));
#38065=CARTESIAN_POINT('',(-8.60795233719346,-0.48724165907481,-81.35));
#38066=CARTESIAN_POINT('',(-8.60795233719346,-0.487241659074809,-81.35));
#38067=CARTESIAN_POINT('',(-8.76432075605962,-0.804227990941668,-81.35));
#38068=CARTESIAN_POINT('Origin',(-8.21904360754086,-0.87615038872741,-81.35));
#38069=CARTESIAN_POINT('',(-10.7007720090583,-2.74067924394038,-81.35));
#38070=CARTESIAN_POINT('Origin',(-10.995,-0.510000000000002,-81.35));
#38071=CARTESIAN_POINT('',(-11.0177583409252,-2.89704766280654,-81.35));
#38072=CARTESIAN_POINT('Origin',(-10.6288496112726,-3.28595639245914,-81.35));
#38073=CARTESIAN_POINT('',(-11.3889087296526,-3.26819805153396,-81.35));
#38074=CARTESIAN_POINT('',(-11.3889087296526,-3.26819805153396,-81.35));
#38075=CARTESIAN_POINT('',(-11.55,-3.65710678118656,-81.35));
#38076=CARTESIAN_POINT('Origin',(-11.,-3.65710678118656,-81.35));
#38077=CARTESIAN_POINT('',(-11.55,-4.54289321881346,-81.35));
#38078=CARTESIAN_POINT('',(-11.55,-4.54289321881346,-81.35));
#38079=CARTESIAN_POINT('',(-11.3889087296526,-4.93180194846607,-81.35));
#38080=CARTESIAN_POINT('Origin',(-11.,-4.54289321881346,-81.35));
#38081=CARTESIAN_POINT('',(-11.0177583409252,-5.30295233719346,-81.35));
#38082=CARTESIAN_POINT('',(-11.0177583409252,-5.30295233719346,-81.35));
#38083=CARTESIAN_POINT('',(-10.7007720090583,-5.45932075605962,-81.35));
#38084=CARTESIAN_POINT('Origin',(-10.6288496112726,-4.91404360754086,-81.35));
#38085=CARTESIAN_POINT('',(-8.76432075605962,-7.39577200905833,-81.35));
#38086=CARTESIAN_POINT('Origin',(-10.995,-7.69,-81.35));
#38087=CARTESIAN_POINT('',(-8.60795233719346,-7.7127583409252,-81.35));
#38088=CARTESIAN_POINT('Origin',(-8.21904360754086,-7.32384961127259,-81.35));
#38089=CARTESIAN_POINT('',(-8.23180194846605,-8.0889087296526,-81.35));
#38090=CARTESIAN_POINT('',(-8.23180194846605,-8.0889087296526,-81.35));
#38091=CARTESIAN_POINT('',(-8.1,-8.40710678118654,-81.35));
#38092=CARTESIAN_POINT('Origin',(-8.55,-8.40710678118654,-81.35));
#38093=CARTESIAN_POINT('',(-8.1,-12.0328932188134,-81.35));
#38094=CARTESIAN_POINT('',(-8.1,-12.0328932188134,-81.35));
#38095=CARTESIAN_POINT('',(-8.23180194846605,-12.3510912703474,-81.35));
#38096=CARTESIAN_POINT('Origin',(-8.55,-12.0328932188134,-81.35));
#38097=CARTESIAN_POINT('',(-12.3307106781186,-16.45,-81.35));
#38098=CARTESIAN_POINT('',(-12.3307106781186,-16.45,-81.35));
#38099=CARTESIAN_POINT('',(-22.1792893218814,-16.45,-81.35));
#38100=CARTESIAN_POINT('',(-22.1792893218814,-16.45,-81.35));
#38101=CARTESIAN_POINT('',(-23.15,-15.4792893218813,-81.35));
#38102=CARTESIAN_POINT('',(-23.15,-15.4792893218813,-81.35));
#38103=CARTESIAN_POINT('',(-23.15,11.9792893218814,-81.35));
#38104=CARTESIAN_POINT('',(-23.15,11.9792893218814,-81.35));
#38105=CARTESIAN_POINT('',(-22.1792893218813,12.95,-81.35));
#38106=CARTESIAN_POINT('',(-22.1792893218813,12.95,-81.35));
#38107=CARTESIAN_POINT('',(22.1792893218813,12.95,-81.35));
#38108=CARTESIAN_POINT('',(22.1792893218813,12.95,-81.35));
#38109=CARTESIAN_POINT('',(23.15,11.9792893218814,-81.35));
#38110=CARTESIAN_POINT('',(23.15,11.9792893218814,-81.35));
#38111=CARTESIAN_POINT('',(23.15,-15.4792893218813,-81.35));
#38112=CARTESIAN_POINT('',(23.15,-15.4792893218813,-81.35));
#38113=CARTESIAN_POINT('',(22.1792893218814,-16.45,-81.35));
#38114=CARTESIAN_POINT('',(22.1792893218814,-16.45,-81.35));
#38115=CARTESIAN_POINT('',(12.3307106781187,-16.45,-81.35));
#38116=CARTESIAN_POINT('Origin',(8.23180194846605,-12.3510912703474,-81.35));
#38117=CARTESIAN_POINT('',(8.23180194846605,-12.3510912703474,-81.3));
#38118=CARTESIAN_POINT('',(12.3307106781187,-16.45,-81.3));
#38119=CARTESIAN_POINT('',(8.23180194846605,-12.3510912703474,-81.3));
#38120=CARTESIAN_POINT('',(8.23180194846605,-12.3510912703474,-81.35));
#38121=CARTESIAN_POINT('',(12.3307106781187,-16.45,-81.35));
#38122=CARTESIAN_POINT('Origin',(8.55,-12.0328932188134,-81.35));
#38123=CARTESIAN_POINT('',(8.1,-12.0328932188134,-81.3));
#38124=CARTESIAN_POINT('Origin',(8.55,-12.0328932188134,-81.3));
#38125=CARTESIAN_POINT('',(8.1,-12.0328932188134,-81.35));
#38126=CARTESIAN_POINT('Origin',(8.1,-8.40710678118654,-81.35));
#38127=CARTESIAN_POINT('',(8.1,-8.40710678118654,-81.3));
#38128=CARTESIAN_POINT('',(8.1,-8.40710678118654,-81.3));
#38129=CARTESIAN_POINT('',(8.1,-8.40710678118654,-81.35));
#38130=CARTESIAN_POINT('Origin',(8.55,-8.40710678118654,-81.35));
#38131=CARTESIAN_POINT('',(8.23180194846606,-8.08890872965259,-81.3));
#38132=CARTESIAN_POINT('Origin',(8.55,-8.40710678118654,-81.3));
#38133=CARTESIAN_POINT('',(8.23180194846606,-8.08890872965259,-81.35));
#38134=CARTESIAN_POINT('Origin',(8.60795233719346,-7.71275834092519,-81.35));
#38135=CARTESIAN_POINT('',(8.60795233719346,-7.71275834092519,-81.3));
#38136=CARTESIAN_POINT('',(8.60795233719346,-7.71275834092519,-81.3));
#38137=CARTESIAN_POINT('',(8.60795233719346,-7.71275834092519,-81.35));
#38138=CARTESIAN_POINT('Origin',(8.21904360754086,-7.32384961127259,-81.35));
#38139=CARTESIAN_POINT('',(8.76432075605962,-7.39577200905833,-81.3));
#38140=CARTESIAN_POINT('Origin',(8.21904360754086,-7.32384961127259,-81.3));
#38141=CARTESIAN_POINT('',(8.76432075605962,-7.39577200905833,-81.35));
#38142=CARTESIAN_POINT('Origin',(10.995,-7.69,-81.35));
#38143=CARTESIAN_POINT('',(10.7007720090583,-5.45932075605962,-81.3));
#38144=CARTESIAN_POINT('Origin',(10.995,-7.69,-81.3));
#38145=CARTESIAN_POINT('',(10.7007720090583,-5.45932075605962,-81.35));
#38146=CARTESIAN_POINT('Origin',(10.6288496112726,-4.91404360754086,-81.35));
#38147=CARTESIAN_POINT('',(11.0177583409252,-5.30295233719346,-81.3));
#38148=CARTESIAN_POINT('Origin',(10.6288496112726,-4.91404360754086,-81.3));
#38149=CARTESIAN_POINT('',(11.0177583409252,-5.30295233719346,-81.35));
#38150=CARTESIAN_POINT('Origin',(11.3889087296526,-4.93180194846606,-81.35));
#38151=CARTESIAN_POINT('',(11.3889087296526,-4.93180194846606,-81.3));
#38152=CARTESIAN_POINT('',(11.3889087296526,-4.93180194846606,-81.3));
#38153=CARTESIAN_POINT('',(11.3889087296526,-4.93180194846606,-81.35));
#38154=CARTESIAN_POINT('Origin',(11.,-4.54289321881346,-81.35));
#38155=CARTESIAN_POINT('',(11.55,-4.54289321881346,-81.3));
#38156=CARTESIAN_POINT('Origin',(11.,-4.54289321881346,-81.3));
#38157=CARTESIAN_POINT('',(11.55,-4.54289321881346,-81.35));
#38158=CARTESIAN_POINT('Origin',(11.55,-3.65710678118656,-81.35));
#38159=CARTESIAN_POINT('',(11.55,-3.65710678118656,-81.3));
#38160=CARTESIAN_POINT('',(11.55,-3.65710678118656,-81.3));
#38161=CARTESIAN_POINT('',(11.55,-3.65710678118656,-81.35));
#38162=CARTESIAN_POINT('Origin',(11.,-3.65710678118656,-81.35));
#38163=CARTESIAN_POINT('',(11.3889087296526,-3.26819805153396,-81.3));
#38164=CARTESIAN_POINT('Origin',(11.,-3.65710678118656,-81.3));
#38165=CARTESIAN_POINT('',(11.3889087296526,-3.26819805153396,-81.35));
#38166=CARTESIAN_POINT('Origin',(11.0177583409252,-2.89704766280654,-81.35));
#38167=CARTESIAN_POINT('',(11.0177583409252,-2.89704766280654,-81.3));
#38168=CARTESIAN_POINT('',(11.0177583409252,-2.89704766280654,-81.3));
#38169=CARTESIAN_POINT('',(11.0177583409252,-2.89704766280654,-81.35));
#38170=CARTESIAN_POINT('Origin',(10.6288496112726,-3.28595639245914,-81.35));
#38171=CARTESIAN_POINT('',(10.7007720090583,-2.74067924394038,-81.3));
#38172=CARTESIAN_POINT('Origin',(10.6288496112726,-3.28595639245914,-81.3));
#38173=CARTESIAN_POINT('',(10.7007720090583,-2.74067924394038,-81.35));
#38174=CARTESIAN_POINT('Origin',(10.995,-0.509999999999999,-81.35));
#38175=CARTESIAN_POINT('',(8.76432075605962,-0.804227990941667,-81.3));
#38176=CARTESIAN_POINT('Origin',(10.995,-0.509999999999999,-81.3));
#38177=CARTESIAN_POINT('',(8.76432075605962,-0.804227990941667,-81.35));
#38178=CARTESIAN_POINT('Origin',(8.21904360754086,-0.876150388727407,-81.35));
#38179=CARTESIAN_POINT('',(8.60795233719346,-0.487241659074806,-81.3));
#38180=CARTESIAN_POINT('Origin',(8.21904360754086,-0.876150388727407,-81.3));
#38181=CARTESIAN_POINT('',(8.60795233719346,-0.487241659074806,-81.35));
#38182=CARTESIAN_POINT('Origin',(8.07071067811865,0.0500000000000006,-81.35));
#38183=CARTESIAN_POINT('',(8.07071067811865,0.0500000000000006,-81.3));
#38184=CARTESIAN_POINT('',(8.07071067811865,0.0500000000000006,-81.3));
#38185=CARTESIAN_POINT('',(8.07071067811865,0.0500000000000006,-81.35));
#38186=CARTESIAN_POINT('Origin',(-8.07071067811865,0.0499999999999998,-81.35));
#38187=CARTESIAN_POINT('',(-8.07071067811865,0.0499999999999998,-81.3));
#38188=CARTESIAN_POINT('',(-8.07071067811865,0.0499999999999998,-81.3));
#38189=CARTESIAN_POINT('',(-8.07071067811865,0.0499999999999998,-81.35));
#38190=CARTESIAN_POINT('Origin',(-8.60795233719346,-0.487241659074809,-81.35));
#38191=CARTESIAN_POINT('',(-8.60795233719346,-0.48724165907481,-81.3));
#38192=CARTESIAN_POINT('',(-8.60795233719346,-0.487241659074809,-81.3));
#38193=CARTESIAN_POINT('',(-8.60795233719346,-0.48724165907481,-81.35));
#38194=CARTESIAN_POINT('Origin',(-8.21904360754086,-0.87615038872741,-81.35));
#38195=CARTESIAN_POINT('',(-8.76432075605962,-0.804227990941668,-81.3));
#38196=CARTESIAN_POINT('Origin',(-8.21904360754086,-0.87615038872741,-81.3));
#38197=CARTESIAN_POINT('',(-8.76432075605962,-0.804227990941668,-81.35));
#38198=CARTESIAN_POINT('Origin',(-10.995,-0.510000000000002,-81.35));
#38199=CARTESIAN_POINT('',(-10.7007720090583,-2.74067924394038,-81.3));
#38200=CARTESIAN_POINT('Origin',(-10.995,-0.510000000000002,-81.3));
#38201=CARTESIAN_POINT('',(-10.7007720090583,-2.74067924394038,-81.35));
#38202=CARTESIAN_POINT('Origin',(-10.6288496112726,-3.28595639245914,-81.35));
#38203=CARTESIAN_POINT('',(-11.0177583409252,-2.89704766280654,-81.3));
#38204=CARTESIAN_POINT('Origin',(-10.6288496112726,-3.28595639245914,-81.3));
#38205=CARTESIAN_POINT('',(-11.0177583409252,-2.89704766280654,-81.35));
#38206=CARTESIAN_POINT('Origin',(-11.3889087296526,-3.26819805153396,-81.35));
#38207=CARTESIAN_POINT('',(-11.3889087296526,-3.26819805153396,-81.3));
#38208=CARTESIAN_POINT('',(-11.3889087296526,-3.26819805153396,-81.3));
#38209=CARTESIAN_POINT('',(-11.3889087296526,-3.26819805153396,-81.35));
#38210=CARTESIAN_POINT('Origin',(-11.,-3.65710678118656,-81.35));
#38211=CARTESIAN_POINT('',(-11.55,-3.65710678118656,-81.3));
#38212=CARTESIAN_POINT('Origin',(-11.,-3.65710678118656,-81.3));
#38213=CARTESIAN_POINT('',(-11.55,-3.65710678118656,-81.35));
#38214=CARTESIAN_POINT('Origin',(-11.55,-4.54289321881346,-81.35));
#38215=CARTESIAN_POINT('',(-11.55,-4.54289321881346,-81.3));
#38216=CARTESIAN_POINT('',(-11.55,-4.54289321881346,-81.3));
#38217=CARTESIAN_POINT('',(-11.55,-4.54289321881346,-81.35));
#38218=CARTESIAN_POINT('Origin',(-11.,-4.54289321881346,-81.35));
#38219=CARTESIAN_POINT('',(-11.3889087296526,-4.93180194846607,-81.3));
#38220=CARTESIAN_POINT('Origin',(-11.,-4.54289321881346,-81.3));
#38221=CARTESIAN_POINT('',(-11.3889087296526,-4.93180194846607,-81.35));
#38222=CARTESIAN_POINT('Origin',(-11.0177583409252,-5.30295233719346,-81.35));
#38223=CARTESIAN_POINT('',(-11.0177583409252,-5.30295233719346,-81.3));
#38224=CARTESIAN_POINT('',(-11.0177583409252,-5.30295233719346,-81.3));
#38225=CARTESIAN_POINT('',(-11.0177583409252,-5.30295233719346,-81.35));
#38226=CARTESIAN_POINT('Origin',(-10.6288496112726,-4.91404360754086,-81.35));
#38227=CARTESIAN_POINT('',(-10.7007720090583,-5.45932075605962,-81.3));
#38228=CARTESIAN_POINT('Origin',(-10.6288496112726,-4.91404360754086,-81.3));
#38229=CARTESIAN_POINT('',(-10.7007720090583,-5.45932075605962,-81.35));
#38230=CARTESIAN_POINT('Origin',(-10.995,-7.69,-81.35));
#38231=CARTESIAN_POINT('',(-8.76432075605962,-7.39577200905833,-81.3));
#38232=CARTESIAN_POINT('Origin',(-10.995,-7.69,-81.3));
#38233=CARTESIAN_POINT('',(-8.76432075605962,-7.39577200905833,-81.35));
#38234=CARTESIAN_POINT('Origin',(-8.21904360754086,-7.32384961127259,-81.35));
#38235=CARTESIAN_POINT('',(-8.60795233719346,-7.7127583409252,-81.3));
#38236=CARTESIAN_POINT('Origin',(-8.21904360754086,-7.32384961127259,-81.3));
#38237=CARTESIAN_POINT('',(-8.60795233719346,-7.7127583409252,-81.35));
#38238=CARTESIAN_POINT('Origin',(-8.23180194846605,-8.0889087296526,-81.35));
#38239=CARTESIAN_POINT('',(-8.23180194846605,-8.0889087296526,-81.3));
#38240=CARTESIAN_POINT('',(-8.23180194846605,-8.0889087296526,-81.3));
#38241=CARTESIAN_POINT('',(-8.23180194846605,-8.0889087296526,-81.35));
#38242=CARTESIAN_POINT('Origin',(-8.55,-8.40710678118654,-81.35));
#38243=CARTESIAN_POINT('',(-8.1,-8.40710678118654,-81.3));
#38244=CARTESIAN_POINT('Origin',(-8.55,-8.40710678118654,-81.3));
#38245=CARTESIAN_POINT('',(-8.1,-8.40710678118654,-81.35));
#38246=CARTESIAN_POINT('Origin',(-8.1,-12.0328932188134,-81.35));
#38247=CARTESIAN_POINT('',(-8.1,-12.0328932188134,-81.3));
#38248=CARTESIAN_POINT('',(-8.1,-12.0328932188134,-81.3));
#38249=CARTESIAN_POINT('',(-8.1,-12.0328932188134,-81.35));
#38250=CARTESIAN_POINT('Origin',(-8.55,-12.0328932188134,-81.35));
#38251=CARTESIAN_POINT('',(-8.23180194846605,-12.3510912703474,-81.3));
#38252=CARTESIAN_POINT('Origin',(-8.55,-12.0328932188134,-81.3));
#38253=CARTESIAN_POINT('',(-8.23180194846605,-12.3510912703474,-81.35));
#38254=CARTESIAN_POINT('Origin',(-12.3307106781186,-16.45,-81.35));
#38255=CARTESIAN_POINT('',(-12.3307106781186,-16.45,-81.3));
#38256=CARTESIAN_POINT('',(-12.3307106781186,-16.45,-81.3));
#38257=CARTESIAN_POINT('',(-12.3307106781186,-16.45,-81.35));
#38258=CARTESIAN_POINT('Origin',(-22.1792893218814,-16.45,-81.35));
#38259=CARTESIAN_POINT('',(-22.1792893218814,-16.45,-81.3));
#38260=CARTESIAN_POINT('',(-22.1792893218814,-16.45,-81.3));
#38261=CARTESIAN_POINT('',(-22.1792893218814,-16.45,-81.35));
#38262=CARTESIAN_POINT('Origin',(-23.15,-15.4792893218813,-81.35));
#38263=CARTESIAN_POINT('',(-23.15,-15.4792893218813,-81.3));
#38264=CARTESIAN_POINT('',(-23.15,-15.4792893218813,-81.3));
#38265=CARTESIAN_POINT('',(-23.15,-15.4792893218813,-81.35));
#38266=CARTESIAN_POINT('Origin',(-23.15,11.9792893218814,-81.35));
#38267=CARTESIAN_POINT('',(-23.15,11.9792893218814,-81.3));
#38268=CARTESIAN_POINT('',(-23.15,11.9792893218814,-81.3));
#38269=CARTESIAN_POINT('',(-23.15,11.9792893218814,-81.35));
#38270=CARTESIAN_POINT('Origin',(-22.1792893218813,12.95,-81.35));
#38271=CARTESIAN_POINT('',(-22.1792893218813,12.95,-81.3));
#38272=CARTESIAN_POINT('',(-22.1792893218813,12.95,-81.3));
#38273=CARTESIAN_POINT('',(-22.1792893218813,12.95,-81.35));
#38274=CARTESIAN_POINT('Origin',(22.1792893218813,12.95,-81.35));
#38275=CARTESIAN_POINT('',(22.1792893218813,12.95,-81.3));
#38276=CARTESIAN_POINT('',(22.1792893218813,12.95,-81.3));
#38277=CARTESIAN_POINT('',(22.1792893218813,12.95,-81.35));
#38278=CARTESIAN_POINT('Origin',(23.15,11.9792893218814,-81.35));
#38279=CARTESIAN_POINT('',(23.15,11.9792893218814,-81.3));
#38280=CARTESIAN_POINT('',(23.15,11.9792893218814,-81.3));
#38281=CARTESIAN_POINT('',(23.15,11.9792893218814,-81.35));
#38282=CARTESIAN_POINT('Origin',(23.15,-15.4792893218813,-81.35));
#38283=CARTESIAN_POINT('',(23.15,-15.4792893218813,-81.3));
#38284=CARTESIAN_POINT('',(23.15,-15.4792893218813,-81.3));
#38285=CARTESIAN_POINT('',(23.15,-15.4792893218813,-81.35));
#38286=CARTESIAN_POINT('Origin',(22.1792893218814,-16.45,-81.35));
#38287=CARTESIAN_POINT('',(22.1792893218814,-16.45,-81.3));
#38288=CARTESIAN_POINT('',(22.1792893218814,-16.45,-81.3));
#38289=CARTESIAN_POINT('',(22.1792893218814,-16.45,-81.35));
#38290=CARTESIAN_POINT('Origin',(12.3307106781187,-16.45,-81.35));
#38291=CARTESIAN_POINT('',(12.3307106781187,-16.45,-81.3));
#38292=CARTESIAN_POINT('Origin',(-1.62630325872826E-14,12.5,-10.6));
#38293=CARTESIAN_POINT('Origin',(-1.50786351795467E-14,12.7,-8.1));
#38294=CARTESIAN_POINT('',(-0.500000000000016,12.7,-8.1));
#38295=CARTESIAN_POINT('',(-0.500000000000016,12.7,-8.1));
#38296=CARTESIAN_POINT('',(0.499999999999983,12.7,-8.1));
#38297=CARTESIAN_POINT('Origin',(-1.50786351795467E-14,12.7,-8.1));
#38298=CARTESIAN_POINT('',(0.499999999999983,12.7,-8.1));
#38299=CARTESIAN_POINT('Origin',(0.,0.,0.));
#38300=CARTESIAN_POINT('',(4.99995,13.,0.));
#38301=CARTESIAN_POINT('',(22.2,13.,0.));
#38302=CARTESIAN_POINT('',(-22.2,13.,0.));
#38303=CARTESIAN_POINT('',(4.99995,8.,0.));
#38304=CARTESIAN_POINT('',(4.99995,13.,0.));
#38305=CARTESIAN_POINT('',(-4.99995,8.,0.));
#38306=CARTESIAN_POINT('Origin',(0.,8.,0.));
#38307=CARTESIAN_POINT('',(-4.99995,13.,0.));
#38308=CARTESIAN_POINT('',(-4.99995,13.,0.));
#38309=CARTESIAN_POINT('',(-22.2,13.,0.));
#38310=CARTESIAN_POINT('',(-22.2,13.,0.));
#38311=CARTESIAN_POINT('',(-23.2,12.,0.));
#38312=CARTESIAN_POINT('',(-22.2,13.,0.));
#38313=CARTESIAN_POINT('',(-23.2,-15.5,0.));
#38314=CARTESIAN_POINT('',(-23.2,12.,0.));
#38315=CARTESIAN_POINT('',(-22.2,-16.5,0.));
#38316=CARTESIAN_POINT('',(-23.2,-15.5,0.));
#38317=CARTESIAN_POINT('',(-12.31,-16.5,0.));
#38318=CARTESIAN_POINT('',(-23.,-16.5,0.));
#38319=CARTESIAN_POINT('',(-8.19644660940672,-12.3864466094067,0.));
#38320=CARTESIAN_POINT('',(-12.31,-16.5,0.));
#38321=CARTESIAN_POINT('',(-8.05,-12.0328932188134,0.));
#38322=CARTESIAN_POINT('Origin',(-8.55,-12.0328932188134,0.));
#38323=CARTESIAN_POINT('',(-8.05,-8.40710678118654,0.));
#38324=CARTESIAN_POINT('',(-8.05,-12.24,0.));
#38325=CARTESIAN_POINT('',(-8.19644660940673,-8.05355339059327,0.));
#38326=CARTESIAN_POINT('Origin',(-8.55,-8.40710678118654,0.));
#38327=CARTESIAN_POINT('',(-8.57259699813413,-7.67740300186587,0.));
#38328=CARTESIAN_POINT('',(-8.05,-8.2,0.));
#38329=CARTESIAN_POINT('',(-8.71475010619428,-7.38923360925963,0.));
#38330=CARTESIAN_POINT('Origin',(-8.21904360754086,-7.32384961127259,0.));
#38331=CARTESIAN_POINT('',(-10.6942336092596,-5.40975010619428,0.));
#38332=CARTESIAN_POINT('Origin',(-10.995,-7.69,0.));
#38333=CARTESIAN_POINT('',(-10.9824030018659,-5.26759699813413,0.));
#38334=CARTESIAN_POINT('Origin',(-10.6288496112726,-4.91404360754086,0.));
#38335=CARTESIAN_POINT('',(-11.3535533905933,-4.89644660940674,0.));
#38336=CARTESIAN_POINT('',(-8.05,-8.2,0.));
#38337=CARTESIAN_POINT('',(-11.5,-4.54289321881346,0.));
#38338=CARTESIAN_POINT('Origin',(-11.,-4.54289321881346,0.));
#38339=CARTESIAN_POINT('',(-11.5,-3.65710678118656,0.));
#38340=CARTESIAN_POINT('',(-11.5,-4.75000000000001,0.));
#38341=CARTESIAN_POINT('',(-11.3535533905933,-3.30355339059329,0.));
#38342=CARTESIAN_POINT('Origin',(-11.,-3.65710678118656,0.));
#38343=CARTESIAN_POINT('',(-10.9824030018659,-2.93240300186587,0.));
#38344=CARTESIAN_POINT('',(-8.05,-1.60428730688303E-15,0.));
#38345=CARTESIAN_POINT('',(-10.6942336092596,-2.79024989380572,0.));
#38346=CARTESIAN_POINT('Origin',(-10.6288496112726,-3.28595639245914,0.));
#38347=CARTESIAN_POINT('',(-8.71475010619428,-0.810766390740372,0.));
#38348=CARTESIAN_POINT('Origin',(-10.995,-0.510000000000002,0.));
#38349=CARTESIAN_POINT('',(-8.57259699813413,-0.522596998134137,0.));
#38350=CARTESIAN_POINT('Origin',(-8.21904360754086,-0.87615038872741,0.));
#38351=CARTESIAN_POINT('',(-8.05,-1.60428730688303E-15,0.));
#38352=CARTESIAN_POINT('',(-8.05,-1.60428730688303E-15,0.));
#38353=CARTESIAN_POINT('',(8.05,3.67394039744206E-16,0.));
#38354=CARTESIAN_POINT('',(8.05,3.67394039744206E-16,0.));
#38355=CARTESIAN_POINT('',(8.57259699813413,-0.522596998134133,0.));
#38356=CARTESIAN_POINT('',(8.05,3.67394039744206E-16,0.));
#38357=CARTESIAN_POINT('',(8.71475010619428,-0.81076639074037,0.));
#38358=CARTESIAN_POINT('Origin',(8.21904360754086,-0.876150388727407,0.));
#38359=CARTESIAN_POINT('',(10.6942336092596,-2.79024989380572,0.));
#38360=CARTESIAN_POINT('Origin',(10.995,-0.509999999999999,0.));
#38361=CARTESIAN_POINT('',(10.9824030018659,-2.93240300186586,0.));
#38362=CARTESIAN_POINT('Origin',(10.6288496112726,-3.28595639245914,0.));
#38363=CARTESIAN_POINT('',(11.3535533905933,-3.30355339059329,0.));
#38364=CARTESIAN_POINT('',(8.05,3.67394039744206E-16,0.));
#38365=CARTESIAN_POINT('',(11.5,-3.65710678118656,0.));
#38366=CARTESIAN_POINT('Origin',(11.,-3.65710678118656,0.));
#38367=CARTESIAN_POINT('',(11.5,-4.54289321881346,0.));
#38368=CARTESIAN_POINT('',(11.5,-4.75000000000001,0.));
#38369=CARTESIAN_POINT('',(11.3535533905933,-4.89644660940673,0.));
#38370=CARTESIAN_POINT('Origin',(11.,-4.54289321881346,0.));
#38371=CARTESIAN_POINT('',(10.9824030018659,-5.26759699813413,0.));
#38372=CARTESIAN_POINT('',(8.05,-8.2,0.));
#38373=CARTESIAN_POINT('',(10.6942336092596,-5.40975010619428,0.));
#38374=CARTESIAN_POINT('Origin',(10.6288496112726,-4.91404360754086,0.));
#38375=CARTESIAN_POINT('',(8.71475010619428,-7.38923360925963,0.));
#38376=CARTESIAN_POINT('Origin',(10.995,-7.69,0.));
#38377=CARTESIAN_POINT('',(8.57259699813413,-7.67740300186587,0.));
#38378=CARTESIAN_POINT('Origin',(8.21904360754086,-7.32384961127259,0.));
#38379=CARTESIAN_POINT('',(8.19644660940673,-8.05355339059327,0.));
#38380=CARTESIAN_POINT('',(8.05,-8.2,0.));
#38381=CARTESIAN_POINT('',(8.05,-8.40710678118654,0.));
#38382=CARTESIAN_POINT('Origin',(8.55,-8.40710678118654,0.));
#38383=CARTESIAN_POINT('',(8.05,-12.0328932188134,0.));
#38384=CARTESIAN_POINT('',(8.05,-12.24,0.));
#38385=CARTESIAN_POINT('',(8.19644660940673,-12.3864466094067,0.));
#38386=CARTESIAN_POINT('Origin',(8.55,-12.0328932188134,0.));
#38387=CARTESIAN_POINT('',(12.31,-16.5,0.));
#38388=CARTESIAN_POINT('',(12.31,-16.5,0.));
#38389=CARTESIAN_POINT('',(22.2,-16.5,0.));
#38390=CARTESIAN_POINT('',(12.31,-16.5,0.));
#38391=CARTESIAN_POINT('',(23.2,-15.5,0.));
#38392=CARTESIAN_POINT('',(23.2,-15.5,0.));
#38393=CARTESIAN_POINT('',(23.2,12.,0.));
#38394=CARTESIAN_POINT('',(23.2,12.,0.));
#38395=CARTESIAN_POINT('',(22.2,13.,0.));
#38396=CARTESIAN_POINT('Origin',(0.499999999999983,12.7,-8.1));
#38397=CARTESIAN_POINT('',(0.499999999999983,13.,-8.1));
#38398=CARTESIAN_POINT('',(0.499999999999983,13.,-8.1));
#38399=CARTESIAN_POINT('',(0.499999999999983,12.7,-8.1));
#38400=CARTESIAN_POINT('Origin',(-0.500000000000016,12.7,-8.1));
#38401=CARTESIAN_POINT('',(-0.500000000000017,13.,-8.1));
#38402=CARTESIAN_POINT('',(-0.500000000000017,13.,-8.1));
#38403=CARTESIAN_POINT('',(-0.500000000000016,12.7,-8.1));
#38404=CARTESIAN_POINT('Origin',(-1.50786351795467E-14,12.7,-8.1));
#38405=CARTESIAN_POINT('Origin',(-1.54689479616415E-14,13.,-8.1));
#38406=CARTESIAN_POINT('Origin',(-1.87674352915389E-14,12.5,-74.2));
#38407=CARTESIAN_POINT('Origin',(-1.50786351795467E-14,12.7,-76.7));
#38408=CARTESIAN_POINT('',(0.499999999999986,12.7,-76.7));
#38409=CARTESIAN_POINT('',(0.499999999999986,12.7,-76.7));
#38410=CARTESIAN_POINT('',(-0.500000000000025,12.7,-76.7));
#38411=CARTESIAN_POINT('Origin',(-1.50786351795467E-14,12.7,-76.7));
#38412=CARTESIAN_POINT('',(-0.500000000000025,12.7,-76.7));
#38413=CARTESIAN_POINT('Origin',(12.31,-16.5,-84.8));
#38414=CARTESIAN_POINT('',(12.31,-16.5,-3.45));
#38415=CARTESIAN_POINT('',(22.2,-16.5,-3.45));
#38416=CARTESIAN_POINT('',(12.31,-16.5,-3.45));
#38417=CARTESIAN_POINT('',(22.2,-16.5,-13.4));
#38418=CARTESIAN_POINT('',(12.31,-16.5,-84.8));
#38419=CARTESIAN_POINT('Origin',(23.2,-15.5,-13.4));
#38420=CARTESIAN_POINT('',(23.2,-15.5,-3.45));
#38421=CARTESIAN_POINT('',(22.2,-16.5,-3.45));
#38422=CARTESIAN_POINT('',(23.2,-15.5,-13.4));
#38423=CARTESIAN_POINT('Origin',(23.2,12.,-13.4));
#38424=CARTESIAN_POINT('',(23.2,12.,-3.45));
#38425=CARTESIAN_POINT('',(23.2,-15.5,-3.45));
#38426=CARTESIAN_POINT('',(23.2,12.,-13.4));
#38427=CARTESIAN_POINT('Origin',(22.2,13.,-13.4));
#38428=CARTESIAN_POINT('',(22.2,13.,-3.45));
#38429=CARTESIAN_POINT('',(23.2,12.,-3.45));
#38430=CARTESIAN_POINT('',(22.2,13.,-13.4));
#38431=CARTESIAN_POINT('Origin',(-22.2,13.,-13.4));
#38432=CARTESIAN_POINT('',(4.99995,13.,-0.999999999999999));
#38433=CARTESIAN_POINT('',(-4.99995,13.,-1.));
#38434=CARTESIAN_POINT('',(-4.99995,13.,-1.));
#38435=CARTESIAN_POINT('',(4.99995,13.,-1.));
#38436=CARTESIAN_POINT('',(-22.2,13.,-3.45));
#38437=CARTESIAN_POINT('',(22.2,13.,-3.45));
#38438=CARTESIAN_POINT('',(-22.2,13.,-13.4));
#38439=CARTESIAN_POINT('',(-4.99995,13.,-1.));
#38440=CARTESIAN_POINT('Origin',(-22.2,13.,-13.4));
#38441=CARTESIAN_POINT('',(-23.2,12.,-3.45));
#38442=CARTESIAN_POINT('',(-22.2,13.,-3.45));
#38443=CARTESIAN_POINT('',(-23.2,12.,-13.4));
#38444=CARTESIAN_POINT('Origin',(-23.2,12.,-13.4));
#38445=CARTESIAN_POINT('',(-23.2,-15.5,-3.45));
#38446=CARTESIAN_POINT('',(-23.2,12.,-3.45));
#38447=CARTESIAN_POINT('',(-23.2,-15.5,-13.4));
#38448=CARTESIAN_POINT('Origin',(-23.2,-15.5,-13.4));
#38449=CARTESIAN_POINT('',(-22.2,-16.5,-3.45));
#38450=CARTESIAN_POINT('',(-23.2,-15.5,-3.45));
#38451=CARTESIAN_POINT('',(-22.2,-16.5,-13.4));
#38452=CARTESIAN_POINT('Origin',(-23.,-16.5,-84.8));
#38453=CARTESIAN_POINT('',(-12.31,-16.5,-3.45));
#38454=CARTESIAN_POINT('',(-22.2,-16.5,-3.45));
#38455=CARTESIAN_POINT('',(-12.31,-16.5,-84.8));
#38456=CARTESIAN_POINT('Origin',(-12.31,-16.5,-84.8));
#38457=CARTESIAN_POINT('',(-8.19644660940672,-12.3864466094067,-3.45));
#38458=CARTESIAN_POINT('',(-12.31,-16.5,-3.45));
#38459=CARTESIAN_POINT('',(-8.19644660940672,-12.3864466094067,-84.8));
#38460=CARTESIAN_POINT('Origin',(-8.55,-12.0328932188134,-84.8));
#38461=CARTESIAN_POINT('',(-8.05,-12.0328932188134,-3.45));
#38462=CARTESIAN_POINT('Origin',(-8.55,-12.0328932188134,-3.45));
#38463=CARTESIAN_POINT('',(-8.05,-12.0328932188134,-84.8));
#38464=CARTESIAN_POINT('Origin',(-8.05,-12.24,-84.8));
#38465=CARTESIAN_POINT('',(-8.05,-8.40710678118654,-3.45));
#38466=CARTESIAN_POINT('',(-8.05,-12.0328932188134,-3.45));
#38467=CARTESIAN_POINT('',(-8.05,-8.40710678118654,-84.8));
#38468=CARTESIAN_POINT('Origin',(-8.55,-8.40710678118654,-84.8));
#38469=CARTESIAN_POINT('',(-8.19644660940673,-8.05355339059327,-3.45));
#38470=CARTESIAN_POINT('Origin',(-8.55,-8.40710678118654,-3.45));
#38471=CARTESIAN_POINT('',(-8.19644660940673,-8.05355339059327,-84.8));
#38472=CARTESIAN_POINT('Origin',(-8.05,-8.2,-84.8));
#38473=CARTESIAN_POINT('',(-8.57259699813413,-7.67740300186587,-3.45));
#38474=CARTESIAN_POINT('',(-8.19644660940673,-8.05355339059327,-3.45));
#38475=CARTESIAN_POINT('',(-8.57259699813413,-7.67740300186587,0.));
#38476=CARTESIAN_POINT('Origin',(-8.21904360754086,-7.32384961127259,-84.8));
#38477=CARTESIAN_POINT('',(-8.71475010619428,-7.38923360925963,-3.45));
#38478=CARTESIAN_POINT('Origin',(-8.21904360754086,-7.32384961127259,-3.45));
#38479=CARTESIAN_POINT('',(-8.71475010619428,-7.38923360925963,-84.8));
#38480=CARTESIAN_POINT('Origin',(-10.995,-7.69,-84.8));
#38481=CARTESIAN_POINT('',(-10.6942336092596,-5.40975010619428,-3.45));
#38482=CARTESIAN_POINT('Origin',(-10.995,-7.69,-3.45));
#38483=CARTESIAN_POINT('',(-10.6942336092596,-5.40975010619428,-84.8));
#38484=CARTESIAN_POINT('Origin',(-10.6288496112726,-4.91404360754086,-84.8));
#38485=CARTESIAN_POINT('',(-10.9824030018659,-5.26759699813413,-3.45));
#38486=CARTESIAN_POINT('Origin',(-10.6288496112726,-4.91404360754086,-3.45));
#38487=CARTESIAN_POINT('',(-10.9824030018659,-5.26759699813413,-84.8));
#38488=CARTESIAN_POINT('Origin',(-8.05,-8.2,-84.8));
#38489=CARTESIAN_POINT('',(-11.3535533905933,-4.89644660940674,-3.45));
#38490=CARTESIAN_POINT('',(-10.9824030018659,-5.26759699813413,-3.45));
#38491=CARTESIAN_POINT('',(-11.3535533905933,-4.89644660940674,0.));
#38492=CARTESIAN_POINT('Origin',(-11.,-4.54289321881346,-84.8));
#38493=CARTESIAN_POINT('',(-11.5,-4.54289321881346,-3.45));
#38494=CARTESIAN_POINT('Origin',(-11.,-4.54289321881346,-3.45));
#38495=CARTESIAN_POINT('',(-11.5,-4.54289321881346,-84.8));
#38496=CARTESIAN_POINT('Origin',(-11.5,-4.75000000000001,-84.8));
#38497=CARTESIAN_POINT('',(-11.5,-3.65710678118656,-3.45));
#38498=CARTESIAN_POINT('',(-11.5,-4.54289321881346,-3.45));
#38499=CARTESIAN_POINT('',(-11.5,-3.65710678118656,0.));
#38500=CARTESIAN_POINT('Origin',(-11.,-3.65710678118656,-84.8));
#38501=CARTESIAN_POINT('',(-11.3535533905933,-3.30355339059329,-3.45));
#38502=CARTESIAN_POINT('Origin',(-11.,-3.65710678118656,-3.45));
#38503=CARTESIAN_POINT('',(-11.3535533905933,-3.30355339059329,-84.8));
#38504=CARTESIAN_POINT('Origin',(-8.05,-1.60428730688303E-15,-84.8));
#38505=CARTESIAN_POINT('',(-10.9824030018659,-2.93240300186587,-3.45));
#38506=CARTESIAN_POINT('',(-11.3535533905933,-3.30355339059329,-3.45));
#38507=CARTESIAN_POINT('',(-10.9824030018659,-2.93240300186587,0.));
#38508=CARTESIAN_POINT('Origin',(-10.6288496112726,-3.28595639245914,-84.8));
#38509=CARTESIAN_POINT('',(-10.6942336092596,-2.79024989380572,-3.45));
#38510=CARTESIAN_POINT('Origin',(-10.6288496112726,-3.28595639245914,-3.45));
#38511=CARTESIAN_POINT('',(-10.6942336092596,-2.79024989380572,-84.8));
#38512=CARTESIAN_POINT('Origin',(-10.995,-0.510000000000002,-84.8));
#38513=CARTESIAN_POINT('',(-8.71475010619428,-0.810766390740372,-3.45));
#38514=CARTESIAN_POINT('Origin',(-10.995,-0.510000000000002,-3.45));
#38515=CARTESIAN_POINT('',(-8.71475010619428,-0.810766390740372,-84.8));
#38516=CARTESIAN_POINT('Origin',(-8.21904360754086,-0.87615038872741,-84.8));
#38517=CARTESIAN_POINT('',(-8.57259699813413,-0.522596998134137,-3.45));
#38518=CARTESIAN_POINT('Origin',(-8.21904360754086,-0.87615038872741,-3.45));
#38519=CARTESIAN_POINT('',(-8.57259699813413,-0.522596998134137,-84.8));
#38520=CARTESIAN_POINT('Origin',(-8.05,-1.60428730688303E-15,-84.8));
#38521=CARTESIAN_POINT('',(-8.05,-1.60428730688303E-15,-3.45));
#38522=CARTESIAN_POINT('',(-8.57259699813413,-0.522596998134137,-3.45));
#38523=CARTESIAN_POINT('',(-8.05,-1.60428730688303E-15,-84.8));
#38524=CARTESIAN_POINT('Origin',(8.05,3.67394039744206E-16,-84.8));
#38525=CARTESIAN_POINT('',(8.05,3.67394039744206E-16,-3.45));
#38526=CARTESIAN_POINT('',(-8.05,-1.60428730688303E-15,-3.45));
#38527=CARTESIAN_POINT('',(8.05,3.67394039744206E-16,-84.8));
#38528=CARTESIAN_POINT('Origin',(8.05,3.67394039744206E-16,-84.8));
#38529=CARTESIAN_POINT('',(8.57259699813413,-0.522596998134133,-3.45));
#38530=CARTESIAN_POINT('',(8.05,3.67394039744206E-16,-3.45));
#38531=CARTESIAN_POINT('',(8.57259699813413,-0.522596998134133,0.));
#38532=CARTESIAN_POINT('Origin',(8.21904360754086,-0.876150388727407,-84.8));
#38533=CARTESIAN_POINT('',(8.71475010619428,-0.81076639074037,-3.45));
#38534=CARTESIAN_POINT('Origin',(8.21904360754086,-0.876150388727407,-3.45));
#38535=CARTESIAN_POINT('',(8.71475010619428,-0.81076639074037,-84.8));
#38536=CARTESIAN_POINT('Origin',(10.995,-0.509999999999999,-84.8));
#38537=CARTESIAN_POINT('',(10.6942336092596,-2.79024989380572,-3.45));
#38538=CARTESIAN_POINT('Origin',(10.995,-0.509999999999999,-3.45));
#38539=CARTESIAN_POINT('',(10.6942336092596,-2.79024989380572,-84.8));
#38540=CARTESIAN_POINT('Origin',(10.6288496112726,-3.28595639245914,-84.8));
#38541=CARTESIAN_POINT('',(10.9824030018659,-2.93240300186586,-3.45));
#38542=CARTESIAN_POINT('Origin',(10.6288496112726,-3.28595639245914,-3.45));
#38543=CARTESIAN_POINT('',(10.9824030018659,-2.93240300186586,-84.8));
#38544=CARTESIAN_POINT('Origin',(8.05,3.67394039744206E-16,-84.8));
#38545=CARTESIAN_POINT('',(11.3535533905933,-3.30355339059329,-3.45));
#38546=CARTESIAN_POINT('',(10.9824030018659,-2.93240300186586,-3.45));
#38547=CARTESIAN_POINT('',(11.3535533905933,-3.30355339059329,0.));
#38548=CARTESIAN_POINT('Origin',(11.,-3.65710678118656,-84.8));
#38549=CARTESIAN_POINT('',(11.5,-3.65710678118656,-3.45));
#38550=CARTESIAN_POINT('Origin',(11.,-3.65710678118656,-3.45));
#38551=CARTESIAN_POINT('',(11.5,-3.65710678118656,-84.8));
#38552=CARTESIAN_POINT('Origin',(11.5,-4.75000000000001,-84.8));
#38553=CARTESIAN_POINT('',(11.5,-4.54289321881346,-3.45));
#38554=CARTESIAN_POINT('',(11.5,-3.65710678118656,-3.45));
#38555=CARTESIAN_POINT('',(11.5,-4.54289321881346,0.));
#38556=CARTESIAN_POINT('Origin',(11.,-4.54289321881346,-84.8));
#38557=CARTESIAN_POINT('',(11.3535533905933,-4.89644660940673,-3.45));
#38558=CARTESIAN_POINT('Origin',(11.,-4.54289321881346,-3.45));
#38559=CARTESIAN_POINT('',(11.3535533905933,-4.89644660940673,-84.8));
#38560=CARTESIAN_POINT('Origin',(8.05,-8.2,-84.8));
#38561=CARTESIAN_POINT('',(10.9824030018659,-5.26759699813413,-3.45));
#38562=CARTESIAN_POINT('',(11.3535533905933,-4.89644660940673,-3.45));
#38563=CARTESIAN_POINT('',(10.9824030018659,-5.26759699813413,0.));
#38564=CARTESIAN_POINT('Origin',(10.6288496112726,-4.91404360754086,-84.8));
#38565=CARTESIAN_POINT('',(10.6942336092596,-5.40975010619428,-3.45));
#38566=CARTESIAN_POINT('Origin',(10.6288496112726,-4.91404360754086,-3.45));
#38567=CARTESIAN_POINT('',(10.6942336092596,-5.40975010619428,-84.8));
#38568=CARTESIAN_POINT('Origin',(10.995,-7.69,-84.8));
#38569=CARTESIAN_POINT('',(8.71475010619428,-7.38923360925963,-3.45));
#38570=CARTESIAN_POINT('Origin',(10.995,-7.69,-3.45));
#38571=CARTESIAN_POINT('',(8.71475010619428,-7.38923360925963,-84.8));
#38572=CARTESIAN_POINT('Origin',(8.21904360754086,-7.32384961127259,-84.8));
#38573=CARTESIAN_POINT('',(8.57259699813413,-7.67740300186587,-3.45));
#38574=CARTESIAN_POINT('Origin',(8.21904360754086,-7.32384961127259,-3.45));
#38575=CARTESIAN_POINT('',(8.57259699813413,-7.67740300186587,-84.8));
#38576=CARTESIAN_POINT('Origin',(8.05,-8.2,-84.8));
#38577=CARTESIAN_POINT('',(8.19644660940673,-8.05355339059327,-3.45));
#38578=CARTESIAN_POINT('',(8.57259699813413,-7.67740300186587,-3.45));
#38579=CARTESIAN_POINT('',(8.19644660940673,-8.05355339059327,-84.8));
#38580=CARTESIAN_POINT('Origin',(8.55,-8.40710678118654,-84.8));
#38581=CARTESIAN_POINT('',(8.05,-8.40710678118654,-3.45));
#38582=CARTESIAN_POINT('Origin',(8.55,-8.40710678118654,-3.45));
#38583=CARTESIAN_POINT('',(8.05,-8.40710678118654,-84.8));
#38584=CARTESIAN_POINT('Origin',(8.05,-12.24,-84.8));
#38585=CARTESIAN_POINT('',(8.05,-12.0328932188134,-3.45));
#38586=CARTESIAN_POINT('',(8.05,-8.40710678118654,-3.45));
#38587=CARTESIAN_POINT('',(8.05,-12.0328932188134,-84.8));
#38588=CARTESIAN_POINT('Origin',(8.55,-12.0328932188134,-84.8));
#38589=CARTESIAN_POINT('',(8.19644660940673,-12.3864466094067,-3.45));
#38590=CARTESIAN_POINT('Origin',(8.55,-12.0328932188134,-3.45));
#38591=CARTESIAN_POINT('',(8.19644660940673,-12.3864466094067,-84.8));
#38592=CARTESIAN_POINT('Origin',(12.31,-16.5,-84.8));
#38593=CARTESIAN_POINT('',(8.19644660940673,-12.3864466094067,-3.45));
#38594=CARTESIAN_POINT('Origin',(-1.54689479616415E-14,13.,-8.1));
#38595=CARTESIAN_POINT('Origin',(-34.5,4.40457132572236E-15,-104.175753233145));
#38596=CARTESIAN_POINT('',(-30.9292009086072,4.33680868994202E-15,-59.4));
#38597=CARTESIAN_POINT('',(-30.9292009086072,4.33680868994202E-15,-25.4));
#38598=CARTESIAN_POINT('',(-30.9292009086072,4.37613505316247E-15,-13.4));
#38599=CARTESIAN_POINT('',(-34.,4.4005895457577E-15,-25.4));
#38600=CARTESIAN_POINT('',(-34.5,4.40457132572236E-15,-25.4));
#38601=CARTESIAN_POINT('',(-34.,4.4005895457577E-15,-59.4));
#38602=CARTESIAN_POINT('',(-34.,4.4005895457577E-15,-104.175753233145));
#38603=CARTESIAN_POINT('',(-34.5,4.40457132572236E-15,-59.4));
#38604=CARTESIAN_POINT('Origin',(35.,6.66784336078585E-15,-104.175753233145));
#38605=CARTESIAN_POINT('',(34.5,6.46233547508513E-15,-59.4));
#38606=CARTESIAN_POINT('',(34.5,6.46233547508513E-15,-25.4));
#38607=CARTESIAN_POINT('',(34.5,6.46233547508513E-15,-104.175753233145));
#38608=CARTESIAN_POINT('',(30.9292009086072,4.77048955893622E-15,-25.4));
#38609=CARTESIAN_POINT('',(35.,6.66784336078585E-15,-25.4));
#38610=CARTESIAN_POINT('',(30.9292009086072,4.99468073201678E-15,-59.4));
#38611=CARTESIAN_POINT('',(30.9292009086072,4.99468073201678E-15,-71.4));
#38612=CARTESIAN_POINT('',(35.,6.66784336078585E-15,-59.4));
#38613=CARTESIAN_POINT('Origin',(-0.500000000000025,12.7,-76.7));
#38614=CARTESIAN_POINT('',(-0.500000000000025,13.,-76.7));
#38615=CARTESIAN_POINT('',(-0.500000000000025,13.,-76.7));
#38616=CARTESIAN_POINT('',(-0.500000000000025,12.7,-76.7));
#38617=CARTESIAN_POINT('Origin',(0.499999999999986,12.7,-76.7));
#38618=CARTESIAN_POINT('',(0.499999999999986,13.,-76.7));
#38619=CARTESIAN_POINT('',(0.499999999999986,13.,-76.7));
#38620=CARTESIAN_POINT('',(0.499999999999986,12.7,-76.7));
#38621=CARTESIAN_POINT('Origin',(-1.50786351795467E-14,12.7,-76.7));
#38622=CARTESIAN_POINT('Origin',(-1.54689479616415E-14,13.,-76.7));
#38623=CARTESIAN_POINT('Origin',(-30.9292009086072,-2.,-104.175753233145));
#38624=CARTESIAN_POINT('',(-28.9973492560291,-1.48236190979496,-25.4));
#38625=CARTESIAN_POINT('Origin',(-30.9292009086072,-2.,-25.4));
#38626=CARTESIAN_POINT('',(-28.9973492560291,-1.48236190979496,-59.4));
#38627=CARTESIAN_POINT('Origin',(-30.9292009086072,-2.,-59.4));
#38628=CARTESIAN_POINT('',(-28.9973492560291,-1.48236190979496,-71.4));
#38629=CARTESIAN_POINT('Origin',(0.,0.,-25.4));
#38630=CARTESIAN_POINT('',(-25.7,-13.788236863595,-25.4));
#38631=CARTESIAN_POINT('',(-29.3945469326493,4.36391374425416E-15,-25.4));
#38632=CARTESIAN_POINT('',(-25.7,0.500000000000004,-25.4));
#38633=CARTESIAN_POINT('',(-25.7,-16.5,-25.4));
#38634=CARTESIAN_POINT('',(-34.5,0.500000000000005,-25.4));
#38635=CARTESIAN_POINT('',(-25.7,0.500000000000004,-25.4));
#38636=CARTESIAN_POINT('',(-34.5,0.500000000000005,-25.4));
#38637=CARTESIAN_POINT('Origin',(-25.7,-16.5,-25.4));
#38638=CARTESIAN_POINT('',(-25.7,-13.788236863595,-24.6339201514178));
#38639=CARTESIAN_POINT('',(-25.7,-13.788236863595,-104.175753233145));
#38640=CARTESIAN_POINT('',(-25.7,0.500000000000004,-24.6339201514178));
#38641=CARTESIAN_POINT('',(-25.7,24.2065391822594,-24.6339201514178));
#38642=CARTESIAN_POINT('',(-25.7,0.500000000000004,-25.4));
#38643=CARTESIAN_POINT('Origin',(25.7,0.500000000000004,-25.4));
#38644=CARTESIAN_POINT('',(25.7,0.500000000000004,-25.4));
#38645=CARTESIAN_POINT('',(25.7,0.499999999999997,-24.6339201514179));
#38646=CARTESIAN_POINT('',(25.7,0.500000000000004,-25.4));
#38647=CARTESIAN_POINT('',(25.7,-13.788236863595,-24.6339201514178));
#38648=CARTESIAN_POINT('',(25.7,24.2065391822594,-24.6339201514179));
#38649=CARTESIAN_POINT('',(25.7,-13.788236863595,-25.4));
#38650=CARTESIAN_POINT('',(25.7,-13.788236863595,-104.175753233145));
#38651=CARTESIAN_POINT('',(25.7,0.500000000000004,-25.4));
#38652=CARTESIAN_POINT('Origin',(0.,0.,-25.4));
#38653=CARTESIAN_POINT('',(28.9973492560291,-1.48236190979496,-25.4));
#38654=CARTESIAN_POINT('',(29.3945469326493,4.36391374425416E-15,-25.4));
#38655=CARTESIAN_POINT('Origin',(30.9292009086072,-2.,-25.4));
#38656=CARTESIAN_POINT('',(35.,0.500000000000005,-25.4));
#38657=CARTESIAN_POINT('',(34.5,6.46233547508513E-15,-25.4));
#38658=CARTESIAN_POINT('',(35.,0.500000000000005,-25.4));
#38659=CARTESIAN_POINT('Origin',(30.9292009086072,-2.,-104.175753233145));
#38660=CARTESIAN_POINT('',(28.9973492560291,-1.48236190979496,-59.4));
#38661=CARTESIAN_POINT('',(28.9973492560291,-1.48236190979496,-13.4));
#38662=CARTESIAN_POINT('Origin',(30.9292009086072,-2.,-59.4));
#38663=CARTESIAN_POINT('Origin',(-8.55,-12.0328932188134,-3.45));
#38664=CARTESIAN_POINT('',(12.3307106781187,-16.45,-3.45));
#38665=CARTESIAN_POINT('',(22.1792893218814,-16.45,-3.45));
#38666=CARTESIAN_POINT('',(12.3307106781187,-16.45,-3.45));
#38667=CARTESIAN_POINT('',(23.15,-15.4792893218813,-3.45));
#38668=CARTESIAN_POINT('',(22.1792893218814,-16.45,-3.45));
#38669=CARTESIAN_POINT('',(23.15,11.9792893218814,-3.45));
#38670=CARTESIAN_POINT('',(23.15,-15.4792893218813,-3.45));
#38671=CARTESIAN_POINT('',(22.1792893218813,12.95,-3.45));
#38672=CARTESIAN_POINT('',(23.15,11.9792893218814,-3.45));
#38673=CARTESIAN_POINT('',(-22.1792893218813,12.95,-3.45));
#38674=CARTESIAN_POINT('',(22.1792893218813,12.95,-3.45));
#38675=CARTESIAN_POINT('',(-23.15,11.9792893218814,-3.45));
#38676=CARTESIAN_POINT('',(-22.1792893218813,12.95,-3.45));
#38677=CARTESIAN_POINT('',(-23.15,-15.4792893218813,-3.45));
#38678=CARTESIAN_POINT('',(-23.15,11.9792893218814,-3.45));
#38679=CARTESIAN_POINT('',(-22.1792893218814,-16.45,-3.45));
#38680=CARTESIAN_POINT('',(-23.15,-15.4792893218813,-3.45));
#38681=CARTESIAN_POINT('',(-12.3307106781186,-16.45,-3.45));
#38682=CARTESIAN_POINT('',(-22.1792893218814,-16.45,-3.45));
#38683=CARTESIAN_POINT('',(-8.23180194846605,-12.3510912703474,-3.45));
#38684=CARTESIAN_POINT('',(-12.3307106781186,-16.45,-3.45));
#38685=CARTESIAN_POINT('',(-8.1,-12.0328932188134,-3.45));
#38686=CARTESIAN_POINT('Origin',(-8.55,-12.0328932188134,-3.45));
#38687=CARTESIAN_POINT('',(-8.1,-8.40710678118654,-3.45));
#38688=CARTESIAN_POINT('',(-8.1,-12.0328932188134,-3.45));
#38689=CARTESIAN_POINT('',(-8.23180194846605,-8.0889087296526,-3.45));
#38690=CARTESIAN_POINT('Origin',(-8.55,-8.40710678118654,-3.45));
#38691=CARTESIAN_POINT('',(-8.60795233719346,-7.7127583409252,-3.45));
#38692=CARTESIAN_POINT('',(-8.23180194846605,-8.0889087296526,-3.45));
#38693=CARTESIAN_POINT('',(-8.76432075605962,-7.39577200905833,-3.45));
#38694=CARTESIAN_POINT('Origin',(-8.21904360754086,-7.32384961127259,-3.45));
#38695=CARTESIAN_POINT('',(-10.7007720090583,-5.45932075605962,-3.45));
#38696=CARTESIAN_POINT('Origin',(-10.995,-7.69,-3.45));
#38697=CARTESIAN_POINT('',(-11.0177583409252,-5.30295233719346,-3.45));
#38698=CARTESIAN_POINT('Origin',(-10.6288496112726,-4.91404360754086,-3.45));
#38699=CARTESIAN_POINT('',(-11.3889087296526,-4.93180194846607,-3.45));
#38700=CARTESIAN_POINT('',(-11.0177583409252,-5.30295233719346,-3.45));
#38701=CARTESIAN_POINT('',(-11.55,-4.54289321881346,-3.45));
#38702=CARTESIAN_POINT('Origin',(-11.,-4.54289321881346,-3.45));
#38703=CARTESIAN_POINT('',(-11.55,-3.65710678118656,-3.45));
#38704=CARTESIAN_POINT('',(-11.55,-4.54289321881346,-3.45));
#38705=CARTESIAN_POINT('',(-11.3889087296526,-3.26819805153396,-3.45));
#38706=CARTESIAN_POINT('Origin',(-11.,-3.65710678118656,-3.45));
#38707=CARTESIAN_POINT('',(-11.0177583409252,-2.89704766280654,-3.45));
#38708=CARTESIAN_POINT('',(-11.3889087296526,-3.26819805153396,-3.45));
#38709=CARTESIAN_POINT('',(-10.7007720090583,-2.74067924394038,-3.45));
#38710=CARTESIAN_POINT('Origin',(-10.6288496112726,-3.28595639245914,-3.45));
#38711=CARTESIAN_POINT('',(-8.76432075605962,-0.804227990941668,-3.45));
#38712=CARTESIAN_POINT('Origin',(-10.995,-0.510000000000002,-3.45));
#38713=CARTESIAN_POINT('',(-8.60795233719346,-0.48724165907481,-3.45));
#38714=CARTESIAN_POINT('Origin',(-8.21904360754086,-0.87615038872741,-3.45));
#38715=CARTESIAN_POINT('',(-8.07071067811865,0.0499999999999998,-3.45));
#38716=CARTESIAN_POINT('',(-8.60795233719346,-0.487241659074809,-3.45));
#38717=CARTESIAN_POINT('',(8.07071067811865,0.0500000000000006,-3.45));
#38718=CARTESIAN_POINT('',(-8.07071067811865,0.0499999999999998,-3.45));
#38719=CARTESIAN_POINT('',(8.60795233719346,-0.487241659074806,-3.45));
#38720=CARTESIAN_POINT('',(8.07071067811865,0.0500000000000006,-3.45));
#38721=CARTESIAN_POINT('',(8.76432075605962,-0.804227990941667,-3.45));
#38722=CARTESIAN_POINT('Origin',(8.21904360754086,-0.876150388727407,-3.45));
#38723=CARTESIAN_POINT('',(10.7007720090583,-2.74067924394038,-3.45));
#38724=CARTESIAN_POINT('Origin',(10.995,-0.509999999999999,-3.45));
#38725=CARTESIAN_POINT('',(11.0177583409252,-2.89704766280654,-3.45));
#38726=CARTESIAN_POINT('Origin',(10.6288496112726,-3.28595639245914,-3.45));
#38727=CARTESIAN_POINT('',(11.3889087296526,-3.26819805153396,-3.45));
#38728=CARTESIAN_POINT('',(11.0177583409252,-2.89704766280654,-3.45));
#38729=CARTESIAN_POINT('',(11.55,-3.65710678118656,-3.45));
#38730=CARTESIAN_POINT('Origin',(11.,-3.65710678118656,-3.45));
#38731=CARTESIAN_POINT('',(11.55,-4.54289321881346,-3.45));
#38732=CARTESIAN_POINT('',(11.55,-3.65710678118656,-3.45));
#38733=CARTESIAN_POINT('',(11.3889087296526,-4.93180194846606,-3.45));
#38734=CARTESIAN_POINT('Origin',(11.,-4.54289321881346,-3.45));
#38735=CARTESIAN_POINT('',(11.0177583409252,-5.30295233719346,-3.45));
#38736=CARTESIAN_POINT('',(11.3889087296526,-4.93180194846606,-3.45));
#38737=CARTESIAN_POINT('',(10.7007720090583,-5.45932075605962,-3.45));
#38738=CARTESIAN_POINT('Origin',(10.6288496112726,-4.91404360754086,-3.45));
#38739=CARTESIAN_POINT('',(8.76432075605962,-7.39577200905833,-3.45));
#38740=CARTESIAN_POINT('Origin',(10.995,-7.69,-3.45));
#38741=CARTESIAN_POINT('',(8.60795233719346,-7.71275834092519,-3.45));
#38742=CARTESIAN_POINT('Origin',(8.21904360754086,-7.32384961127259,-3.45));
#38743=CARTESIAN_POINT('',(8.23180194846606,-8.08890872965259,-3.45));
#38744=CARTESIAN_POINT('',(8.60795233719346,-7.71275834092519,-3.45));
#38745=CARTESIAN_POINT('',(8.1,-8.40710678118654,-3.45));
#38746=CARTESIAN_POINT('Origin',(8.55,-8.40710678118654,-3.45));
#38747=CARTESIAN_POINT('',(8.1,-12.0328932188134,-3.45));
#38748=CARTESIAN_POINT('',(8.1,-8.40710678118654,-3.45));
#38749=CARTESIAN_POINT('',(8.23180194846605,-12.3510912703474,-3.45));
#38750=CARTESIAN_POINT('Origin',(8.55,-12.0328932188134,-3.45));
#38751=CARTESIAN_POINT('',(8.23180194846605,-12.3510912703474,-3.45));
#38752=CARTESIAN_POINT('Origin',(34.5,6.46233547508513E-15,-104.175753233145));
#38753=CARTESIAN_POINT('',(35.,0.500000000000005,-59.4));
#38754=CARTESIAN_POINT('',(35.,0.500000000000007,-104.175753233145));
#38755=CARTESIAN_POINT('',(34.5,6.46233547508513E-15,-59.4));
#38756=CARTESIAN_POINT('Origin',(-34.5,0.500000000000005,-104.175753233145));
#38757=CARTESIAN_POINT('',(-34.5,0.500000000000005,-59.4));
#38758=CARTESIAN_POINT('',(-34.5,0.500000000000005,-104.175753233145));
#38759=CARTESIAN_POINT('',(-34.5,0.500000000000005,-59.4));
#38760=CARTESIAN_POINT('Origin',(0.,0.,-59.4));
#38761=CARTESIAN_POINT('',(-25.7,0.500000000000004,-59.4));
#38762=CARTESIAN_POINT('',(-25.7,-13.788236863595,-59.4));
#38763=CARTESIAN_POINT('',(-25.7,0.500000000000004,-59.4));
#38764=CARTESIAN_POINT('',(-29.3945469326493,4.36391374425416E-15,-59.4));
#38765=CARTESIAN_POINT('',(-35.,0.500000000000005,-59.4));
#38766=CARTESIAN_POINT('Origin',(-25.7,0.500000000000004,-59.4));
#38767=CARTESIAN_POINT('',(-25.7,0.500000000000004,-60.1660798485821));
#38768=CARTESIAN_POINT('',(-25.7,0.500000000000004,-59.4));
#38769=CARTESIAN_POINT('',(-25.7,-13.788236863595,-60.1660798485821));
#38770=CARTESIAN_POINT('',(-25.7,24.2065391822594,-60.1660798485822));
#38771=CARTESIAN_POINT('',(-25.7,-13.788236863595,-104.175753233145));
#38772=CARTESIAN_POINT('Origin',(0.,0.,-59.4));
#38773=CARTESIAN_POINT('',(25.7,0.500000000000004,-59.4));
#38774=CARTESIAN_POINT('',(35.,0.500000000000005,-59.4));
#38775=CARTESIAN_POINT('',(25.7,-13.788236863595,-59.4));
#38776=CARTESIAN_POINT('',(29.3945469326493,4.36391374425416E-15,-59.4));
#38777=CARTESIAN_POINT('',(25.7,0.500000000000004,-59.4));
#38778=CARTESIAN_POINT('Origin',(25.7,0.500000000000004,-59.4));
#38779=CARTESIAN_POINT('',(25.7,-13.788236863595,-60.1660798485821));
#38780=CARTESIAN_POINT('',(25.7,-13.788236863595,-104.175753233145));
#38781=CARTESIAN_POINT('',(25.7,0.499999999999997,-60.1660798485821));
#38782=CARTESIAN_POINT('',(25.7,24.2065391822594,-60.1660798485821));
#38783=CARTESIAN_POINT('',(25.7,0.500000000000004,-59.4));
#38784=CARTESIAN_POINT('Origin',(-1.54689479616415E-14,13.,-76.7));
#38785=CARTESIAN_POINT('Origin',(-29.3945469326493,4.36391374425416E-15,
-104.175753233145));
#38786=CARTESIAN_POINT('Origin',(-28.5,-3.33849460240199,-64.9));
#38787=CARTESIAN_POINT('Origin',(-28.5,-3.33849460240201,-19.9));
#38788=CARTESIAN_POINT('Origin',(35.,0.500000000000005,-25.4));
#38789=CARTESIAN_POINT('',(25.7,0.499999999999997,-15.1660798485821));
#38790=CARTESIAN_POINT('Origin',(28.5,0.499999999999997,-19.9));
#38791=CARTESIAN_POINT('',(35.,0.500000000000005,-13.4));
#38792=CARTESIAN_POINT('',(35.,0.500000000000007,-104.175753233145));
#38793=CARTESIAN_POINT('',(25.7,0.500000000000004,-13.4));
#38794=CARTESIAN_POINT('',(35.,0.500000000000005,-13.4));
#38795=CARTESIAN_POINT('',(25.7,0.500000000000004,-25.4));
#38796=CARTESIAN_POINT('Origin',(25.7,0.500000000000004,-25.4));
#38797=CARTESIAN_POINT('',(25.7,-13.788236863595,-13.4));
#38798=CARTESIAN_POINT('',(25.7,-13.788236863595,-15.1660798485821));
#38799=CARTESIAN_POINT('',(25.7,-13.788236863595,-104.175753233145));
#38800=CARTESIAN_POINT('',(25.7,24.2065391822594,-15.1660798485821));
#38801=CARTESIAN_POINT('',(25.7,0.500000000000004,-13.4));
#38802=CARTESIAN_POINT('Origin',(-29.3945469326493,4.36391374425416E-15,
-104.175753233145));
#38803=CARTESIAN_POINT('',(-25.7,-13.788236863595,-15.1660798485821));
#38804=CARTESIAN_POINT('Origin',(-28.5,-3.33849460240201,-19.9));
#38805=CARTESIAN_POINT('',(-25.7,-13.788236863595,-13.4));
#38806=CARTESIAN_POINT('',(-29.3945469326493,4.36391374425416E-15,-13.4));
#38807=CARTESIAN_POINT('',(-25.7,-13.788236863595,-104.175753233145));
#38808=CARTESIAN_POINT('Origin',(-25.7,-16.5,-25.4));
#38809=CARTESIAN_POINT('',(-25.7,0.500000000000004,-15.1660798485822));
#38810=CARTESIAN_POINT('',(-25.7,0.500000000000004,-13.4));
#38811=CARTESIAN_POINT('',(-25.7,0.500000000000004,-25.4));
#38812=CARTESIAN_POINT('',(-25.7,24.2065391822594,-15.1660798485822));
#38813=CARTESIAN_POINT('',(-25.7,-16.5,-13.4));
#38814=CARTESIAN_POINT('Origin',(-25.7,0.500000000000004,-25.4));
#38815=CARTESIAN_POINT('',(-34.5,0.500000000000005,-13.4));
#38816=CARTESIAN_POINT('',(-25.7,0.500000000000004,-13.4));
#38817=CARTESIAN_POINT('',(-34.5,0.500000000000005,-104.175753233145));
#38818=CARTESIAN_POINT('Origin',(-28.5,0.500000000000004,-19.9));
#38819=CARTESIAN_POINT('Origin',(29.3945469326493,4.36391374425416E-15,
-104.175753233145));
#38820=CARTESIAN_POINT('',(25.4958861827765,-14.55,-15.2929076226792));
#38821=CARTESIAN_POINT('Origin',(28.5,-3.33849460240214,-19.9));
#38822=CARTESIAN_POINT('',(25.4958861827765,-14.55,-13.4));
#38823=CARTESIAN_POINT('',(29.3945469326493,4.36391374425416E-15,-13.4));
#38824=CARTESIAN_POINT('',(25.4958861827765,-14.55,-104.175753233145));
#38825=CARTESIAN_POINT('Origin',(29.3945469326493,4.36391374425416E-15,
-104.175753233145));
#38826=CARTESIAN_POINT('Origin',(28.5,-3.33849460240214,-64.9));
#38827=CARTESIAN_POINT('Origin',(28.5,-3.33849460240214,-19.9));
#38828=CARTESIAN_POINT('Origin',(12.3307106781187,-16.45,-3.45));
#38829=CARTESIAN_POINT('',(12.3307106781187,-16.45,-3.5));
#38830=CARTESIAN_POINT('',(22.1792893218814,-16.45,-3.5));
#38831=CARTESIAN_POINT('',(12.3307106781187,-16.45,-3.5));
#38832=CARTESIAN_POINT('',(22.1792893218814,-16.45,-3.45));
#38833=CARTESIAN_POINT('',(12.3307106781187,-16.45,-3.45));
#38834=CARTESIAN_POINT('Origin',(22.1792893218814,-16.45,-3.45));
#38835=CARTESIAN_POINT('',(23.15,-15.4792893218813,-3.5));
#38836=CARTESIAN_POINT('',(22.1792893218814,-16.45,-3.5));
#38837=CARTESIAN_POINT('',(23.15,-15.4792893218813,-3.45));
#38838=CARTESIAN_POINT('Origin',(23.15,-15.4792893218813,-3.45));
#38839=CARTESIAN_POINT('',(23.15,11.9792893218814,-3.5));
#38840=CARTESIAN_POINT('',(23.15,-15.4792893218813,-3.5));
#38841=CARTESIAN_POINT('',(23.15,11.9792893218814,-3.45));
#38842=CARTESIAN_POINT('Origin',(23.15,11.9792893218814,-3.45));
#38843=CARTESIAN_POINT('',(22.1792893218813,12.95,-3.5));
#38844=CARTESIAN_POINT('',(23.15,11.9792893218814,-3.5));
#38845=CARTESIAN_POINT('',(22.1792893218813,12.95,-3.45));
#38846=CARTESIAN_POINT('Origin',(22.1792893218813,12.95,-3.45));
#38847=CARTESIAN_POINT('',(-22.1792893218813,12.95,-3.5));
#38848=CARTESIAN_POINT('',(22.1792893218813,12.95,-3.5));
#38849=CARTESIAN_POINT('',(-22.1792893218813,12.95,-3.45));
#38850=CARTESIAN_POINT('Origin',(-22.1792893218813,12.95,-3.45));
#38851=CARTESIAN_POINT('',(-23.15,11.9792893218814,-3.5));
#38852=CARTESIAN_POINT('',(-22.1792893218813,12.95,-3.5));
#38853=CARTESIAN_POINT('',(-23.15,11.9792893218814,-3.45));
#38854=CARTESIAN_POINT('Origin',(-23.15,11.9792893218814,-3.45));
#38855=CARTESIAN_POINT('',(-23.15,-15.4792893218813,-3.5));
#38856=CARTESIAN_POINT('',(-23.15,11.9792893218814,-3.5));
#38857=CARTESIAN_POINT('',(-23.15,-15.4792893218813,-3.45));
#38858=CARTESIAN_POINT('Origin',(-23.15,-15.4792893218813,-3.45));
#38859=CARTESIAN_POINT('',(-22.1792893218814,-16.45,-3.5));
#38860=CARTESIAN_POINT('',(-23.15,-15.4792893218813,-3.5));
#38861=CARTESIAN_POINT('',(-22.1792893218814,-16.45,-3.45));
#38862=CARTESIAN_POINT('Origin',(-22.1792893218814,-16.45,-3.45));
#38863=CARTESIAN_POINT('',(-12.3307106781186,-16.45,-3.5));
#38864=CARTESIAN_POINT('',(-22.1792893218814,-16.45,-3.5));
#38865=CARTESIAN_POINT('',(-12.3307106781186,-16.45,-3.45));
#38866=CARTESIAN_POINT('Origin',(-12.3307106781186,-16.45,-3.45));
#38867=CARTESIAN_POINT('',(-8.23180194846605,-12.3510912703474,-3.5));
#38868=CARTESIAN_POINT('',(-12.3307106781186,-16.45,-3.5));
#38869=CARTESIAN_POINT('',(-8.23180194846605,-12.3510912703474,-3.45));
#38870=CARTESIAN_POINT('Origin',(-8.55,-12.0328932188134,-3.45));
#38871=CARTESIAN_POINT('',(-8.1,-12.0328932188134,-3.5));
#38872=CARTESIAN_POINT('Origin',(-8.55,-12.0328932188134,-3.5));
#38873=CARTESIAN_POINT('',(-8.1,-12.0328932188134,-3.45));
#38874=CARTESIAN_POINT('Origin',(-8.1,-12.0328932188134,-3.45));
#38875=CARTESIAN_POINT('',(-8.1,-8.40710678118654,-3.5));
#38876=CARTESIAN_POINT('',(-8.1,-12.0328932188134,-3.5));
#38877=CARTESIAN_POINT('',(-8.1,-8.40710678118654,-3.45));
#38878=CARTESIAN_POINT('Origin',(-8.55,-8.40710678118654,-3.45));
#38879=CARTESIAN_POINT('',(-8.23180194846605,-8.0889087296526,-3.5));
#38880=CARTESIAN_POINT('Origin',(-8.55,-8.40710678118654,-3.5));
#38881=CARTESIAN_POINT('',(-8.23180194846605,-8.0889087296526,-3.45));
#38882=CARTESIAN_POINT('Origin',(-8.23180194846605,-8.0889087296526,-3.45));
#38883=CARTESIAN_POINT('',(-8.60795233719346,-7.7127583409252,-3.5));
#38884=CARTESIAN_POINT('',(-8.23180194846605,-8.0889087296526,-3.5));
#38885=CARTESIAN_POINT('',(-8.60795233719346,-7.7127583409252,-3.45));
#38886=CARTESIAN_POINT('Origin',(-8.21904360754086,-7.32384961127259,-3.45));
#38887=CARTESIAN_POINT('',(-8.76432075605962,-7.39577200905833,-3.5));
#38888=CARTESIAN_POINT('Origin',(-8.21904360754086,-7.32384961127259,-3.5));
#38889=CARTESIAN_POINT('',(-8.76432075605962,-7.39577200905833,-3.45));
#38890=CARTESIAN_POINT('Origin',(-10.995,-7.69,-3.45));
#38891=CARTESIAN_POINT('',(-10.7007720090583,-5.45932075605962,-3.5));
#38892=CARTESIAN_POINT('Origin',(-10.995,-7.69,-3.5));
#38893=CARTESIAN_POINT('',(-10.7007720090583,-5.45932075605962,-3.45));
#38894=CARTESIAN_POINT('Origin',(-10.6288496112726,-4.91404360754086,-3.45));
#38895=CARTESIAN_POINT('',(-11.0177583409252,-5.30295233719346,-3.5));
#38896=CARTESIAN_POINT('Origin',(-10.6288496112726,-4.91404360754086,-3.5));
#38897=CARTESIAN_POINT('',(-11.0177583409252,-5.30295233719346,-3.45));
#38898=CARTESIAN_POINT('Origin',(-11.0177583409252,-5.30295233719346,-3.45));
#38899=CARTESIAN_POINT('',(-11.3889087296526,-4.93180194846607,-3.5));
#38900=CARTESIAN_POINT('',(-11.0177583409252,-5.30295233719346,-3.5));
#38901=CARTESIAN_POINT('',(-11.3889087296526,-4.93180194846607,-3.45));
#38902=CARTESIAN_POINT('Origin',(-11.,-4.54289321881346,-3.45));
#38903=CARTESIAN_POINT('',(-11.55,-4.54289321881346,-3.5));
#38904=CARTESIAN_POINT('Origin',(-11.,-4.54289321881346,-3.5));
#38905=CARTESIAN_POINT('',(-11.55,-4.54289321881346,-3.45));
#38906=CARTESIAN_POINT('Origin',(-11.55,-4.54289321881346,-3.45));
#38907=CARTESIAN_POINT('',(-11.55,-3.65710678118656,-3.5));
#38908=CARTESIAN_POINT('',(-11.55,-4.54289321881346,-3.5));
#38909=CARTESIAN_POINT('',(-11.55,-3.65710678118656,-3.45));
#38910=CARTESIAN_POINT('Origin',(-11.,-3.65710678118656,-3.45));
#38911=CARTESIAN_POINT('',(-11.3889087296526,-3.26819805153396,-3.5));
#38912=CARTESIAN_POINT('Origin',(-11.,-3.65710678118656,-3.5));
#38913=CARTESIAN_POINT('',(-11.3889087296526,-3.26819805153396,-3.45));
#38914=CARTESIAN_POINT('Origin',(-11.3889087296526,-3.26819805153396,-3.45));
#38915=CARTESIAN_POINT('',(-11.0177583409252,-2.89704766280654,-3.5));
#38916=CARTESIAN_POINT('',(-11.3889087296526,-3.26819805153396,-3.5));
#38917=CARTESIAN_POINT('',(-11.0177583409252,-2.89704766280654,-3.45));
#38918=CARTESIAN_POINT('Origin',(-10.6288496112726,-3.28595639245914,-3.45));
#38919=CARTESIAN_POINT('',(-10.7007720090583,-2.74067924394038,-3.5));
#38920=CARTESIAN_POINT('Origin',(-10.6288496112726,-3.28595639245914,-3.5));
#38921=CARTESIAN_POINT('',(-10.7007720090583,-2.74067924394038,-3.45));
#38922=CARTESIAN_POINT('Origin',(-10.995,-0.510000000000002,-3.45));
#38923=CARTESIAN_POINT('',(-8.76432075605962,-0.804227990941668,-3.5));
#38924=CARTESIAN_POINT('Origin',(-10.995,-0.510000000000002,-3.5));
#38925=CARTESIAN_POINT('',(-8.76432075605962,-0.804227990941668,-3.45));
#38926=CARTESIAN_POINT('Origin',(-8.21904360754086,-0.87615038872741,-3.45));
#38927=CARTESIAN_POINT('',(-8.60795233719346,-0.48724165907481,-3.5));
#38928=CARTESIAN_POINT('Origin',(-8.21904360754086,-0.87615038872741,-3.5));
#38929=CARTESIAN_POINT('',(-8.60795233719346,-0.48724165907481,-3.45));
#38930=CARTESIAN_POINT('Origin',(-8.60795233719346,-0.487241659074809,-3.45));
#38931=CARTESIAN_POINT('',(-8.07071067811865,0.0499999999999998,-3.5));
#38932=CARTESIAN_POINT('',(-8.60795233719346,-0.487241659074809,-3.5));
#38933=CARTESIAN_POINT('',(-8.07071067811865,0.0499999999999998,-3.45));
#38934=CARTESIAN_POINT('Origin',(-8.07071067811865,0.0499999999999998,-3.45));
#38935=CARTESIAN_POINT('',(8.07071067811865,0.0500000000000006,-3.5));
#38936=CARTESIAN_POINT('',(-8.07071067811865,0.0499999999999998,-3.5));
#38937=CARTESIAN_POINT('',(8.07071067811865,0.0500000000000006,-3.45));
#38938=CARTESIAN_POINT('Origin',(8.07071067811865,0.0500000000000006,-3.45));
#38939=CARTESIAN_POINT('',(8.60795233719346,-0.487241659074806,-3.5));
#38940=CARTESIAN_POINT('',(8.07071067811865,0.0500000000000006,-3.5));
#38941=CARTESIAN_POINT('',(8.60795233719346,-0.487241659074806,-3.45));
#38942=CARTESIAN_POINT('Origin',(8.21904360754086,-0.876150388727407,-3.45));
#38943=CARTESIAN_POINT('',(8.76432075605962,-0.804227990941667,-3.5));
#38944=CARTESIAN_POINT('Origin',(8.21904360754086,-0.876150388727407,-3.5));
#38945=CARTESIAN_POINT('',(8.76432075605962,-0.804227990941667,-3.45));
#38946=CARTESIAN_POINT('Origin',(10.995,-0.509999999999999,-3.45));
#38947=CARTESIAN_POINT('',(10.7007720090583,-2.74067924394038,-3.5));
#38948=CARTESIAN_POINT('Origin',(10.995,-0.509999999999999,-3.5));
#38949=CARTESIAN_POINT('',(10.7007720090583,-2.74067924394038,-3.45));
#38950=CARTESIAN_POINT('Origin',(10.6288496112726,-3.28595639245914,-3.45));
#38951=CARTESIAN_POINT('',(11.0177583409252,-2.89704766280654,-3.5));
#38952=CARTESIAN_POINT('Origin',(10.6288496112726,-3.28595639245914,-3.5));
#38953=CARTESIAN_POINT('',(11.0177583409252,-2.89704766280654,-3.45));
#38954=CARTESIAN_POINT('Origin',(11.0177583409252,-2.89704766280654,-3.45));
#38955=CARTESIAN_POINT('',(11.3889087296526,-3.26819805153396,-3.5));
#38956=CARTESIAN_POINT('',(11.0177583409252,-2.89704766280654,-3.5));
#38957=CARTESIAN_POINT('',(11.3889087296526,-3.26819805153396,-3.45));
#38958=CARTESIAN_POINT('Origin',(11.,-3.65710678118656,-3.45));
#38959=CARTESIAN_POINT('',(11.55,-3.65710678118656,-3.5));
#38960=CARTESIAN_POINT('Origin',(11.,-3.65710678118656,-3.5));
#38961=CARTESIAN_POINT('',(11.55,-3.65710678118656,-3.45));
#38962=CARTESIAN_POINT('Origin',(11.55,-3.65710678118656,-3.45));
#38963=CARTESIAN_POINT('',(11.55,-4.54289321881346,-3.5));
#38964=CARTESIAN_POINT('',(11.55,-3.65710678118656,-3.5));
#38965=CARTESIAN_POINT('',(11.55,-4.54289321881346,-3.45));
#38966=CARTESIAN_POINT('Origin',(11.,-4.54289321881346,-3.45));
#38967=CARTESIAN_POINT('',(11.3889087296526,-4.93180194846606,-3.5));
#38968=CARTESIAN_POINT('Origin',(11.,-4.54289321881346,-3.5));
#38969=CARTESIAN_POINT('',(11.3889087296526,-4.93180194846606,-3.45));
#38970=CARTESIAN_POINT('Origin',(11.3889087296526,-4.93180194846606,-3.45));
#38971=CARTESIAN_POINT('',(11.0177583409252,-5.30295233719346,-3.5));
#38972=CARTESIAN_POINT('',(11.3889087296526,-4.93180194846606,-3.5));
#38973=CARTESIAN_POINT('',(11.0177583409252,-5.30295233719346,-3.45));
#38974=CARTESIAN_POINT('Origin',(10.6288496112726,-4.91404360754086,-3.45));
#38975=CARTESIAN_POINT('',(10.7007720090583,-5.45932075605962,-3.5));
#38976=CARTESIAN_POINT('Origin',(10.6288496112726,-4.91404360754086,-3.5));
#38977=CARTESIAN_POINT('',(10.7007720090583,-5.45932075605962,-3.45));
#38978=CARTESIAN_POINT('Origin',(10.995,-7.69,-3.45));
#38979=CARTESIAN_POINT('',(8.76432075605962,-7.39577200905833,-3.5));
#38980=CARTESIAN_POINT('Origin',(10.995,-7.69,-3.5));
#38981=CARTESIAN_POINT('',(8.76432075605962,-7.39577200905833,-3.45));
#38982=CARTESIAN_POINT('Origin',(8.21904360754086,-7.32384961127259,-3.45));
#38983=CARTESIAN_POINT('',(8.60795233719346,-7.71275834092519,-3.5));
#38984=CARTESIAN_POINT('Origin',(8.21904360754086,-7.32384961127259,-3.5));
#38985=CARTESIAN_POINT('',(8.60795233719346,-7.71275834092519,-3.45));
#38986=CARTESIAN_POINT('Origin',(8.60795233719346,-7.71275834092519,-3.45));
#38987=CARTESIAN_POINT('',(8.23180194846606,-8.08890872965259,-3.5));
#38988=CARTESIAN_POINT('',(8.60795233719346,-7.71275834092519,-3.5));
#38989=CARTESIAN_POINT('',(8.23180194846606,-8.08890872965259,-3.45));
#38990=CARTESIAN_POINT('Origin',(8.55,-8.40710678118654,-3.45));
#38991=CARTESIAN_POINT('',(8.1,-8.40710678118654,-3.5));
#38992=CARTESIAN_POINT('Origin',(8.55,-8.40710678118654,-3.5));
#38993=CARTESIAN_POINT('',(8.1,-8.40710678118654,-3.45));
#38994=CARTESIAN_POINT('Origin',(8.1,-8.40710678118654,-3.45));
#38995=CARTESIAN_POINT('',(8.1,-12.0328932188134,-3.5));
#38996=CARTESIAN_POINT('',(8.1,-8.40710678118654,-3.5));
#38997=CARTESIAN_POINT('',(8.1,-12.0328932188134,-3.45));
#38998=CARTESIAN_POINT('Origin',(8.55,-12.0328932188134,-3.45));
#38999=CARTESIAN_POINT('',(8.23180194846605,-12.3510912703474,-3.5));
#39000=CARTESIAN_POINT('Origin',(8.55,-12.0328932188134,-3.5));
#39001=CARTESIAN_POINT('',(8.23180194846605,-12.3510912703474,-3.45));
#39002=CARTESIAN_POINT('Origin',(8.23180194846605,-12.3510912703474,-3.45));
#39003=CARTESIAN_POINT('',(8.23180194846605,-12.3510912703474,-3.5));
#39004=CARTESIAN_POINT('Origin',(-1.64657055886728E-14,13.8,-1.36260717503886E-30));
#39005=CARTESIAN_POINT('',(-4.99999999999999,13.8,-3.5));
#39006=CARTESIAN_POINT('',(5.00000000000001,13.8,-3.5));
#39007=CARTESIAN_POINT('',(-5.8,13.8,-3.5));
#39008=CARTESIAN_POINT('',(5.,13.8,-13.4));
#39009=CARTESIAN_POINT('',(5.,13.8,-13.4));
#39010=CARTESIAN_POINT('',(-4.99999999999999,13.8,-13.4));
#39011=CARTESIAN_POINT('',(-5.8,13.8,-13.4));
#39012=CARTESIAN_POINT('',(-4.99999999999999,13.8,-3.5));
#39013=CARTESIAN_POINT('Origin',(5.00000000000001,13.8,-2.19030741916265E-15));
#39014=CARTESIAN_POINT('',(5.8,13.,-3.5));
#39015=CARTESIAN_POINT('',(5.00000000000001,13.8,-3.5));
#39016=CARTESIAN_POINT('',(5.8,13.,-13.4));
#39017=CARTESIAN_POINT('',(5.8,13.,-13.4));
#39018=CARTESIAN_POINT('',(5.00000000000001,13.8,-13.4));
#39019=CARTESIAN_POINT('Origin',(-22.2,13.,-13.4));
#39020=CARTESIAN_POINT('',(22.2,13.,-3.5));
#39021=CARTESIAN_POINT('',(22.2,13.,-3.5));
#39022=CARTESIAN_POINT('',(22.2,13.,-13.4));
#39023=CARTESIAN_POINT('',(22.2,13.,-13.4));
#39024=CARTESIAN_POINT('',(-22.2,13.,-13.4));
#39025=CARTESIAN_POINT('Origin',(22.2,13.,-13.4));
#39026=CARTESIAN_POINT('',(23.2,12.,-3.5));
#39027=CARTESIAN_POINT('',(23.2,12.,-3.5));
#39028=CARTESIAN_POINT('',(23.2,12.,-13.4));
#39029=CARTESIAN_POINT('',(23.2,12.,-13.4));
#39030=CARTESIAN_POINT('',(22.2,13.,-13.4));
#39031=CARTESIAN_POINT('Origin',(23.2,12.,-13.4));
#39032=CARTESIAN_POINT('',(23.2,-15.5,-3.5));
#39033=CARTESIAN_POINT('',(23.2,-15.5,-3.5));
#39034=CARTESIAN_POINT('',(23.2,-15.5,-13.4));
#39035=CARTESIAN_POINT('',(23.2,-15.5,-13.4));
#39036=CARTESIAN_POINT('',(23.2,12.,-13.4));
#39037=CARTESIAN_POINT('Origin',(-23.2,12.,-13.4));
#39038=CARTESIAN_POINT('',(-23.2,12.,-3.5));
#39039=CARTESIAN_POINT('',(-23.2,-15.5,-3.5));
#39040=CARTESIAN_POINT('',(-23.2,12.,-3.5));
#39041=CARTESIAN_POINT('',(-23.2,12.,-13.4));
#39042=CARTESIAN_POINT('',(-23.2,12.,-13.4));
#39043=CARTESIAN_POINT('',(-23.2,-15.5,-13.4));
#39044=CARTESIAN_POINT('',(-23.2,12.,-13.4));
#39045=CARTESIAN_POINT('',(-23.2,-15.5,-13.4));
#39046=CARTESIAN_POINT('Origin',(-22.2,13.,-13.4));
#39047=CARTESIAN_POINT('',(-22.2,13.,-3.5));
#39048=CARTESIAN_POINT('',(-22.2,13.,-3.5));
#39049=CARTESIAN_POINT('',(-22.2,13.,-13.4));
#39050=CARTESIAN_POINT('',(-22.2,13.,-13.4));
#39051=CARTESIAN_POINT('',(-22.2,13.,-13.4));
#39052=CARTESIAN_POINT('Origin',(-22.2,13.,-13.4));
#39053=CARTESIAN_POINT('',(-5.8,13.,-3.5));
#39054=CARTESIAN_POINT('',(22.2,13.,-3.5));
#39055=CARTESIAN_POINT('',(-5.8,13.,-13.4));
#39056=CARTESIAN_POINT('',(-5.8,13.,-13.4));
#39057=CARTESIAN_POINT('',(-22.2,13.,-13.4));
#39058=CARTESIAN_POINT('Origin',(-4.99999999999999,13.8,-4.38061483832526E-16));
#39059=CARTESIAN_POINT('',(-4.99999999999999,13.8,-13.4));
#39060=CARTESIAN_POINT('',(-4.99999999999999,13.8,-3.5));
#39061=CARTESIAN_POINT('Origin',(35.,13.,-104.175753233145));
#39062=CARTESIAN_POINT('',(35.,13.,-13.4));
#39063=CARTESIAN_POINT('',(35.,13.,-13.4));
#39064=CARTESIAN_POINT('',(35.,0.500000000000005,-71.4));
#39065=CARTESIAN_POINT('',(35.,0.500000000000005,-59.4));
#39066=CARTESIAN_POINT('',(35.,13.,-71.4));
#39067=CARTESIAN_POINT('',(35.,13.,-71.4));
#39068=CARTESIAN_POINT('',(35.,13.,-104.175753233145));
#39069=CARTESIAN_POINT('Origin',(34.,14.,-104.175753233145));
#39070=CARTESIAN_POINT('',(34.,14.,-71.4));
#39071=CARTESIAN_POINT('',(34.,14.,-71.4));
#39072=CARTESIAN_POINT('',(34.,14.,-13.4));
#39073=CARTESIAN_POINT('',(34.,14.,-104.175753233145));
#39074=CARTESIAN_POINT('',(34.,14.,-13.4));
#39075=CARTESIAN_POINT('Origin',(-23.,14.,-84.8));
#39076=CARTESIAN_POINT('',(17.505,14.,-71.4));
#39077=CARTESIAN_POINT('',(17.505,14.,-13.4));
#39078=CARTESIAN_POINT('',(17.505,14.,-83.0807063142603));
#39079=CARTESIAN_POINT('',(23.,14.,-13.4));
#39080=CARTESIAN_POINT('',(23.,14.,-71.4));
#39081=CARTESIAN_POINT('Origin',(17.005,13.5,-83.0807063142603));
#39082=CARTESIAN_POINT('',(17.005,13.5,-71.4));
#39083=CARTESIAN_POINT('',(17.005,13.5,-13.4));
#39084=CARTESIAN_POINT('',(17.005,13.5,-83.0807063142603));
#39085=CARTESIAN_POINT('',(17.005,13.5,-13.4));
#39086=CARTESIAN_POINT('',(17.005,13.5,-71.4));
#39087=CARTESIAN_POINT('Origin',(17.005,13.5,-83.0807063142603));
#39088=CARTESIAN_POINT('',(6.33500000000001,13.5,-71.4));
#39089=CARTESIAN_POINT('',(6.33500000000001,13.5,-13.4));
#39090=CARTESIAN_POINT('',(6.33500000000001,13.5,-83.0807063142603));
#39091=CARTESIAN_POINT('',(17.005,13.5,-13.4));
#39092=CARTESIAN_POINT('',(17.005,13.5,-71.4));
#39093=CARTESIAN_POINT('Origin',(6.33500000000001,13.5,-83.0807063142603));
#39094=CARTESIAN_POINT('',(5.835,14.,-71.4));
#39095=CARTESIAN_POINT('',(5.835,14.,-13.4));
#39096=CARTESIAN_POINT('',(5.835,14.,-83.0807063142603));
#39097=CARTESIAN_POINT('',(6.33500000000001,13.5,-13.4));
#39098=CARTESIAN_POINT('',(6.33500000000001,13.5,-71.4));
#39099=CARTESIAN_POINT('Origin',(-23.,14.,-84.8));
#39100=CARTESIAN_POINT('',(-5.835,14.,-71.4));
#39101=CARTESIAN_POINT('',(23.,14.,-71.4));
#39102=CARTESIAN_POINT('',(-5.835,14.,-13.4));
#39103=CARTESIAN_POINT('',(-5.835,14.,-83.0807063142603));
#39104=CARTESIAN_POINT('',(23.,14.,-13.4));
#39105=CARTESIAN_POINT('Origin',(-6.33500000000001,13.5,-83.0807063142603));
#39106=CARTESIAN_POINT('',(-6.33500000000001,13.5,-71.4));
#39107=CARTESIAN_POINT('',(-6.33500000000001,13.5,-13.4));
#39108=CARTESIAN_POINT('',(-6.33500000000001,13.5,-83.0807063142603));
#39109=CARTESIAN_POINT('',(-6.33500000000001,13.5,-13.4));
#39110=CARTESIAN_POINT('',(-6.33500000000001,13.5,-71.4));
#39111=CARTESIAN_POINT('Origin',(-17.005,13.5,-83.0807063142603));
#39112=CARTESIAN_POINT('',(-17.005,13.5,-71.4));
#39113=CARTESIAN_POINT('',(-17.005,13.5,-13.4));
#39114=CARTESIAN_POINT('',(-17.005,13.5,-83.0807063142603));
#39115=CARTESIAN_POINT('',(-17.005,13.5,-13.4));
#39116=CARTESIAN_POINT('',(-17.005,13.5,-71.4));
#39117=CARTESIAN_POINT('Origin',(-17.005,13.5,-83.0807063142603));
#39118=CARTESIAN_POINT('',(-17.505,14.,-71.4));
#39119=CARTESIAN_POINT('',(-17.505,14.,-13.4));
#39120=CARTESIAN_POINT('',(-17.505,14.,-83.0807063142603));
#39121=CARTESIAN_POINT('',(-17.005,13.5,-13.4));
#39122=CARTESIAN_POINT('',(-17.005,13.5,-71.4));
#39123=CARTESIAN_POINT('Origin',(-23.,14.,-84.8));
#39124=CARTESIAN_POINT('',(-34.,14.,-71.4));
#39125=CARTESIAN_POINT('',(23.,14.,-71.4));
#39126=CARTESIAN_POINT('',(-34.,14.,-13.4));
#39127=CARTESIAN_POINT('',(-34.,14.,-104.175753233145));
#39128=CARTESIAN_POINT('',(23.,14.,-13.4));
#39129=CARTESIAN_POINT('Origin',(-34.,14.,-104.175753233145));
#39130=CARTESIAN_POINT('',(-35.,13.,-71.4));
#39131=CARTESIAN_POINT('',(-34.,14.,-71.4));
#39132=CARTESIAN_POINT('',(-35.,13.,-13.4));
#39133=CARTESIAN_POINT('',(-35.,13.,-104.175753233145));
#39134=CARTESIAN_POINT('',(-34.,14.,-13.4));
#39135=CARTESIAN_POINT('Origin',(-35.,13.,-104.175753233145));
#39136=CARTESIAN_POINT('',(-35.,5.6,-71.4));
#39137=CARTESIAN_POINT('',(-35.,13.,-71.4));
#39138=CARTESIAN_POINT('',(-35.,5.6,-13.4));
#39139=CARTESIAN_POINT('',(-35.,5.6,-104.175753233145));
#39140=CARTESIAN_POINT('',(-35.,13.,-13.4));
#39141=CARTESIAN_POINT('Origin',(-35.,5.6,-104.175753233145));
#39142=CARTESIAN_POINT('',(-34.5,5.10000000000001,-71.4));
#39143=CARTESIAN_POINT('',(-35.,5.6,-71.4));
#39144=CARTESIAN_POINT('',(-34.5,5.10000000000001,-13.4));
#39145=CARTESIAN_POINT('',(-34.5,5.10000000000001,-104.175753233145));
#39146=CARTESIAN_POINT('',(-35.,5.6,-13.4));
#39147=CARTESIAN_POINT('Origin',(-34.5,5.10000000000001,-104.175753233145));
#39148=CARTESIAN_POINT('',(-34.5,0.500000000000005,-71.4));
#39149=CARTESIAN_POINT('',(-34.5,5.10000000000001,-71.4));
#39150=CARTESIAN_POINT('',(-34.5,0.500000000000005,-104.175753233145));
#39151=CARTESIAN_POINT('',(-34.5,5.10000000000001,-13.4));
#39152=CARTESIAN_POINT('Origin',(-35.,0.500000000000005,-59.4));
#39153=CARTESIAN_POINT('',(-25.7,0.500000000000004,-69.6339201514178));
#39154=CARTESIAN_POINT('Origin',(-28.5,0.500000000000004,-64.9));
#39155=CARTESIAN_POINT('',(-25.7,0.500000000000004,-71.4));
#39156=CARTESIAN_POINT('',(-35.,0.500000000000005,-71.4));
#39157=CARTESIAN_POINT('',(-25.7,0.500000000000004,-59.4));
#39158=CARTESIAN_POINT('Origin',(-25.7,0.500000000000004,-59.4));
#39159=CARTESIAN_POINT('',(-25.7,-13.788236863595,-71.4));
#39160=CARTESIAN_POINT('',(-25.7,-13.788236863595,-69.6339201514178));
#39161=CARTESIAN_POINT('',(-25.7,-13.788236863595,-104.175753233145));
#39162=CARTESIAN_POINT('',(-25.7,24.2065391822594,-69.6339201514178));
#39163=CARTESIAN_POINT('',(-25.7,0.500000000000004,-71.4));
#39164=CARTESIAN_POINT('Origin',(-29.3945469326493,4.36391374425416E-15,
-104.175753233145));
#39165=CARTESIAN_POINT('',(-25.4958861827765,-14.55,-69.5070923773207));
#39166=CARTESIAN_POINT('Origin',(-28.5,-3.33849460240199,-64.9));
#39167=CARTESIAN_POINT('',(-25.4958861827765,-14.55,-71.4));
#39168=CARTESIAN_POINT('',(-29.3945469326493,4.36391374425416E-15,-71.4));
#39169=CARTESIAN_POINT('',(-25.4958861827765,-14.55,-104.175753233145));
#39170=CARTESIAN_POINT('Origin',(29.3945469326493,4.36391374425416E-15,
-104.175753233145));
#39171=CARTESIAN_POINT('',(25.7,-13.788236863595,-69.6339201514178));
#39172=CARTESIAN_POINT('Origin',(28.5,-3.33849460240214,-64.9));
#39173=CARTESIAN_POINT('',(25.7,-13.788236863595,-71.4));
#39174=CARTESIAN_POINT('',(29.3945469326493,4.36391374425416E-15,-71.4));
#39175=CARTESIAN_POINT('',(25.7,-13.788236863595,-104.175753233145));
#39176=CARTESIAN_POINT('Origin',(25.7,0.500000000000004,-59.4));
#39177=CARTESIAN_POINT('',(25.7,0.499999999999997,-69.6339201514178));
#39178=CARTESIAN_POINT('',(25.7,0.500000000000004,-71.4));
#39179=CARTESIAN_POINT('',(25.7,0.500000000000004,-59.4));
#39180=CARTESIAN_POINT('',(25.7,24.2065391822594,-69.6339201514178));
#39181=CARTESIAN_POINT('',(25.7,0.500000000000004,-71.4));
#39182=CARTESIAN_POINT('Origin',(35.,0.500000000000005,-59.4));
#39183=CARTESIAN_POINT('',(35.,0.500000000000005,-71.4));
#39184=CARTESIAN_POINT('Origin',(28.5,0.499999999999997,-64.9));
#39185=CARTESIAN_POINT('Origin',(-25.4958861827765,-14.55,-104.175753233145));
#39186=CARTESIAN_POINT('Origin',(-28.5000000000034,-12.2029290542103,-64.8999999999982));
#39187=CARTESIAN_POINT('',(-23.,-16.5,-71.4));
#39188=CARTESIAN_POINT('',(-25.4958861827765,-14.55,-71.4));
#39189=CARTESIAN_POINT('',(-23.,-16.5,-84.8));
#39190=CARTESIAN_POINT('Origin',(-23.2,-15.5,-13.4));
#39191=CARTESIAN_POINT('',(-22.2,-16.5,-3.5));
#39192=CARTESIAN_POINT('',(-23.2,-15.5,-3.5));
#39193=CARTESIAN_POINT('',(-22.2,-16.5,-13.4));
#39194=CARTESIAN_POINT('',(-23.2,-15.5,-13.4));
#39195=CARTESIAN_POINT('',(-22.2,-16.5,-13.4));
#39196=CARTESIAN_POINT('Origin',(23.2,-15.5,-13.4));
#39197=CARTESIAN_POINT('',(22.2,-16.5,-3.5));
#39198=CARTESIAN_POINT('',(22.2,-16.5,-3.5));
#39199=CARTESIAN_POINT('',(22.2,-16.5,-13.4));
#39200=CARTESIAN_POINT('',(22.2,-16.5,-13.4));
#39201=CARTESIAN_POINT('',(23.2,-15.5,-13.4));
#39202=CARTESIAN_POINT('Origin',(0.,0.,-13.4));
#39203=CARTESIAN_POINT('',(-23.,-16.5,-13.4));
#39204=CARTESIAN_POINT('',(23.,-16.5,-13.4));
#39205=CARTESIAN_POINT('',(22.2,-16.5,-13.4));
#39206=CARTESIAN_POINT('',(25.4958861827765,-14.55,-13.4));
#39207=CARTESIAN_POINT('Origin',(25.4958861827765,-14.55,-104.175753233145));
#39208=CARTESIAN_POINT('Origin',(28.5000000000021,-12.2029290542113,-19.9000000000011));
#39209=CARTESIAN_POINT('',(23.,-16.5,-84.8));
#39210=CARTESIAN_POINT('Origin',(-5.8,13.8,-3.5));
#39211=CARTESIAN_POINT('',(-12.31,-16.5,-3.5));
#39212=CARTESIAN_POINT('',(-22.2,-16.5,-3.5));
#39213=CARTESIAN_POINT('',(-8.19644660940672,-12.3864466094067,-3.5));
#39214=CARTESIAN_POINT('',(-12.31,-16.5,-3.5));
#39215=CARTESIAN_POINT('',(-8.05,-12.0328932188134,-3.5));
#39216=CARTESIAN_POINT('Origin',(-8.55,-12.0328932188134,-3.5));
#39217=CARTESIAN_POINT('',(-8.05,-8.40710678118654,-3.5));
#39218=CARTESIAN_POINT('',(-8.05,-12.0328932188134,-3.5));
#39219=CARTESIAN_POINT('',(-8.19644660940673,-8.05355339059327,-3.5));
#39220=CARTESIAN_POINT('Origin',(-8.55,-8.40710678118654,-3.5));
#39221=CARTESIAN_POINT('',(-8.57259699813413,-7.67740300186587,-3.5));
#39222=CARTESIAN_POINT('',(-8.19644660940673,-8.05355339059327,-3.5));
#39223=CARTESIAN_POINT('',(-8.71475010619428,-7.38923360925963,-3.5));
#39224=CARTESIAN_POINT('Origin',(-8.21904360754086,-7.32384961127259,-3.5));
#39225=CARTESIAN_POINT('',(-10.6942336092596,-5.40975010619428,-3.5));
#39226=CARTESIAN_POINT('Origin',(-10.995,-7.69,-3.5));
#39227=CARTESIAN_POINT('',(-10.9824030018659,-5.26759699813413,-3.5));
#39228=CARTESIAN_POINT('Origin',(-10.6288496112726,-4.91404360754086,-3.5));
#39229=CARTESIAN_POINT('',(-11.3535533905933,-4.89644660940674,-3.5));
#39230=CARTESIAN_POINT('',(-10.9824030018659,-5.26759699813413,-3.5));
#39231=CARTESIAN_POINT('',(-11.5,-4.54289321881346,-3.5));
#39232=CARTESIAN_POINT('Origin',(-11.,-4.54289321881346,-3.5));
#39233=CARTESIAN_POINT('',(-11.5,-3.65710678118656,-3.5));
#39234=CARTESIAN_POINT('',(-11.5,-4.54289321881346,-3.5));
#39235=CARTESIAN_POINT('',(-11.3535533905933,-3.30355339059329,-3.5));
#39236=CARTESIAN_POINT('Origin',(-11.,-3.65710678118656,-3.5));
#39237=CARTESIAN_POINT('',(-10.9824030018659,-2.93240300186587,-3.5));
#39238=CARTESIAN_POINT('',(-11.3535533905933,-3.30355339059329,-3.5));
#39239=CARTESIAN_POINT('',(-10.6942336092596,-2.79024989380572,-3.5));
#39240=CARTESIAN_POINT('Origin',(-10.6288496112726,-3.28595639245914,-3.5));
#39241=CARTESIAN_POINT('',(-8.71475010619428,-0.810766390740372,-3.5));
#39242=CARTESIAN_POINT('Origin',(-10.995,-0.510000000000002,-3.5));
#39243=CARTESIAN_POINT('',(-8.57259699813413,-0.522596998134137,-3.5));
#39244=CARTESIAN_POINT('Origin',(-8.21904360754086,-0.87615038872741,-3.5));
#39245=CARTESIAN_POINT('',(-8.05,-1.60428730688303E-15,-3.5));
#39246=CARTESIAN_POINT('',(-8.57259699813413,-0.522596998134137,-3.5));
#39247=CARTESIAN_POINT('',(8.05,3.67394039744206E-16,-3.5));
#39248=CARTESIAN_POINT('',(-8.05,-1.60428730688303E-15,-3.5));
#39249=CARTESIAN_POINT('',(8.57259699813413,-0.522596998134133,-3.5));
#39250=CARTESIAN_POINT('',(8.05,3.67394039744206E-16,-3.5));
#39251=CARTESIAN_POINT('',(8.71475010619428,-0.81076639074037,-3.5));
#39252=CARTESIAN_POINT('Origin',(8.21904360754086,-0.876150388727407,-3.5));
#39253=CARTESIAN_POINT('',(10.6942336092596,-2.79024989380572,-3.5));
#39254=CARTESIAN_POINT('Origin',(10.995,-0.509999999999999,-3.5));
#39255=CARTESIAN_POINT('',(10.9824030018659,-2.93240300186586,-3.5));
#39256=CARTESIAN_POINT('Origin',(10.6288496112726,-3.28595639245914,-3.5));
#39257=CARTESIAN_POINT('',(11.3535533905933,-3.30355339059329,-3.5));
#39258=CARTESIAN_POINT('',(10.9824030018659,-2.93240300186586,-3.5));
#39259=CARTESIAN_POINT('',(11.5,-3.65710678118656,-3.5));
#39260=CARTESIAN_POINT('Origin',(11.,-3.65710678118656,-3.5));
#39261=CARTESIAN_POINT('',(11.5,-4.54289321881346,-3.5));
#39262=CARTESIAN_POINT('',(11.5,-3.65710678118656,-3.5));
#39263=CARTESIAN_POINT('',(11.3535533905933,-4.89644660940673,-3.5));
#39264=CARTESIAN_POINT('Origin',(11.,-4.54289321881346,-3.5));
#39265=CARTESIAN_POINT('',(10.9824030018659,-5.26759699813413,-3.5));
#39266=CARTESIAN_POINT('',(11.3535533905933,-4.89644660940673,-3.5));
#39267=CARTESIAN_POINT('',(10.6942336092596,-5.40975010619428,-3.5));
#39268=CARTESIAN_POINT('Origin',(10.6288496112726,-4.91404360754086,-3.5));
#39269=CARTESIAN_POINT('',(8.71475010619428,-7.38923360925963,-3.5));
#39270=CARTESIAN_POINT('Origin',(10.995,-7.69,-3.5));
#39271=CARTESIAN_POINT('',(8.57259699813413,-7.67740300186587,-3.5));
#39272=CARTESIAN_POINT('Origin',(8.21904360754086,-7.32384961127259,-3.5));
#39273=CARTESIAN_POINT('',(8.19644660940673,-8.05355339059327,-3.5));
#39274=CARTESIAN_POINT('',(8.57259699813413,-7.67740300186587,-3.5));
#39275=CARTESIAN_POINT('',(8.05,-8.40710678118654,-3.5));
#39276=CARTESIAN_POINT('Origin',(8.55,-8.40710678118654,-3.5));
#39277=CARTESIAN_POINT('',(8.05,-12.0328932188134,-3.5));
#39278=CARTESIAN_POINT('',(8.05,-8.40710678118654,-3.5));
#39279=CARTESIAN_POINT('',(8.19644660940673,-12.3864466094067,-3.5));
#39280=CARTESIAN_POINT('Origin',(8.55,-12.0328932188134,-3.5));
#39281=CARTESIAN_POINT('',(12.31,-16.5,-3.5));
#39282=CARTESIAN_POINT('',(8.19644660940673,-12.3864466094067,-3.5));
#39283=CARTESIAN_POINT('',(12.31,-16.5,-3.5));
#39284=CARTESIAN_POINT('Origin',(0.,0.,-71.4));
#39285=CARTESIAN_POINT('',(22.2,-16.5,-71.4));
#39286=CARTESIAN_POINT('',(22.2,-16.5,-71.4));
#39287=CARTESIAN_POINT('',(23.2,-15.5,-71.4));
#39288=CARTESIAN_POINT('',(23.2,-15.5,-71.4));
#39289=CARTESIAN_POINT('',(23.2,12.,-71.4));
#39290=CARTESIAN_POINT('',(23.2,12.,-71.4));
#39291=CARTESIAN_POINT('',(22.2,13.,-71.4));
#39292=CARTESIAN_POINT('',(22.2,13.,-71.4));
#39293=CARTESIAN_POINT('',(5.79999999999999,13.,-71.4));
#39294=CARTESIAN_POINT('',(-22.2,13.,-71.4));
#39295=CARTESIAN_POINT('',(4.99999999999997,13.8,-71.4));
#39296=CARTESIAN_POINT('',(4.99999999999996,13.8,-71.4));
#39297=CARTESIAN_POINT('',(-4.99999999999998,13.8,-71.4));
#39298=CARTESIAN_POINT('',(-5.79999999999999,13.8,-71.4));
#39299=CARTESIAN_POINT('',(-5.79999999999999,13.,-71.4));
#39300=CARTESIAN_POINT('',(-4.99999999999997,13.8,-71.4));
#39301=CARTESIAN_POINT('',(-22.2,13.,-71.4));
#39302=CARTESIAN_POINT('',(-22.2,13.,-71.4));
#39303=CARTESIAN_POINT('',(-23.2,12.,-71.4));
#39304=CARTESIAN_POINT('',(-23.2,12.,-71.4));
#39305=CARTESIAN_POINT('',(-23.2,-15.5,-71.4));
#39306=CARTESIAN_POINT('',(-23.2,-15.5,-71.4));
#39307=CARTESIAN_POINT('',(-22.2,-16.5,-71.4));
#39308=CARTESIAN_POINT('',(-22.2,-16.5,-71.4));
#39309=CARTESIAN_POINT('',(-23.,-16.5,-71.4));
#39310=CARTESIAN_POINT('Origin',(-4.99999999999996,13.8,1.31418445149757E-15));
#39311=CARTESIAN_POINT('',(-5.79999999999999,13.,-81.3));
#39312=CARTESIAN_POINT('',(-4.99999999999999,13.8,-81.3));
#39313=CARTESIAN_POINT('',(-4.99999999999997,13.8,-81.3));
#39314=CARTESIAN_POINT('',(-5.8,13.,-81.3));
#39315=CARTESIAN_POINT('',(-4.99999999999998,13.8,-71.4));
#39316=CARTESIAN_POINT('Origin',(22.2,13.,-84.8));
#39317=CARTESIAN_POINT('',(23.2,12.,-81.3));
#39318=CARTESIAN_POINT('',(22.2,13.,-81.3));
#39319=CARTESIAN_POINT('',(23.2,12.,-81.3));
#39320=CARTESIAN_POINT('',(22.2,13.,-84.8));
#39321=CARTESIAN_POINT('',(23.2,12.,-84.8));
#39322=CARTESIAN_POINT('Origin',(23.2,12.,-84.8));
#39323=CARTESIAN_POINT('',(23.2,-15.5,-81.3));
#39324=CARTESIAN_POINT('',(23.2,-15.5,-81.3));
#39325=CARTESIAN_POINT('',(23.2,-15.5,-84.8));
#39326=CARTESIAN_POINT('Origin',(23.2,-15.5,-84.8));
#39327=CARTESIAN_POINT('',(22.2,-16.5,-81.3));
#39328=CARTESIAN_POINT('',(22.2,-16.5,-81.3));
#39329=CARTESIAN_POINT('',(22.2,-16.5,-84.8));
#39330=CARTESIAN_POINT('Origin',(-22.2,13.,-84.8));
#39331=CARTESIAN_POINT('',(5.8,13.,-81.3));
#39332=CARTESIAN_POINT('',(22.2,13.,-81.3));
#39333=CARTESIAN_POINT('',(5.8,13.,-81.3));
#39334=CARTESIAN_POINT('Origin',(8.55,-12.0328932188134,-84.8));
#39335=CARTESIAN_POINT('',(8.05,-12.0328932188134,-81.3));
#39336=CARTESIAN_POINT('',(8.05,-12.0328932188134,-84.8));
#39337=CARTESIAN_POINT('',(8.19644660940673,-12.3864466094067,-81.3));
#39338=CARTESIAN_POINT('Origin',(8.55,-12.0328932188134,-81.3));
#39339=CARTESIAN_POINT('',(8.19644660940673,-12.3864466094067,-84.8));
#39340=CARTESIAN_POINT('Origin',(8.55,-8.40710678118654,-84.8));
#39341=CARTESIAN_POINT('',(8.19644660940673,-8.05355339059327,-81.3));
#39342=CARTESIAN_POINT('',(8.19644660940673,-8.05355339059327,-84.8));
#39343=CARTESIAN_POINT('',(8.05,-8.40710678118654,-81.3));
#39344=CARTESIAN_POINT('Origin',(8.55,-8.40710678118654,-81.3));
#39345=CARTESIAN_POINT('',(8.05,-8.40710678118654,-84.8));
#39346=CARTESIAN_POINT('Origin',(8.05,-12.24,-84.8));
#39347=CARTESIAN_POINT('',(8.05,-8.40710678118654,-81.3));
#39348=CARTESIAN_POINT('Origin',(12.31,-16.5,-84.8));
#39349=CARTESIAN_POINT('',(12.31,-16.5,-81.3));
#39350=CARTESIAN_POINT('',(8.19644660940673,-12.3864466094067,-81.3));
#39351=CARTESIAN_POINT('',(12.31,-16.5,-84.8));
#39352=CARTESIAN_POINT('Origin',(12.31,-16.5,-84.8));
#39353=CARTESIAN_POINT('',(12.31,-16.5,-81.3));
#39354=CARTESIAN_POINT('Origin',(8.21904360754086,-7.32384961127259,-84.8));
#39355=CARTESIAN_POINT('',(8.71475010619428,-7.38923360925963,-81.3));
#39356=CARTESIAN_POINT('',(8.57259699813413,-7.67740300186587,-81.3));
#39357=CARTESIAN_POINT('Origin',(8.21904360754086,-7.32384961127259,-81.3));
#39358=CARTESIAN_POINT('',(8.57259699813413,-7.67740300186587,-84.8));
#39359=CARTESIAN_POINT('',(8.71475010619428,-7.38923360925963,-84.8));
#39360=CARTESIAN_POINT('Origin',(10.6288496112726,-4.91404360754086,-84.8));
#39361=CARTESIAN_POINT('',(10.9824030018659,-5.26759699813413,-81.3));
#39362=CARTESIAN_POINT('',(10.6942336092596,-5.40975010619428,-81.3));
#39363=CARTESIAN_POINT('Origin',(10.6288496112726,-4.91404360754086,-81.3));
#39364=CARTESIAN_POINT('',(10.6942336092596,-5.40975010619428,-84.8));
#39365=CARTESIAN_POINT('',(10.9824030018659,-5.26759699813413,0.));
#39366=CARTESIAN_POINT('Origin',(10.995,-7.69,-84.8));
#39367=CARTESIAN_POINT('Origin',(10.995,-7.69,-81.3));
#39368=CARTESIAN_POINT('Origin',(11.,-4.54289321881346,-84.8));
#39369=CARTESIAN_POINT('',(11.5,-4.54289321881346,-81.3));
#39370=CARTESIAN_POINT('',(11.3535533905933,-4.89644660940673,-81.3));
#39371=CARTESIAN_POINT('Origin',(11.,-4.54289321881346,-81.3));
#39372=CARTESIAN_POINT('',(11.3535533905933,-4.89644660940673,-84.8));
#39373=CARTESIAN_POINT('',(11.5,-4.54289321881346,0.));
#39374=CARTESIAN_POINT('Origin',(11.,-3.65710678118656,-84.8));
#39375=CARTESIAN_POINT('',(11.3535533905933,-3.30355339059329,-81.3));
#39376=CARTESIAN_POINT('',(11.5,-3.65710678118656,-81.3));
#39377=CARTESIAN_POINT('Origin',(11.,-3.65710678118656,-81.3));
#39378=CARTESIAN_POINT('',(11.5,-3.65710678118656,-84.8));
#39379=CARTESIAN_POINT('',(11.3535533905933,-3.30355339059329,0.));
#39380=CARTESIAN_POINT('Origin',(11.5,-4.75000000000001,-84.8));
#39381=CARTESIAN_POINT('',(11.5,-3.65710678118656,-81.3));
#39382=CARTESIAN_POINT('Origin',(8.05,-8.2,-84.8));
#39383=CARTESIAN_POINT('',(11.3535533905933,-4.89644660940673,-81.3));
#39384=CARTESIAN_POINT('Origin',(10.6288496112726,-3.28595639245914,-84.8));
#39385=CARTESIAN_POINT('',(10.6942336092596,-2.79024989380572,-81.3));
#39386=CARTESIAN_POINT('',(10.9824030018659,-2.93240300186586,-81.3));
#39387=CARTESIAN_POINT('Origin',(10.6288496112726,-3.28595639245914,-81.3));
#39388=CARTESIAN_POINT('',(10.9824030018659,-2.93240300186586,-84.8));
#39389=CARTESIAN_POINT('',(10.6942336092596,-2.79024989380572,-84.8));
#39390=CARTESIAN_POINT('Origin',(8.21904360754086,-0.876150388727407,-84.8));
#39391=CARTESIAN_POINT('',(8.57259699813413,-0.522596998134133,-81.3));
#39392=CARTESIAN_POINT('',(8.71475010619428,-0.81076639074037,-81.3));
#39393=CARTESIAN_POINT('Origin',(8.21904360754086,-0.876150388727407,-81.3));
#39394=CARTESIAN_POINT('',(8.71475010619428,-0.81076639074037,-84.8));
#39395=CARTESIAN_POINT('',(8.57259699813413,-0.522596998134133,0.));
#39396=CARTESIAN_POINT('Origin',(10.995,-0.509999999999999,-84.8));
#39397=CARTESIAN_POINT('Origin',(10.995,-0.509999999999999,-81.3));
#39398=CARTESIAN_POINT('Origin',(8.05,3.67394039744206E-16,-84.8));
#39399=CARTESIAN_POINT('',(-8.05,-1.60428730688303E-15,-81.3));
#39400=CARTESIAN_POINT('',(-8.05,-1.60428730688303E-15,-84.8));
#39401=CARTESIAN_POINT('',(8.05,3.67394039744206E-16,-81.3));
#39402=CARTESIAN_POINT('',(-8.05,-1.60428730688303E-15,-81.3));
#39403=CARTESIAN_POINT('',(8.05,3.67394039744206E-16,-84.8));
#39404=CARTESIAN_POINT('Origin',(8.05,3.67394039744206E-16,-84.8));
#39405=CARTESIAN_POINT('',(8.05,3.67394039744206E-16,-81.3));
#39406=CARTESIAN_POINT('Origin',(-8.21904360754086,-0.87615038872741,-84.8));
#39407=CARTESIAN_POINT('',(-8.71475010619428,-0.810766390740372,-81.3));
#39408=CARTESIAN_POINT('',(-8.57259699813413,-0.522596998134137,-81.3));
#39409=CARTESIAN_POINT('Origin',(-8.21904360754086,-0.87615038872741,-81.3));
#39410=CARTESIAN_POINT('',(-8.57259699813413,-0.522596998134137,-84.8));
#39411=CARTESIAN_POINT('',(-8.71475010619428,-0.810766390740372,-84.8));
#39412=CARTESIAN_POINT('Origin',(-10.6288496112726,-3.28595639245914,-84.8));
#39413=CARTESIAN_POINT('',(-10.9824030018659,-2.93240300186587,-81.3));
#39414=CARTESIAN_POINT('',(-10.6942336092596,-2.79024989380572,-81.3));
#39415=CARTESIAN_POINT('Origin',(-10.6288496112726,-3.28595639245914,-81.3));
#39416=CARTESIAN_POINT('',(-10.6942336092596,-2.79024989380572,-84.8));
#39417=CARTESIAN_POINT('',(-10.9824030018659,-2.93240300186587,0.));
#39418=CARTESIAN_POINT('Origin',(-10.995,-0.510000000000002,-84.8));
#39419=CARTESIAN_POINT('Origin',(-10.995,-0.510000000000002,-81.3));
#39420=CARTESIAN_POINT('Origin',(-11.,-3.65710678118656,-84.8));
#39421=CARTESIAN_POINT('',(-11.5,-3.65710678118656,-81.3));
#39422=CARTESIAN_POINT('',(-11.3535533905933,-3.30355339059329,-81.3));
#39423=CARTESIAN_POINT('Origin',(-11.,-3.65710678118656,-81.3));
#39424=CARTESIAN_POINT('',(-11.3535533905933,-3.30355339059329,-84.8));
#39425=CARTESIAN_POINT('',(-11.5,-3.65710678118656,0.));
#39426=CARTESIAN_POINT('Origin',(-11.,-4.54289321881346,-84.8));
#39427=CARTESIAN_POINT('',(-11.3535533905933,-4.89644660940674,-81.3));
#39428=CARTESIAN_POINT('',(-11.5,-4.54289321881346,-81.3));
#39429=CARTESIAN_POINT('Origin',(-11.,-4.54289321881346,-81.3));
#39430=CARTESIAN_POINT('',(-11.5,-4.54289321881346,-84.8));
#39431=CARTESIAN_POINT('',(-11.3535533905933,-4.89644660940674,0.));
#39432=CARTESIAN_POINT('Origin',(-11.5,-4.75000000000001,-84.8));
#39433=CARTESIAN_POINT('',(-11.5,-4.54289321881346,-81.3));
#39434=CARTESIAN_POINT('Origin',(-8.05,-1.60428730688303E-15,-84.8));
#39435=CARTESIAN_POINT('',(-11.3535533905933,-3.30355339059329,-81.3));
#39436=CARTESIAN_POINT('Origin',(-8.05,-1.60428730688303E-15,-84.8));
#39437=CARTESIAN_POINT('',(-8.57259699813413,-0.522596998134137,-81.3));
#39438=CARTESIAN_POINT('Origin',(-10.6288496112726,-4.91404360754086,-84.8));
#39439=CARTESIAN_POINT('',(-10.6942336092596,-5.40975010619428,-81.3));
#39440=CARTESIAN_POINT('',(-10.9824030018659,-5.26759699813413,-81.3));
#39441=CARTESIAN_POINT('Origin',(-10.6288496112726,-4.91404360754086,-81.3));
#39442=CARTESIAN_POINT('',(-10.9824030018659,-5.26759699813413,-84.8));
#39443=CARTESIAN_POINT('',(-10.6942336092596,-5.40975010619428,-84.8));
#39444=CARTESIAN_POINT('Origin',(-8.21904360754086,-7.32384961127259,-84.8));
#39445=CARTESIAN_POINT('',(-8.57259699813413,-7.67740300186587,-81.3));
#39446=CARTESIAN_POINT('',(-8.71475010619428,-7.38923360925963,-81.3));
#39447=CARTESIAN_POINT('Origin',(-8.21904360754086,-7.32384961127259,-81.3));
#39448=CARTESIAN_POINT('',(-8.71475010619428,-7.38923360925963,-84.8));
#39449=CARTESIAN_POINT('',(-8.57259699813413,-7.67740300186587,0.));
#39450=CARTESIAN_POINT('Origin',(-10.995,-7.69,-84.8));
#39451=CARTESIAN_POINT('Origin',(-10.995,-7.69,-81.3));
#39452=CARTESIAN_POINT('Origin',(-8.55,-8.40710678118654,-84.8));
#39453=CARTESIAN_POINT('',(-8.05,-8.40710678118654,-81.3));
#39454=CARTESIAN_POINT('',(-8.05,-8.40710678118654,-84.8));
#39455=CARTESIAN_POINT('',(-8.19644660940673,-8.05355339059327,-81.3));
#39456=CARTESIAN_POINT('Origin',(-8.55,-8.40710678118654,-81.3));
#39457=CARTESIAN_POINT('',(-8.19644660940673,-8.05355339059327,-84.8));
#39458=CARTESIAN_POINT('Origin',(-8.55,-12.0328932188134,-84.8));
#39459=CARTESIAN_POINT('',(-8.19644660940672,-12.3864466094067,-81.3));
#39460=CARTESIAN_POINT('',(-8.19644660940672,-12.3864466094067,-84.8));
#39461=CARTESIAN_POINT('',(-8.05,-12.0328932188134,-81.3));
#39462=CARTESIAN_POINT('Origin',(-8.55,-12.0328932188134,-81.3));
#39463=CARTESIAN_POINT('',(-8.05,-12.0328932188134,-84.8));
#39464=CARTESIAN_POINT('Origin',(-22.2,-16.5,-84.8));
#39465=CARTESIAN_POINT('',(-23.2,-15.5,-81.3));
#39466=CARTESIAN_POINT('',(-22.2,-16.5,-81.3));
#39467=CARTESIAN_POINT('',(-23.2,-15.5,-81.3));
#39468=CARTESIAN_POINT('',(-22.2,-16.5,-84.8));
#39469=CARTESIAN_POINT('',(-23.2,-15.5,-84.8));
#39470=CARTESIAN_POINT('Origin',(-23.2,-15.5,-84.8));
#39471=CARTESIAN_POINT('',(-23.2,12.,-81.3));
#39472=CARTESIAN_POINT('',(-23.2,12.,-81.3));
#39473=CARTESIAN_POINT('',(-23.2,12.,-84.8));
#39474=CARTESIAN_POINT('Origin',(-23.2,12.,-84.8));
#39475=CARTESIAN_POINT('',(-22.2,13.,-81.3));
#39476=CARTESIAN_POINT('',(-22.2,13.,-81.3));
#39477=CARTESIAN_POINT('',(-22.2,13.,-84.8));
#39478=CARTESIAN_POINT('Origin',(-22.2,13.,-84.8));
#39479=CARTESIAN_POINT('',(22.2,13.,-81.3));
#39480=CARTESIAN_POINT('Origin',(-23.,-16.5,-84.8));
#39481=CARTESIAN_POINT('',(-12.31,-16.5,-81.3));
#39482=CARTESIAN_POINT('',(-22.2,-16.5,-81.3));
#39483=CARTESIAN_POINT('',(-12.31,-16.5,-84.8));
#39484=CARTESIAN_POINT('Origin',(-12.31,-16.5,-84.8));
#39485=CARTESIAN_POINT('',(-12.31,-16.5,-81.3));
#39486=CARTESIAN_POINT('Origin',(-8.05,-12.24,-84.8));
#39487=CARTESIAN_POINT('',(-8.05,-12.0328932188134,-81.3));
#39488=CARTESIAN_POINT('Origin',(-8.05,-8.2,-84.8));
#39489=CARTESIAN_POINT('',(-8.19644660940673,-8.05355339059327,-81.3));
#39490=CARTESIAN_POINT('Origin',(-8.05,-8.2,-84.8));
#39491=CARTESIAN_POINT('',(-10.9824030018659,-5.26759699813413,-81.3));
#39492=CARTESIAN_POINT('Origin',(8.05,3.67394039744206E-16,-84.8));
#39493=CARTESIAN_POINT('',(10.9824030018659,-2.93240300186586,-81.3));
#39494=CARTESIAN_POINT('Origin',(8.05,-8.2,-84.8));
#39495=CARTESIAN_POINT('',(8.57259699813413,-7.67740300186587,-81.3));
#39496=CARTESIAN_POINT('Origin',(4.99999999999995,13.8,1.31418445149758E-15));
#39497=CARTESIAN_POINT('',(4.99999999999997,13.8,-81.3));
#39498=CARTESIAN_POINT('',(4.99999999999996,13.8,-81.3));
#39499=CARTESIAN_POINT('',(4.99999999999997,13.8,-81.3));
#39500=CARTESIAN_POINT('Origin',(-1.64657055886728E-14,13.8,4.08782152511659E-30));
#39501=CARTESIAN_POINT('',(-5.8,13.8,-81.3));
#39502=CARTESIAN_POINT('Origin',(-5.8,13.8,-81.3));
#39503=CARTESIAN_POINT('Origin',(4.99995,13.,-1.));
#39504=CARTESIAN_POINT('',(4.99995,8.,-1.));
#39505=CARTESIAN_POINT('',(4.99995,13.,-1.));
#39506=CARTESIAN_POINT('',(4.99995,8.,-1.));
#39507=CARTESIAN_POINT('Origin',(0.,8.,-1.));
#39508=CARTESIAN_POINT('',(-4.99995,8.,-1.));
#39509=CARTESIAN_POINT('Origin',(0.,8.,-1.));
#39510=CARTESIAN_POINT('',(-4.99995,8.,-1.));
#39511=CARTESIAN_POINT('Origin',(-4.99995,13.,-1.));
#39512=CARTESIAN_POINT('',(-4.99995,13.,-1.));
#39513=CARTESIAN_POINT('Origin',(0.,8.,-1.));
#39514=CARTESIAN_POINT('Origin',(-28.5,24.2065391822594,-19.9));
#39515=CARTESIAN_POINT('Origin',(-28.5,24.2065391822594,-64.9));
#39516=CARTESIAN_POINT('Origin',(28.5,24.2065391822594,-19.9));
#39517=CARTESIAN_POINT('Origin',(28.5,24.2065391822594,-64.9));
#39518=CARTESIAN_POINT('',(0.,0.,0.));
#39519=CARTESIAN_POINT('Origin',(-1.30104260698261E-15,5.62313017679403,
-9.43017678221748));
#39520=CARTESIAN_POINT('',(-9.42566476249075E-16,6.10854241414471,-5.90647463868609));
#39521=CARTESIAN_POINT('Origin',(-1.30104260698261E-15,4.79163859753386,
-9.0857616930889));
#39522=CARTESIAN_POINT('',(-1.65091236461116E-15,7.42947410803995,-6.70023456114395));
#39523=CARTESIAN_POINT('Origin',(-1.82151749662023E-15,7.24953476434565,
-5.50368876904451));
#39524=CARTESIAN_POINT('Origin',(-1.1944312217556E-15,6.1997608355023,-9.66902502153458));
#39525=CARTESIAN_POINT('Ctrl Pts',(-1.0334492107102E-15,9.1104629285565,
-7.23378761718564));
#39526=CARTESIAN_POINT('Ctrl Pts',(-3.36374346224613,9.1104629285565,-7.23378761718564));
#39527=CARTESIAN_POINT('Ctrl Pts',(-3.36374346224613,7.82321403482853,-10.3414813545735));
#39528=CARTESIAN_POINT('Ctrl Pts',(-3.36374346224613,6.53596514110056,-13.4491750919613));
#39529=CARTESIAN_POINT('Ctrl Pts',(-1.0334492107102E-15,6.53596514110056,
-13.4491750919613));
#39530=CARTESIAN_POINT('Ctrl Pts',(3.36374346224612,6.53596514110056,-13.4491750919613));
#39531=CARTESIAN_POINT('Ctrl Pts',(3.36374346224612,7.82321403482853,-10.3414813545735));
#39532=CARTESIAN_POINT('Ctrl Pts',(3.36374346224612,9.1104629285565,-7.23378761718564));
#39533=CARTESIAN_POINT('Ctrl Pts',(-1.0334492107102E-15,9.1104629285565,
-7.23378761718564));
#39534=CARTESIAN_POINT('Ctrl Pts',(-1.09748950322703E-15,8.40101827381132,
-6.55413148618164));
#39535=CARTESIAN_POINT('Ctrl Pts',(-3.72017113527558,8.40101827381132,-6.55413148618164));
#39536=CARTESIAN_POINT('Ctrl Pts',(-3.72017113527558,6.97737041477854,-9.99112145550203));
#39537=CARTESIAN_POINT('Ctrl Pts',(-3.72017113527558,5.55372255574576,-13.4281114248224));
#39538=CARTESIAN_POINT('Ctrl Pts',(-1.09748950322703E-15,5.55372255574576,
-13.4281114248224));
#39539=CARTESIAN_POINT('Ctrl Pts',(3.72017113527558,5.55372255574576,-13.4281114248224));
#39540=CARTESIAN_POINT('Ctrl Pts',(3.72017113527558,6.97737041477854,-9.99112145550203));
#39541=CARTESIAN_POINT('Ctrl Pts',(3.72017113527558,8.40101827381132,-6.55413148618164));
#39542=CARTESIAN_POINT('Ctrl Pts',(-1.09748950322703E-15,8.40101827381132,
-6.55413148618164));
#39543=CARTESIAN_POINT('Ctrl Pts',(-1.15636367776747E-15,7.42947410803995,
-6.70023456114395));
#39544=CARTESIAN_POINT('Ctrl Pts',(-3.21339563862928,7.42947410803995,-6.70023456114395));
#39545=CARTESIAN_POINT('Ctrl Pts',(-3.21339563862928,6.1997608355023,-9.66902502153458));
#39546=CARTESIAN_POINT('Ctrl Pts',(-3.21339563862928,4.97004756296464,-12.6378154819252));
#39547=CARTESIAN_POINT('Ctrl Pts',(-1.15636367776747E-15,4.97004756296464,
-12.6378154819252));
#39548=CARTESIAN_POINT('Ctrl Pts',(3.21339563862928,4.97004756296464,-12.6378154819252));
#39549=CARTESIAN_POINT('Ctrl Pts',(3.21339563862928,6.1997608355023,-9.66902502153458));
#39550=CARTESIAN_POINT('Ctrl Pts',(3.21339563862928,7.42947410803995,-6.70023456114395));
#39551=CARTESIAN_POINT('Ctrl Pts',(-1.15636367776747E-15,7.42947410803995,
-6.70023456114395));
#39552=CARTESIAN_POINT('',(-1.44538897712945E-15,9.1104629285565,-7.23378761718564));
#39553=CARTESIAN_POINT('Origin',(-1.26789919235761E-15,7.72689451084046,
-8.67799620097772));
#39554=CARTESIAN_POINT('Origin',(-1.07151675469833E-15,7.82321403482853,
-10.3414813545735));
#39555=CARTESIAN_POINT('Origin',(-9.16325707068394E-16,9.87297602634596,
-11.1905205710969));
#39556=CARTESIAN_POINT('',(-1.22248740685523E-15,10.8296846072587,-8.88082173981866));
#39557=CARTESIAN_POINT('',(-1.22248740685523E-15,10.8296846072587,-8.88082173981866));
#39558=CARTESIAN_POINT('Origin',(-9.16325707068394E-16,9.87297602634596,
-11.1905205710969));
#39559=CARTESIAN_POINT('Origin',(-8.67361737988404E-16,9.41103626009031,
-10.9991788549143));
#39560=CARTESIAN_POINT('',(0.944722181384557,9.66424685661039,-11.6944373635354));
#39561=CARTESIAN_POINT('Origin',(-9.16325707068394E-16,9.87297602634596,
-11.1905205710969));
#39562=CARTESIAN_POINT('Origin',(0.,4.50578927537974,-8.96735902705751));
#39563=CARTESIAN_POINT('',(-1.73205080756888,3.64358830043861,-11.8574002906228));
#39564=CARTESIAN_POINT('',(1.73205080756888,3.64358830043861,-11.8574002906228));
#39565=CARTESIAN_POINT('Origin',(0.,4.79163859753386,-9.08576169308891));
#39566=CARTESIAN_POINT('',(-8.67361737988404E-16,2.97505554591939,-12.6628771571027));
#39567=CARTESIAN_POINT('Ctrl Pts',(-8.83559534733916E-12,2.97505554591472,
-12.6628771571063));
#39568=CARTESIAN_POINT('Ctrl Pts',(0.928203230271955,3.46598430139072,-12.2861742738559));
#39569=CARTESIAN_POINT('Ctrl Pts',(1.73205080756887,3.6435883004386,-11.8574002906228));
#39570=CARTESIAN_POINT('Ctrl Pts',(-1.73205080756888,3.64358830043861,-11.8574002906228));
#39571=CARTESIAN_POINT('Ctrl Pts',(-0.928203230271849,3.46598430139071,
-12.2861742738559));
#39572=CARTESIAN_POINT('Ctrl Pts',(9.11080614203771E-12,2.97505554591457,
-12.6628771571064));
#39573=CARTESIAN_POINT('Origin',(0.,2.94387953251129,-8.32039482835873));
#39574=CARTESIAN_POINT('',(-1.73205080756888,4.09192982960656,-5.54875623082487));
#39575=CARTESIAN_POINT('',(1.73205080756888,4.09192982960656,-5.54875623082487));
#39576=CARTESIAN_POINT('Origin',(0.,2.94387953251129,-8.32039482835873));
#39577=CARTESIAN_POINT('',(6.50521303491303E-15,4.76046258412578,-4.74327936434497));
#39578=CARTESIAN_POINT('Ctrl Pts',(-8.84140945978337E-12,4.76046258413045,
-4.74327936434139));
#39579=CARTESIAN_POINT('Ctrl Pts',(0.928203230271958,4.26953382865444,-5.11998224759177));
#39580=CARTESIAN_POINT('Ctrl Pts',(1.73205080756888,4.09192982960656,-5.54875623082487));
#39581=CARTESIAN_POINT('Ctrl Pts',(-1.73205080756888,4.09192982960655,-5.54875623082487));
#39582=CARTESIAN_POINT('Ctrl Pts',(-0.928203230271845,4.26953382865446,
-5.11998224759171));
#39583=CARTESIAN_POINT('Ctrl Pts',(9.11907870314464E-12,4.7604625841306,
-4.74327936434127));
#39584=CARTESIAN_POINT('Origin',(0.,0.,-7.101));
#39585=CARTESIAN_POINT('',(-2.79266716119615,2.86374058300968,-7.101));
#39586=CARTESIAN_POINT('',(2.79266716119615,2.86374058300968,-7.101));
#39587=CARTESIAN_POINT('Origin',(0.,2.44435548440748,-8.11348519290263));
#39588=CARTESIAN_POINT('',(-4.61252776028392E-16,4.,-5.51067764861519));
#39589=CARTESIAN_POINT('Ctrl Pts',(-2.79266716119614,2.86374058300969,-7.10099999999999));
#39590=CARTESIAN_POINT('Ctrl Pts',(-2.791487395233,2.86489106908469,-7.0982224809144));
#39591=CARTESIAN_POINT('Ctrl Pts',(-2.79030270745925,2.86604495955758,-7.09544824938184));
#39592=CARTESIAN_POINT('Ctrl Pts',(-2.64444489381139,3.00792702197672,-6.75569806071638));
#39593=CARTESIAN_POINT('Ctrl Pts',(-2.42146694806281,3.19843151589414,-6.46722664985982));
#39594=CARTESIAN_POINT('Ctrl Pts',(-1.897815678339,3.53535819041829,-6.01625804314877));
#39595=CARTESIAN_POINT('Ctrl Pts',(-1.5580225174343,3.70511768616704,-5.82557882438308));
#39596=CARTESIAN_POINT('Ctrl Pts',(-0.804950314595278,3.93794187104499,
-5.57277579859251));
#39597=CARTESIAN_POINT('Ctrl Pts',(-0.391351836138015,4.,-5.51067764861519));
#39598=CARTESIAN_POINT('Ctrl Pts',(-3.46944695195361E-16,4.,-5.51067764861519));
#39599=CARTESIAN_POINT('',(-3.67394039744206E-16,4.09192982960655,-5.54875623082487));
#39600=CARTESIAN_POINT('',(-3.67394039744206E-16,1.14805029709526,-4.32936140246614));
#39601=CARTESIAN_POINT('Origin',(0.,2.94387953251129,-8.32039482835873));
#39602=CARTESIAN_POINT('Ctrl Pts',(-5.55111512312578E-16,4.,-5.51067764861519));
#39603=CARTESIAN_POINT('Ctrl Pts',(0.391351836138015,4.,-5.51067764861519));
#39604=CARTESIAN_POINT('Ctrl Pts',(0.804950314595278,3.93794187104499,-5.57277579859251));
#39605=CARTESIAN_POINT('Ctrl Pts',(1.5580225174343,3.70511768616704,-5.82557882438308));
#39606=CARTESIAN_POINT('Ctrl Pts',(1.897815678339,3.53535819041829,-6.01625804314877));
#39607=CARTESIAN_POINT('Ctrl Pts',(2.42146694806282,3.19843151589414,-6.46722664985983));
#39608=CARTESIAN_POINT('Ctrl Pts',(2.64444489381139,3.00792702197672,-6.75569806071639));
#39609=CARTESIAN_POINT('Ctrl Pts',(2.79030270745925,2.86604495955758,-7.09544824938184));
#39610=CARTESIAN_POINT('Ctrl Pts',(2.791487395233,2.86489106908469,-7.0982224809144));
#39611=CARTESIAN_POINT('Ctrl Pts',(2.79266716119614,2.86374058300969,-7.10099999999999));
#39612=CARTESIAN_POINT('Origin',(0.,0.,-13.5441803724939));
#39613=CARTESIAN_POINT('',(4.,-4.89858719658941E-16,-7.101));
#39614=CARTESIAN_POINT('Origin',(0.,0.,-7.101));
#39615=CARTESIAN_POINT('',(-4.,-4.89858719658941E-16,-7.101));
#39616=CARTESIAN_POINT('Origin',(0.,0.,-7.101));
#39617=CARTESIAN_POINT('Origin',(0.,0.,-7.101));
#39618=CARTESIAN_POINT('',(4.,4.20648087646404E-14,-3.));
#39619=CARTESIAN_POINT('',(4.,-4.89858719658941E-16,-13.5441803724939));
#39620=CARTESIAN_POINT('',(2.00000000000003,-3.46410161513774,-3.));
#39621=CARTESIAN_POINT('Origin',(0.,0.,-3.));
#39622=CARTESIAN_POINT('',(-1.99999999999998,-3.46410161513777,-3.));
#39623=CARTESIAN_POINT('Origin',(0.,0.,-3.));
#39624=CARTESIAN_POINT('',(-4.,-1.4271988688003E-14,-3.));
#39625=CARTESIAN_POINT('Origin',(0.,0.,-3.));
#39626=CARTESIAN_POINT('',(-2.,3.46410161513775,-3.));
#39627=CARTESIAN_POINT('Origin',(0.,0.,-3.));
#39628=CARTESIAN_POINT('',(1.99999999999999,3.46410161513778,-3.));
#39629=CARTESIAN_POINT('Origin',(0.,0.,-3.));
#39630=CARTESIAN_POINT('Origin',(0.,0.,-3.));
#39631=CARTESIAN_POINT('Origin',(0.,0.,-7.101));
#39632=CARTESIAN_POINT('',(-2.44929359829471E-16,-2.99951956532372E-32,
-11.101));
#39633=CARTESIAN_POINT('Origin',(0.,0.,-7.101));
#39634=CARTESIAN_POINT('Origin',(0.,6.32237232699421,-5.39024356304375));
#39635=CARTESIAN_POINT('',(3.46410161513776,4.79163859753387,-9.08576169308891));
#39636=CARTESIAN_POINT('Origin',(0.,4.79163859753387,-9.08576169308891));
#39637=CARTESIAN_POINT('',(-3.46410161513776,4.79163859753387,-9.08576169308891));
#39638=CARTESIAN_POINT('Origin',(0.,4.79163859753386,-9.08576169308891));
#39639=CARTESIAN_POINT('',(-1.73205080756888,5.93968889462913,-6.31412309555504));
#39640=CARTESIAN_POINT('Origin',(0.,4.79163859753386,-9.08576169308891));
#39641=CARTESIAN_POINT('',(1.73205080756888,5.93968889462913,-6.31412309555504));
#39642=CARTESIAN_POINT('Origin',(0.,4.79163859753386,-9.08576169308891));
#39643=CARTESIAN_POINT('Origin',(0.,4.79163859753386,-9.08576169308891));
#39644=CARTESIAN_POINT('Origin',(0.,4.47461326197163,-4.62487669831358));
#39645=CARTESIAN_POINT('',(3.46410161513776,2.94387953251129,-8.32039482835873));
#39646=CARTESIAN_POINT('Origin',(0.,2.94387953251129,-8.32039482835873));
#39647=CARTESIAN_POINT('',(-3.46410161513776,2.94387953251129,-8.32039482835873));
#39648=CARTESIAN_POINT('Origin',(0.,2.94387953251129,-8.32039482835873));
#39649=CARTESIAN_POINT('',(-1.73205080756888,1.79582923541603,-11.0920334258926));
#39650=CARTESIAN_POINT('Origin',(0.,2.94387953251129,-8.32039482835873));
#39651=CARTESIAN_POINT('',(1.73205080756888,1.79582923541603,-11.0920334258926));
#39652=CARTESIAN_POINT('Origin',(0.,2.94387953251129,-8.32039482835873));
#39653=CARTESIAN_POINT('Origin',(0.,2.94387953251129,-8.32039482835873));
#39654=CARTESIAN_POINT('Origin',(0.,0.,-3.));
#39655=CARTESIAN_POINT('',(-4.00000000000001,2.3094010767585,-3.));
#39656=CARTESIAN_POINT('',(-4.00000000000001,2.3094010767585,-3.));
#39657=CARTESIAN_POINT('',(0.,4.61880215351701,-3.));
#39658=CARTESIAN_POINT('Origin',(0.,0.,-3.));
#39659=CARTESIAN_POINT('',(0.,4.61880215351701,-3.));
#39660=CARTESIAN_POINT('',(0.,4.61880215351701,-3.));
#39661=CARTESIAN_POINT('',(3.99999999999998,2.30940107675855,-3.));
#39662=CARTESIAN_POINT('Origin',(0.,0.,-3.));
#39663=CARTESIAN_POINT('',(3.99999999999998,2.30940107675855,-3.));
#39664=CARTESIAN_POINT('',(3.99999999999998,2.30940107675855,-3.));
#39665=CARTESIAN_POINT('',(4.00000000000002,-2.30940107675847,-3.));
#39666=CARTESIAN_POINT('Origin',(0.,0.,-3.));
#39667=CARTESIAN_POINT('',(4.00000000000002,-2.30940107675847,-3.));
#39668=CARTESIAN_POINT('',(4.00000000000002,-2.30940107675847,-3.));
#39669=CARTESIAN_POINT('',(3.22529230536262E-14,-4.61880215351701,-3.));
#39670=CARTESIAN_POINT('Origin',(0.,0.,-3.));
#39671=CARTESIAN_POINT('',(3.22529230536262E-14,-4.61880215351701,-3.));
#39672=CARTESIAN_POINT('',(3.22529230536262E-14,-4.61880215351701,-3.));
#39673=CARTESIAN_POINT('',(-3.99999999999999,-2.30940107675852,-3.));
#39674=CARTESIAN_POINT('Origin',(0.,0.,-3.));
#39675=CARTESIAN_POINT('',(-3.99999999999999,-2.30940107675852,-3.));
#39676=CARTESIAN_POINT('',(-3.99999999999999,-2.30940107675852,-3.));
#39677=CARTESIAN_POINT('',(-4.00000000000001,2.3094010767585,-3.));
#39678=CARTESIAN_POINT('Origin',(3.99999999999998,2.30940107675855,-3.));
#39679=CARTESIAN_POINT('',(3.99999999999998,2.30940107675855,0.));
#39680=CARTESIAN_POINT('',(0.,4.61880215351701,0.));
#39681=CARTESIAN_POINT('',(3.99999999999998,2.30940107675855,0.));
#39682=CARTESIAN_POINT('',(3.99999999999998,2.30940107675855,-3.));
#39683=CARTESIAN_POINT('',(0.,4.61880215351701,-3.));
#39684=CARTESIAN_POINT('Origin',(4.00000000000002,-2.30940107675847,-3.));
#39685=CARTESIAN_POINT('',(4.00000000000002,-2.30940107675847,0.));
#39686=CARTESIAN_POINT('',(4.00000000000002,-2.30940107675847,0.));
#39687=CARTESIAN_POINT('',(4.00000000000002,-2.30940107675847,-3.));
#39688=CARTESIAN_POINT('Origin',(3.22529230536262E-14,-4.61880215351701,
-3.));
#39689=CARTESIAN_POINT('',(3.22529230536262E-14,-4.61880215351701,0.));
#39690=CARTESIAN_POINT('',(3.22529230536262E-14,-4.61880215351701,0.));
#39691=CARTESIAN_POINT('',(3.22529230536262E-14,-4.61880215351701,-3.));
#39692=CARTESIAN_POINT('Origin',(-3.99999999999999,-2.30940107675852,-3.));
#39693=CARTESIAN_POINT('',(-3.99999999999999,-2.30940107675852,0.));
#39694=CARTESIAN_POINT('',(-3.99999999999999,-2.30940107675852,0.));
#39695=CARTESIAN_POINT('',(-3.99999999999999,-2.30940107675852,-3.));
#39696=CARTESIAN_POINT('Origin',(-4.00000000000001,2.3094010767585,-3.));
#39697=CARTESIAN_POINT('',(-4.00000000000001,2.3094010767585,0.));
#39698=CARTESIAN_POINT('',(-4.00000000000001,2.3094010767585,0.));
#39699=CARTESIAN_POINT('',(-4.00000000000001,2.3094010767585,-3.));
#39700=CARTESIAN_POINT('Origin',(0.,4.61880215351701,-3.));
#39701=CARTESIAN_POINT('',(0.,4.61880215351701,0.));
#39702=CARTESIAN_POINT('Origin',(0.,0.,0.));
#39703=CARTESIAN_POINT('Origin',(0.,2.94387953251129,-8.32039482835873));
#39704=CARTESIAN_POINT('',(-3.46410161513776,3.9950957193956,-6.59103842936755));
#39705=CARTESIAN_POINT('Ctrl Pts',(-3.46410161513776,2.94387953251129,-8.32039482835873));
#39706=CARTESIAN_POINT('Ctrl Pts',(-3.46410161513776,3.29908753061063,-7.46284686188391));
#39707=CARTESIAN_POINT('Ctrl Pts',(-3.46410161513776,3.99509571941731,-6.59103842934036));
#39708=CARTESIAN_POINT('Ctrl Pts',(-3.46410161515884,3.99509571939744,-6.59103842938149));
#39709=CARTESIAN_POINT('Ctrl Pts',(-2.53589838487072,3.91432583055759,-5.97753021406059));
#39710=CARTESIAN_POINT('Ctrl Pts',(-1.73205080756888,4.09192982960655,-5.54875623082487));
#39711=CARTESIAN_POINT('Origin',(0.,2.94387953251129,-8.32039482835873));
#39712=CARTESIAN_POINT('',(-3.46410161513776,2.46436198993525,-10.2865565594127));
#39713=CARTESIAN_POINT('Ctrl Pts',(-1.73205080756888,1.79582923541603,-11.0920334258926));
#39714=CARTESIAN_POINT('Ctrl Pts',(-2.53589838486591,1.97343323446393,-10.6632594426594));
#39715=CARTESIAN_POINT('Ctrl Pts',(-3.46410161514687,2.46436198994007,-10.286556559409));
#39716=CARTESIAN_POINT('Ctrl Pts',(-3.46410161513776,2.46436198993072,-10.2865565594531));
#39717=CARTESIAN_POINT('Ctrl Pts',(-3.46410161513776,2.58867153441109,-9.17794279483566));
#39718=CARTESIAN_POINT('Ctrl Pts',(-3.46410161513776,2.94387953251129,-8.32039482835874));
#39719=CARTESIAN_POINT('Origin',(0.,2.94387953251129,-8.32039482835873));
#39720=CARTESIAN_POINT('',(3.90312782094782E-15,1.69899512520508,-12.1343156244353));
#39721=CARTESIAN_POINT('Ctrl Pts',(9.12142465330762E-12,1.69899512520587,
-12.1343156244413));
#39722=CARTESIAN_POINT('Ctrl Pts',(-0.928203230271842,1.61822523636812,
-11.5208074091258));
#39723=CARTESIAN_POINT('Ctrl Pts',(-1.73205080756888,1.79582923541603,-11.0920334258926));
#39724=CARTESIAN_POINT('Ctrl Pts',(1.73205080756888,1.79582923541603,-11.0920334258926));
#39725=CARTESIAN_POINT('Ctrl Pts',(0.928203230271956,1.61822523636815,-11.5208074091257));
#39726=CARTESIAN_POINT('Ctrl Pts',(-8.8435124366233E-12,1.69899512520584,
-12.1343156244411));
#39727=CARTESIAN_POINT('Origin',(0.,2.94387953251129,-8.32039482835873));
#39728=CARTESIAN_POINT('',(3.46410161513776,2.46436198993525,-10.2865565594127));
#39729=CARTESIAN_POINT('Ctrl Pts',(3.46410161514661,2.46436198993993,-10.2865565594091));
#39730=CARTESIAN_POINT('Ctrl Pts',(2.53589838486581,1.97343323446391,-10.6632594426595));
#39731=CARTESIAN_POINT('Ctrl Pts',(1.73205080756888,1.79582923541603,-11.0920334258926));
#39732=CARTESIAN_POINT('Ctrl Pts',(3.46410161513776,2.94387953251129,-8.32039482835873));
#39733=CARTESIAN_POINT('Ctrl Pts',(3.46410161513776,2.58867153441108,-9.17794279483565));
#39734=CARTESIAN_POINT('Ctrl Pts',(3.46410161513776,2.46436198993072,-10.2865565594531));
#39735=CARTESIAN_POINT('Origin',(0.,2.94387953251129,-8.32039482835873));
#39736=CARTESIAN_POINT('',(3.46410161513776,3.9950957193956,-6.59103842936756));
#39737=CARTESIAN_POINT('Ctrl Pts',(3.46410161513776,3.99509571941731,-6.59103842934036));
#39738=CARTESIAN_POINT('Ctrl Pts',(3.46410161513776,3.29908753061063,-7.46284686188391));
#39739=CARTESIAN_POINT('Ctrl Pts',(3.46410161513776,2.94387953251129,-8.32039482835873));
#39740=CARTESIAN_POINT('Ctrl Pts',(1.73205080756888,4.09192982960655,-5.54875623082487));
#39741=CARTESIAN_POINT('Ctrl Pts',(2.53589838487052,3.91432583055763,-5.97753021406048));
#39742=CARTESIAN_POINT('Ctrl Pts',(3.46410161515834,3.99509571939739,-6.59103842938115));
#39743=CARTESIAN_POINT('Origin',(0.,4.50578927537974,-8.96735902705751));
#39744=CARTESIAN_POINT('',(3.46410161513776,3.74042241064956,-10.8151180920801));
#39745=CARTESIAN_POINT('Ctrl Pts',(3.46410161513776,3.74042241062786,-10.8151180921073));
#39746=CARTESIAN_POINT('Ctrl Pts',(3.46410161513776,4.43643059943453,-9.94330965956373));
#39747=CARTESIAN_POINT('Ctrl Pts',(3.46410161513776,4.79163859753386,-9.08576169308893));
#39748=CARTESIAN_POINT('Ctrl Pts',(1.73205080756889,3.64358830043861,-11.8574002906228));
#39749=CARTESIAN_POINT('Ctrl Pts',(2.53589838487114,3.82119229948767,-11.4286263073868));
#39750=CARTESIAN_POINT('Ctrl Pts',(3.46410161515986,3.74042241064764,-10.8151180920655));
#39751=CARTESIAN_POINT('Origin',(0.,4.50578927537974,-8.96735902705751));
#39752=CARTESIAN_POINT('',(3.46410161513776,5.27115614010992,-7.11959996203494));
#39753=CARTESIAN_POINT('Ctrl Pts',(3.46410161514743,5.2711561401048,-7.11959996203886));
#39754=CARTESIAN_POINT('Ctrl Pts',(2.53589838486614,5.76208489558118,-6.74289707878832));
#39755=CARTESIAN_POINT('Ctrl Pts',(1.73205080756888,5.93968889462914,-6.31412309555504));
#39756=CARTESIAN_POINT('Ctrl Pts',(3.46410161513776,4.79163859753387,-9.08576169308891));
#39757=CARTESIAN_POINT('Ctrl Pts',(3.46410161513776,5.14684659563408,-8.22821372661199));
#39758=CARTESIAN_POINT('Ctrl Pts',(3.46410161513776,5.27115614011445,-7.11959996199452));
#39759=CARTESIAN_POINT('Origin',(0.,4.50578927537974,-8.96735902705751));
#39760=CARTESIAN_POINT('',(6.50521303491303E-15,6.03652300484009,-5.27184089701236));
#39761=CARTESIAN_POINT('Ctrl Pts',(9.66462909312592E-12,6.03652300483925,
-5.27184089700597));
#39762=CARTESIAN_POINT('Ctrl Pts',(-0.928203230271627,6.11729289367709,
-5.88534911232177));
#39763=CARTESIAN_POINT('Ctrl Pts',(-1.73205080756888,5.93968889462913,-6.31412309555505));
#39764=CARTESIAN_POINT('Ctrl Pts',(1.73205080756888,5.93968889462914,-6.31412309555504));
#39765=CARTESIAN_POINT('Ctrl Pts',(0.928203230271628,6.11729289367709,-5.88534911232177));
#39766=CARTESIAN_POINT('Ctrl Pts',(-9.6577405477995E-12,6.03652300483925,
-5.27184089700597));
#39767=CARTESIAN_POINT('Origin',(0.,4.50578927537974,-8.96735902705751));
#39768=CARTESIAN_POINT('',(-3.46410161513776,5.27115614010992,-7.11959996203493));
#39769=CARTESIAN_POINT('Ctrl Pts',(-3.46410161513776,5.27115614011445,-7.1195999619945));
#39770=CARTESIAN_POINT('Ctrl Pts',(-3.46410161513776,5.14684659563408,-8.22821372661199));
#39771=CARTESIAN_POINT('Ctrl Pts',(-3.46410161513776,4.79163859753387,-9.08576169308891));
#39772=CARTESIAN_POINT('Ctrl Pts',(-1.73205080756888,5.93968889462913,-6.31412309555505));
#39773=CARTESIAN_POINT('Ctrl Pts',(-2.53589838486613,5.76208489558118,-6.74289707878832));
#39774=CARTESIAN_POINT('Ctrl Pts',(-3.46410161514742,5.27115614010481,-7.11959996203885));
#39775=CARTESIAN_POINT('Origin',(0.,4.50578927537974,-8.96735902705751));
#39776=CARTESIAN_POINT('',(-3.46410161513776,3.74042241064957,-10.8151180920801));
#39777=CARTESIAN_POINT('Ctrl Pts',(-3.46410161515986,3.74042241064764,-10.8151180920655));
#39778=CARTESIAN_POINT('Ctrl Pts',(-2.53589838487113,3.82119229948767,-11.4286263073868));
#39779=CARTESIAN_POINT('Ctrl Pts',(-1.73205080756889,3.64358830043861,-11.8574002906228));
#39780=CARTESIAN_POINT('Ctrl Pts',(-3.46410161513776,4.79163859753387,-9.08576169308891));
#39781=CARTESIAN_POINT('Ctrl Pts',(-3.46410161513776,4.43643059943453,-9.94330965956373));
#39782=CARTESIAN_POINT('Ctrl Pts',(-3.46410161513776,3.74042241062786,-10.8151180921073));
#39783=CARTESIAN_POINT('Origin',(-8.67361737988404E-16,1.41314580305094,
-12.0159129584039));
#39784=CARTESIAN_POINT('',(-8.67361737988404E-16,1.41314580305094,-12.0159129584039));
#39785=CARTESIAN_POINT('',(-3.46410161513776,2.17851266778112,-10.1681538933813));
#39786=CARTESIAN_POINT('Origin',(-3.46410161513776,2.17851266778112,-10.1681538933813));
#39787=CARTESIAN_POINT('',(-3.46410161513776,3.70924639724147,-6.47263576333616));
#39788=CARTESIAN_POINT('Origin',(-3.46410161513776,3.70924639724147,-6.47263576333616));
#39789=CARTESIAN_POINT('',(7.02214595811131E-16,4.47461326197164,-4.62487669831358));
#39790=CARTESIAN_POINT('Origin',(7.02214595811131E-16,4.47461326197164,
-4.62487669831358));
#39791=CARTESIAN_POINT('',(3.46410161513776,3.70924639724147,-6.47263576333616));
#39792=CARTESIAN_POINT('Origin',(3.46410161513776,3.70924639724147,-6.47263576333616));
#39793=CARTESIAN_POINT('',(3.46410161513776,2.17851266778112,-10.1681538933813));
#39794=CARTESIAN_POINT('Origin',(3.46410161513776,2.17851266778112,-10.1681538933813));
#39795=CARTESIAN_POINT('Origin',(0.944722181384557,9.66424685661038,-11.6944373635354));
#39796=CARTESIAN_POINT('',(0.,0.,0.));
#39797=CARTESIAN_POINT('',(2.22044604925031E-13,22.,-196.455545580277));
#39798=CARTESIAN_POINT('',(0.,30.,-197.455545580276));
#39799=CARTESIAN_POINT('',(2.35922392732846E-13,22.,-368.455545580276));
#39800=CARTESIAN_POINT('',(0.,30.,-369.455545580276));
#39801=CARTESIAN_POINT('',(0.,0.,0.));
#39802=CARTESIAN_POINT('',(0.,22.,-196.455545580277));
#39803=CARTESIAN_POINT('',(0.,30.,-197.455545580276));
#39804=CARTESIAN_POINT('',(0.,22.,-368.455545580276));
#39805=CARTESIAN_POINT('',(0.,30.,-369.455545580276));
#39806=CARTESIAN_POINT('',(0.,0.,0.));
#39807=CARTESIAN_POINT('',(0.,0.,0.));
#39808=CARTESIAN_POINT('Origin',(-10.,0.,0.));
#39809=CARTESIAN_POINT('',(830.2,-7.34788079488416E-16,-6.00000000000003));
#39810=CARTESIAN_POINT('Origin',(830.2,0.,0.));
#39811=CARTESIAN_POINT('',(849.,-7.34788079488416E-16,-6.00000000000003));
#39812=CARTESIAN_POINT('',(-10.,-7.34788079488416E-16,-6.00000000000003));
#39813=CARTESIAN_POINT('',(849.,-2.,5.65685424949241));
#39814=CARTESIAN_POINT('Origin',(849.,0.,0.));
#39815=CARTESIAN_POINT('',(840.,-2.,5.65685424949241));
#39816=CARTESIAN_POINT('',(-10.,-2.,5.65685424949241));
#39817=CARTESIAN_POINT('',(840.,2.,5.65685424949241));
#39818=CARTESIAN_POINT('Ctrl Pts',(840.,2.,5.65685424949241));
#39819=CARTESIAN_POINT('Ctrl Pts',(839.746707879184,2.,5.65685424949241));
#39820=CARTESIAN_POINT('Ctrl Pts',(839.477996053073,1.94898067853764,5.67565356574254));
#39821=CARTESIAN_POINT('Ctrl Pts',(838.985893640085,1.74430581525273,5.74186082552468));
#39822=CARTESIAN_POINT('Ctrl Pts',(838.762313835253,1.59074095999942,5.788137712126));
#39823=CARTESIAN_POINT('Ctrl Pts',(838.409340913544,1.23776803829002,5.87374622031368));
#39824=CARTESIAN_POINT('Ctrl Pts',(838.255713027767,1.01415562391481,5.91887391060683));
#39825=CARTESIAN_POINT('Ctrl Pts',(838.050991158394,0.521932274441699,5.98240475886915));
#39826=CARTESIAN_POINT('Ctrl Pts',(838.,0.253174643734701,6.00000000000003));
#39827=CARTESIAN_POINT('Ctrl Pts',(838.,-0.253174643734697,6.00000000000003));
#39828=CARTESIAN_POINT('Ctrl Pts',(838.050991158394,-0.521932274441696,
5.98240475886915));
#39829=CARTESIAN_POINT('Ctrl Pts',(838.255713027767,-1.0141556239148,5.91887391060683));
#39830=CARTESIAN_POINT('Ctrl Pts',(838.409340913544,-1.23776803829001,5.87374622031368));
#39831=CARTESIAN_POINT('Ctrl Pts',(838.762313835253,-1.59074095999941,5.788137712126));
#39832=CARTESIAN_POINT('Ctrl Pts',(838.985893640085,-1.74430581525273,5.74186082552468));
#39833=CARTESIAN_POINT('Ctrl Pts',(839.477996053073,-1.94898067853763,5.67565356574254));
#39834=CARTESIAN_POINT('Ctrl Pts',(839.746707879184,-2.,5.65685424949241));
#39835=CARTESIAN_POINT('Ctrl Pts',(840.,-2.,5.65685424949241));
#39836=CARTESIAN_POINT('',(849.,2.,5.65685424949241));
#39837=CARTESIAN_POINT('',(-10.,2.,5.65685424949241));
#39838=CARTESIAN_POINT('Origin',(849.,0.,0.));
#39839=CARTESIAN_POINT('Origin',(830.2,0.,0.));
#39840=CARTESIAN_POINT('',(830.,-7.59281015471362E-16,-6.20000000000003));
#39841=CARTESIAN_POINT('Origin',(830.,0.,0.));
#39842=CARTESIAN_POINT('Origin',(830.2,-7.59281015471362E-16,-6.20000000000003));
#39843=CARTESIAN_POINT('Origin',(830.,0.,0.));
#39844=CARTESIAN_POINT('',(829.5,-9.18485099360529E-16,-7.50000000000011));
#39845=CARTESIAN_POINT('Origin',(829.5,0.,0.));
#39846=CARTESIAN_POINT('',(830.,-8.5725275940317E-16,-7.00000000000019));
#39847=CARTESIAN_POINT('',(830.,-8.5725275940317E-16,-7.00000000000019));
#39848=CARTESIAN_POINT('Origin',(830.,0.,0.));
#39849=CARTESIAN_POINT('Origin',(-10.,0.,0.));
#39850=CARTESIAN_POINT('',(790.2,-9.18485099360528E-16,-7.5000000000001));
#39851=CARTESIAN_POINT('Origin',(790.2,0.,0.));
#39852=CARTESIAN_POINT('',(-10.,-9.18485099360528E-16,-7.5000000000001));
#39853=CARTESIAN_POINT('Origin',(790.2,0.,0.));
#39854=CARTESIAN_POINT('',(790.,-9.42978035343474E-16,-7.7000000000001));
#39855=CARTESIAN_POINT('Origin',(790.,0.,0.));
#39856=CARTESIAN_POINT('Origin',(790.2,-9.42978035343474E-16,-7.7000000000001));
#39857=CARTESIAN_POINT('Origin',(790.,0.,0.));
#39858=CARTESIAN_POINT('',(789.,-1.22464679914736E-15,-10.0000000000001));
#39859=CARTESIAN_POINT('Origin',(789.,0.,0.));
#39860=CARTESIAN_POINT('',(790.,-1.10218211923262E-15,-9.00000000000005));
#39861=CARTESIAN_POINT('',(790.,-1.10218211923262E-15,-9.00000000000005));
#39862=CARTESIAN_POINT('Origin',(790.,0.,0.));
#39863=CARTESIAN_POINT('Origin',(-10.,0.,0.));
#39864=CARTESIAN_POINT('',(14.,1.22464679914734E-15,9.9999999999999));
#39865=CARTESIAN_POINT('',(14.,-1.22464679914735E-15,-9.99999999999998));
#39866=CARTESIAN_POINT('Origin',(14.,0.,0.));
#39867=CARTESIAN_POINT('Origin',(14.,0.,0.));
#39868=CARTESIAN_POINT('',(-10.,-1.22464679914735E-15,-9.99999999999998));
#39869=CARTESIAN_POINT('Origin',(14.,0.,0.));
#39870=CARTESIAN_POINT('',(12.9999999999999,-1.10218211923261E-15,8.99999999999991));
#39871=CARTESIAN_POINT('',(14.,-1.22464679914734E-15,9.9999999999999));
#39872=CARTESIAN_POINT('Origin',(12.9999999999999,0.,0.));
#39873=CARTESIAN_POINT('Origin',(12.8,0.,0.));
#39874=CARTESIAN_POINT('',(12.8,-9.18485099360515E-16,-7.5));
#39875=CARTESIAN_POINT('Origin',(12.8,0.,0.));
#39876=CARTESIAN_POINT('',(13.,-9.42978035343462E-16,-7.7));
#39877=CARTESIAN_POINT('Origin',(12.8,-9.42978035343462E-16,-7.7));
#39878=CARTESIAN_POINT('Origin',(13.,0.,0.));
#39879=CARTESIAN_POINT('Origin',(-10.,0.,0.));
#39880=CARTESIAN_POINT('',(4.00000000000001,-9.18485099360515E-16,-7.5));
#39881=CARTESIAN_POINT('Origin',(4.00000000000001,0.,0.));
#39882=CARTESIAN_POINT('',(-10.,-9.18485099360515E-16,-7.5));
#39883=CARTESIAN_POINT('Origin',(-10.,0.,0.));
#39884=CARTESIAN_POINT('',(2.85000000000001,-8.75622461390357E-16,-7.15));
#39885=CARTESIAN_POINT('Origin',(2.85000000000001,0.,0.));
#39886=CARTESIAN_POINT('',(4.00000000000001,-8.75622461390357E-16,-7.15));
#39887=CARTESIAN_POINT('',(-10.,-8.75622461390357E-16,-7.15));
#39888=CARTESIAN_POINT('Origin',(4.00000000000001,0.,0.));
#39889=CARTESIAN_POINT('Origin',(-10.,0.,0.));
#39890=CARTESIAN_POINT('',(1.,9.18485099360515E-16,7.5));
#39891=CARTESIAN_POINT('',(1.,-9.18485099360515E-16,-7.5));
#39892=CARTESIAN_POINT('Origin',(1.,0.,0.));
#39893=CARTESIAN_POINT('Origin',(1.,0.,0.));
#39894=CARTESIAN_POINT('',(2.85000000000001,-9.18485099360515E-16,-7.5));
#39895=CARTESIAN_POINT('',(-10.,-9.18485099360515E-16,-7.5));
#39896=CARTESIAN_POINT('Origin',(2.85000000000001,0.,0.));
#39897=CARTESIAN_POINT('Origin',(1.,0.,0.));
#39898=CARTESIAN_POINT('',(1.80411241501588E-15,-7.9602041944578E-16,6.5));
#39899=CARTESIAN_POINT('',(1.,-9.18485099360515E-16,7.5));
#39900=CARTESIAN_POINT('Origin',(1.73472347597681E-15,0.,0.));
#39901=CARTESIAN_POINT('Origin',(2.85000000000001,7.5,0.));
#39902=CARTESIAN_POINT('Origin',(4.00000000000001,7.5,0.));
#39903=CARTESIAN_POINT('Origin',(13.,8.99999999999991,0.));
#39904=CARTESIAN_POINT('Origin',(790.,7.7000000000001,0.));
#39905=CARTESIAN_POINT('Origin',(830.,6.20000000000003,0.));
#39906=CARTESIAN_POINT('Origin',(850.,0.,0.));
#39907=CARTESIAN_POINT('',(850.,2.,4.58257569495592));
#39908=CARTESIAN_POINT('Ctrl Pts',(849.000000000013,2.,5.65685424947835));
#39909=CARTESIAN_POINT('Ctrl Pts',(849.552457927857,2.,5.07088412883036));
#39910=CARTESIAN_POINT('Ctrl Pts',(850.,2.,4.58257569495594));
#39911=CARTESIAN_POINT('',(850.,-2.,4.58257569495592));
#39912=CARTESIAN_POINT('Origin',(850.,0.,0.));
#39913=CARTESIAN_POINT('Ctrl Pts',(850.000000000053,-2.,4.58257569489865));
#39914=CARTESIAN_POINT('Ctrl Pts',(849.552457927889,-2.,5.07088412879636));
#39915=CARTESIAN_POINT('Ctrl Pts',(849.000000000013,-2.,5.65685424947841));
#39916=CARTESIAN_POINT('Origin',(850.,0.,0.));
#39917=CARTESIAN_POINT('',(850.,2.,3.50000000000002));
#39918=CARTESIAN_POINT('',(850.,2.,6.00000000000002));
#39919=CARTESIAN_POINT('',(850.,-2.,3.50000000000002));
#39920=CARTESIAN_POINT('',(850.,2.,3.50000000000002));
#39921=CARTESIAN_POINT('',(850.,-2.,-6.93889390390722E-16));
#39922=CARTESIAN_POINT('Origin',(4.40872847693047E-16,6.5,0.));
#39923=CARTESIAN_POINT('Origin',(838.,2.,6.00000000000002));
#39924=CARTESIAN_POINT('',(840.,2.,3.50000000000002));
#39925=CARTESIAN_POINT('',(840.,2.,3.50000000000002));
#39926=CARTESIAN_POINT('',(838.,2.,3.50000000000002));
#39927=CARTESIAN_POINT('Origin',(838.,-2.,3.50000000000002));
#39928=CARTESIAN_POINT('',(840.,-2.,3.50000000000002));
#39929=CARTESIAN_POINT('',(838.,-2.,3.50000000000002));
#39930=CARTESIAN_POINT('',(840.,-2.,5.65685424949241));
#39931=CARTESIAN_POINT('Origin',(838.,2.,3.50000000000002));
#39932=CARTESIAN_POINT('Origin',(840.,1.30104260698261E-15,3.50000000000002));
#39933=CARTESIAN_POINT('Origin',(840.,6.93889390390719E-16,-1.20370621524202E-31));
#39934=CARTESIAN_POINT('',(0.,0.,0.));
#39935=CARTESIAN_POINT('Origin',(5.,0.,0.));
#39936=CARTESIAN_POINT('',(5.,25.755227454346,13.3292257380129));
#39937=CARTESIAN_POINT('Ctrl Pts',(5.,25.755227454346,13.3292257380129));
#39938=CARTESIAN_POINT('Ctrl Pts',(4.69114589073871,25.755227454346,13.3292257380129));
#39939=CARTESIAN_POINT('Ctrl Pts',(4.36180679068939,25.7839061219684,13.2742617732837));
#39940=CARTESIAN_POINT('Ctrl Pts',(3.75612725368286,25.8981524209919,13.0499632820151));
#39941=CARTESIAN_POINT('Ctrl Pts',(3.47977417462311,25.9834526414702,12.8805267791833));
#39942=CARTESIAN_POINT('Ctrl Pts',(3.04338216488515,26.1746646562439,12.4873820813809));
#39943=CARTESIAN_POINT('Ctrl Pts',(2.85419996970905,26.2933036476544,12.2374013605568));
#39944=CARTESIAN_POINT('Ctrl Pts',(2.60325479232307,26.5432548470335,11.6853511240012));
#39945=CARTESIAN_POINT('Ctrl Pts',(2.54150000000001,26.6743132994447,11.3831630283214));
#39946=CARTESIAN_POINT('Ctrl Pts',(2.54150000000001,26.9106995862099,10.8124760488539));
#39947=CARTESIAN_POINT('Ctrl Pts',(2.60325479232307,27.0317065174271,10.5061244767731));
#39948=CARTESIAN_POINT('Ctrl Pts',(2.85419996970905,27.2453227952046,9.93902382290224));
#39949=CARTESIAN_POINT('Ctrl Pts',(3.04338216488515,27.3381954227257,9.67837032470212));
#39950=CARTESIAN_POINT('Ctrl Pts',(3.47977417462311,27.4809833922385,9.26516773060774));
#39951=CARTESIAN_POINT('Ctrl Pts',(3.75612725368287,27.5404767280345,9.08504166613792));
#39952=CARTESIAN_POINT('Ctrl Pts',(4.36180679068939,27.6182953794554,8.84565434918702));
#39953=CARTESIAN_POINT('Ctrl Pts',(4.69114589073871,27.6368818912851,8.78651007665487));
#39954=CARTESIAN_POINT('Ctrl Pts',(5.30885410926129,27.6368818912851,8.78651007665487));
#39955=CARTESIAN_POINT('Ctrl Pts',(5.63819320931061,27.6182953794554,8.84565434918702));
#39956=CARTESIAN_POINT('Ctrl Pts',(6.24387274631713,27.5404767280345,9.08504166613792));
#39957=CARTESIAN_POINT('Ctrl Pts',(6.52022582537689,27.4809833922385,9.26516773060774));
#39958=CARTESIAN_POINT('Ctrl Pts',(6.95661783511485,27.3381954227257,9.67837032470212));
#39959=CARTESIAN_POINT('Ctrl Pts',(7.14580003029095,27.2453227952046,9.93902382290224));
#39960=CARTESIAN_POINT('Ctrl Pts',(7.39674520767693,27.0317065174271,10.5061244767731));
#39961=CARTESIAN_POINT('Ctrl Pts',(7.45849999999999,26.9106995862099,10.8124760488539));
#39962=CARTESIAN_POINT('Ctrl Pts',(7.45849999999999,26.6743132994447,11.3831630283214));
#39963=CARTESIAN_POINT('Ctrl Pts',(7.39674520767693,26.5432548470335,11.6853511240012));
#39964=CARTESIAN_POINT('Ctrl Pts',(7.14580003029096,26.2933036476544,12.2374013605568));
#39965=CARTESIAN_POINT('Ctrl Pts',(6.95661783511486,26.1746646562439,12.4873820813809));
#39966=CARTESIAN_POINT('Ctrl Pts',(6.5202258253769,25.9834526414702,12.8805267791833));
#39967=CARTESIAN_POINT('Ctrl Pts',(6.24387274631714,25.8981524209919,13.0499632820151));
#39968=CARTESIAN_POINT('Ctrl Pts',(5.63819320931061,25.7839061219684,13.2742617732837));
#39969=CARTESIAN_POINT('Ctrl Pts',(5.30885410926129,25.755227454346,13.3292257380129));
#39970=CARTESIAN_POINT('Ctrl Pts',(5.,25.755227454346,13.3292257380129));
#39971=CARTESIAN_POINT('',(5.,8.0144099455781,5.98073851829512));
#39972=CARTESIAN_POINT('',(5.,-0.940827218469573,2.27135783067899));
#39973=CARTESIAN_POINT('Ctrl Pts',(5.,8.0144099455781,5.98073851829512));
#39974=CARTESIAN_POINT('Ctrl Pts',(5.31008862954593,8.0144099455781,5.98073851829512));
#39975=CARTESIAN_POINT('Ctrl Pts',(5.63993188917898,8.05340386084043,5.92953036554281));
#39976=CARTESIAN_POINT('Ctrl Pts',(6.24525180858305,8.20369315504142,5.71979564999168));
#39977=CARTESIAN_POINT('Ctrl Pts',(6.52084478062663,8.31410726259137,5.56097433266262));
#39978=CARTESIAN_POINT('Ctrl Pts',(6.95597086860858,8.55158864293188,5.18836525743534));
#39979=CARTESIAN_POINT('Ctrl Pts',(7.14497843142093,8.69464171404924,4.94930727333218));
#39980=CARTESIAN_POINT('Ctrl Pts',(7.39627742385398,8.97925658890556,4.41195966959874));
#39981=CARTESIAN_POINT('Ctrl Pts',(7.45849999999999,9.12014502992114,4.11328147548234));
#39982=CARTESIAN_POINT('Ctrl Pts',(7.45849999999999,9.35744562030459,3.54038717181947));
#39983=CARTESIAN_POINT('Ctrl Pts',(7.39627742385398,9.46901982472393,3.22956662333429));
#39984=CARTESIAN_POINT('Ctrl Pts',(7.14497843142093,9.64772885114073,2.64835138084258));
#39985=CARTESIAN_POINT('Ctrl Pts',(6.95597086860858,9.71561457614021,2.3781580625298));
#39986=CARTESIAN_POINT('Ctrl Pts',(6.52084478062663,9.81116428552076,1.94675896426062));
#39987=CARTESIAN_POINT('Ctrl Pts',(6.24525180858306,9.84539335181388,1.75638076959303));
#39988=CARTESIAN_POINT('Ctrl Pts',(5.63993188917898,9.88742761236105,1.50180535090734));
#39989=CARTESIAN_POINT('Ctrl Pts',(5.31008862954593,9.89606438251724,1.43802285693714));
#39990=CARTESIAN_POINT('Ctrl Pts',(4.68991137045407,9.89606438251724,1.43802285693714));
#39991=CARTESIAN_POINT('Ctrl Pts',(4.36006811082102,9.88742761236105,1.50180535090734));
#39992=CARTESIAN_POINT('Ctrl Pts',(3.75474819141694,9.84539335181388,1.75638076959303));
#39993=CARTESIAN_POINT('Ctrl Pts',(3.47915521937337,9.81116428552076,1.94675896426062));
#39994=CARTESIAN_POINT('Ctrl Pts',(3.04402913139142,9.71561457614021,2.3781580625298));
#39995=CARTESIAN_POINT('Ctrl Pts',(2.85502156857907,9.64772885114073,2.64835138084258));
#39996=CARTESIAN_POINT('Ctrl Pts',(2.60372257614602,9.46901982472393,3.22956662333429));
#39997=CARTESIAN_POINT('Ctrl Pts',(2.54150000000001,9.35744562030459,3.54038717181947));
#39998=CARTESIAN_POINT('Ctrl Pts',(2.54150000000001,9.12014502992114,4.11328147548234));
#39999=CARTESIAN_POINT('Ctrl Pts',(2.60372257614602,8.97925658890556,4.41195966959874));
#40000=CARTESIAN_POINT('Ctrl Pts',(2.85502156857907,8.69464171404924,4.94930727333218));
#40001=CARTESIAN_POINT('Ctrl Pts',(3.04402913139142,8.55158864293188,5.18836525743534));
#40002=CARTESIAN_POINT('Ctrl Pts',(3.47915521937337,8.31410726259137,5.56097433266262));
#40003=CARTESIAN_POINT('Ctrl Pts',(3.75474819141694,8.20369315504142,5.71979564999168));
#40004=CARTESIAN_POINT('Ctrl Pts',(4.36006811082102,8.05340386084043,5.92953036554281));
#40005=CARTESIAN_POINT('Ctrl Pts',(4.68991137045407,8.0144099455781,5.98073851829512));
#40006=CARTESIAN_POINT('Ctrl Pts',(5.,8.0144099455781,5.98073851829512));
#40007=CARTESIAN_POINT('Origin',(10.,16.6170093578838,16.6170093578839));
#40008=CARTESIAN_POINT('',(0.,16.6170093578838,19.9170093578839));
#40009=CARTESIAN_POINT('Origin',(0.,16.6170093578838,16.6170093578839));
#40010=CARTESIAN_POINT('',(10.,16.6170093578838,19.9170093578839));
#40011=CARTESIAN_POINT('',(10.,16.6170093578838,19.9170093578839));
#40012=CARTESIAN_POINT('Origin',(10.,16.6170093578838,16.6170093578839));
#40013=CARTESIAN_POINT('Origin',(10.,23.5,0.));
#40014=CARTESIAN_POINT('',(0.,23.5,3.3));
#40015=CARTESIAN_POINT('Origin',(0.,23.5,0.));
#40016=CARTESIAN_POINT('',(10.,23.5,3.3));
#40017=CARTESIAN_POINT('',(10.,23.5,3.3));
#40018=CARTESIAN_POINT('Origin',(10.,23.5,0.));
#40019=CARTESIAN_POINT('Origin',(10.,16.6170093578838,-16.6170093578839));
#40020=CARTESIAN_POINT('',(0.,16.6170093578838,-13.3170093578839));
#40021=CARTESIAN_POINT('Origin',(0.,16.6170093578838,-16.6170093578839));
#40022=CARTESIAN_POINT('',(10.,16.6170093578838,-13.3170093578839));
#40023=CARTESIAN_POINT('',(10.,16.6170093578838,-13.3170093578839));
#40024=CARTESIAN_POINT('Origin',(10.,16.6170093578838,-16.6170093578839));
#40025=CARTESIAN_POINT('Origin',(10.,-16.6170093578838,16.6170093578839));
#40026=CARTESIAN_POINT('',(0.,-16.6170093578838,19.9170093578839));
#40027=CARTESIAN_POINT('Origin',(0.,-16.6170093578838,16.6170093578839));
#40028=CARTESIAN_POINT('',(10.,-16.6170093578838,19.9170093578839));
#40029=CARTESIAN_POINT('',(10.,-16.6170093578838,19.9170093578839));
#40030=CARTESIAN_POINT('Origin',(10.,-16.6170093578838,16.6170093578839));
#40031=CARTESIAN_POINT('Origin',(10.,-23.5,0.));
#40032=CARTESIAN_POINT('',(0.,-23.5,3.3));
#40033=CARTESIAN_POINT('Origin',(0.,-23.5,0.));
#40034=CARTESIAN_POINT('',(10.,-23.5,3.3));
#40035=CARTESIAN_POINT('',(10.,-23.5,3.3));
#40036=CARTESIAN_POINT('Origin',(10.,-23.5,0.));
#40037=CARTESIAN_POINT('Origin',(10.,-16.6170093578838,-16.6170093578839));
#40038=CARTESIAN_POINT('',(0.,-16.6170093578838,-13.3170093578839));
#40039=CARTESIAN_POINT('Origin',(0.,-16.6170093578838,-16.6170093578839));
#40040=CARTESIAN_POINT('',(10.,-16.6170093578838,-13.3170093578839));
#40041=CARTESIAN_POINT('',(10.,-16.6170093578838,-13.3170093578839));
#40042=CARTESIAN_POINT('Origin',(10.,-16.6170093578838,-16.6170093578839));
#40043=CARTESIAN_POINT('Origin',(-43.5556221990477,0.,0.));
#40044=CARTESIAN_POINT('',(-40.5,-2.20436423846524E-15,-18.));
#40045=CARTESIAN_POINT('Origin',(-40.5,0.,0.));
#40046=CARTESIAN_POINT('',(0.,-2.20436423846524E-15,-18.));
#40047=CARTESIAN_POINT('',(-43.5556221990477,-2.20436423846524E-15,-18.));
#40048=CARTESIAN_POINT('Origin',(0.,0.,0.));
#40049=CARTESIAN_POINT('Origin',(-43.5556221990477,0.,0.));
#40050=CARTESIAN_POINT('',(10.,-1.59204083889156E-15,-13.));
#40051=CARTESIAN_POINT('Origin',(10.,0.,0.));
#40052=CARTESIAN_POINT('',(9.5,-1.59204083889156E-15,-13.));
#40053=CARTESIAN_POINT('',(-43.5556221990477,-1.59204083889156E-15,-13.));
#40054=CARTESIAN_POINT('Origin',(9.5,0.,0.));
#40055=CARTESIAN_POINT('Origin',(-43.5556221990477,0.,0.));
#40056=CARTESIAN_POINT('',(9.5,-1.56142466891288E-15,-12.75));
#40057=CARTESIAN_POINT('Origin',(9.5,0.,0.));
#40058=CARTESIAN_POINT('',(10.,-1.56142466891288E-15,-12.75));
#40059=CARTESIAN_POINT('',(-43.5556221990477,-1.56142466891288E-15,-12.75));
#40060=CARTESIAN_POINT('Origin',(10.,0.,0.));
#40061=CARTESIAN_POINT('Origin',(-43.5556221990477,0.,0.));
#40062=CARTESIAN_POINT('',(10.,-1.22464679914735E-15,-10.));
#40063=CARTESIAN_POINT('Origin',(10.,0.,0.));
#40064=CARTESIAN_POINT('',(-41.,-1.22464679914735E-15,-10.));
#40065=CARTESIAN_POINT('',(-43.5556221990477,-1.22464679914735E-15,-10.));
#40066=CARTESIAN_POINT('Origin',(-41.,0.,0.));
#40067=CARTESIAN_POINT('Origin',(-43.5556221990477,0.,0.));
#40068=CARTESIAN_POINT('',(-41.,-1.56142466891288E-15,-12.75));
#40069=CARTESIAN_POINT('Origin',(-41.,0.,0.));
#40070=CARTESIAN_POINT('',(-40.5,-1.56142466891288E-15,-12.75));
#40071=CARTESIAN_POINT('',(-43.5556221990477,-1.56142466891288E-15,-12.75));
#40072=CARTESIAN_POINT('Origin',(-40.5,0.,0.));
#40073=CARTESIAN_POINT('Origin',(-43.5556221990477,0.,0.));
#40074=CARTESIAN_POINT('',(-40.5,-1.59204083889156E-15,-13.));
#40075=CARTESIAN_POINT('Origin',(-40.5,0.,0.));
#40076=CARTESIAN_POINT('',(-41.,-1.59204083889156E-15,-13.));
#40077=CARTESIAN_POINT('',(-43.5556221990477,-1.59204083889156E-15,-13.));
#40078=CARTESIAN_POINT('Origin',(-41.,0.,0.));
#40079=CARTESIAN_POINT('Origin',(-40.5,0.,0.));
#40080=CARTESIAN_POINT('',(-41.,-2.14313189850787E-15,-17.5));
#40081=CARTESIAN_POINT('Origin',(-41.,0.,0.));
#40082=CARTESIAN_POINT('Origin',(-40.5,-2.14313189850787E-15,-17.5));
#40083=CARTESIAN_POINT('Origin',(10.,28.,0.));
#40084=CARTESIAN_POINT('',(10.,17.3205080756888,22.));
#40085=CARTESIAN_POINT('',(10.,-17.3205080756887,22.));
#40086=CARTESIAN_POINT('',(10.,29.,22.));
#40087=CARTESIAN_POINT('',(10.,-17.3205080756887,-22.));
#40088=CARTESIAN_POINT('Origin',(10.,0.,0.));
#40089=CARTESIAN_POINT('',(10.,17.3205080756888,-22.));
#40090=CARTESIAN_POINT('',(10.,29.,-22.));
#40091=CARTESIAN_POINT('Origin',(10.,0.,0.));
#40092=CARTESIAN_POINT('Origin',(9.,0.,0.));
#40093=CARTESIAN_POINT('',(9.,-18.8944436276912,22.));
#40094=CARTESIAN_POINT('Ctrl Pts',(9.,-18.8944436276912,22.));
#40095=CARTESIAN_POINT('Ctrl Pts',(9.10643154142768,-18.8944436276912,22.));
#40096=CARTESIAN_POINT('Ctrl Pts',(9.22974673696054,-18.8611989035074,22.));
#40097=CARTESIAN_POINT('Ctrl Pts',(9.44255648995507,-18.7490875557919,22.));
#40098=CARTESIAN_POINT('Ctrl Pts',(9.56085821623549,-18.6399950696597,22.));
#40099=CARTESIAN_POINT('Ctrl Pts',(9.75026319887025,-18.3934680475977,22.));
#40100=CARTESIAN_POINT('Ctrl Pts',(9.84146873381169,-18.2019362155735,22.));
#40101=CARTESIAN_POINT('Ctrl Pts',(9.96320710492822,-17.8170936647807,22.));
#40102=CARTESIAN_POINT('Ctrl Pts',(10.,-17.5473641762414,22.));
#40103=CARTESIAN_POINT('Ctrl Pts',(10.,-17.3205080756888,22.));
#40104=CARTESIAN_POINT('',(9.,-18.8944436276912,-22.));
#40105=CARTESIAN_POINT('Origin',(9.,0.,0.));
#40106=CARTESIAN_POINT('Ctrl Pts',(10.,-17.3205080756888,-22.));
#40107=CARTESIAN_POINT('Ctrl Pts',(10.,-17.5473641762414,-22.));
#40108=CARTESIAN_POINT('Ctrl Pts',(9.96320710492822,-17.8170936647807,-22.));
#40109=CARTESIAN_POINT('Ctrl Pts',(9.84146873381169,-18.2019362155735,-22.));
#40110=CARTESIAN_POINT('Ctrl Pts',(9.75026319887025,-18.3934680475977,-22.));
#40111=CARTESIAN_POINT('Ctrl Pts',(9.56085821623549,-18.6399950696597,-22.));
#40112=CARTESIAN_POINT('Ctrl Pts',(9.44255648995507,-18.7490875557919,-22.));
#40113=CARTESIAN_POINT('Ctrl Pts',(9.22974673696054,-18.8611989035074,-22.));
#40114=CARTESIAN_POINT('Ctrl Pts',(9.10643154142768,-18.8944436276912,-22.));
#40115=CARTESIAN_POINT('Ctrl Pts',(9.,-18.8944436276912,-22.));
#40116=CARTESIAN_POINT('Origin',(9.,0.,0.));
#40117=CARTESIAN_POINT('',(9.,18.8944436276912,22.));
#40118=CARTESIAN_POINT('Ctrl Pts',(10.,17.3205080756888,22.));
#40119=CARTESIAN_POINT('Ctrl Pts',(10.,17.5473641762414,22.));
#40120=CARTESIAN_POINT('Ctrl Pts',(9.96320710492822,17.8170936647807,22.));
#40121=CARTESIAN_POINT('Ctrl Pts',(9.84146873381169,18.2019362155735,22.));
#40122=CARTESIAN_POINT('Ctrl Pts',(9.75026319887025,18.3934680475977,22.));
#40123=CARTESIAN_POINT('Ctrl Pts',(9.56085821623549,18.6399950696597,22.));
#40124=CARTESIAN_POINT('Ctrl Pts',(9.44255648995507,18.7490875557919,22.));
#40125=CARTESIAN_POINT('Ctrl Pts',(9.22974673696054,18.8611989035074,22.));
#40126=CARTESIAN_POINT('Ctrl Pts',(9.10643154142768,18.8944436276912,22.));
#40127=CARTESIAN_POINT('Ctrl Pts',(9.,18.8944436276912,22.));
#40128=CARTESIAN_POINT('',(9.,18.8944436276912,-22.));
#40129=CARTESIAN_POINT('Ctrl Pts',(9.,18.8944436276912,-22.));
#40130=CARTESIAN_POINT('Ctrl Pts',(9.10643154142768,18.8944436276912,-22.));
#40131=CARTESIAN_POINT('Ctrl Pts',(9.22974673696054,18.8611989035074,-22.));
#40132=CARTESIAN_POINT('Ctrl Pts',(9.44255648995507,18.7490875557919,-22.));
#40133=CARTESIAN_POINT('Ctrl Pts',(9.56085821623549,18.6399950696597,-22.));
#40134=CARTESIAN_POINT('Ctrl Pts',(9.75026319887025,18.3934680475977,-22.));
#40135=CARTESIAN_POINT('Ctrl Pts',(9.84146873381169,18.2019362155735,-22.));
#40136=CARTESIAN_POINT('Ctrl Pts',(9.96320710492822,17.8170936647807,-22.));
#40137=CARTESIAN_POINT('Ctrl Pts',(10.,17.5473641762414,-22.));
#40138=CARTESIAN_POINT('Ctrl Pts',(10.,17.3205080756888,-22.));
#40139=CARTESIAN_POINT('Origin',(9.,0.,0.));
#40140=CARTESIAN_POINT('Origin',(-43.5556221990477,0.,0.));
#40141=CARTESIAN_POINT('',(1.00000000000386,18.8944436277047,-22.));
#40142=CARTESIAN_POINT('',(-43.5556221990477,18.8944436276912,-22.));
#40143=CARTESIAN_POINT('',(1.,18.8944436276912,22.));
#40144=CARTESIAN_POINT('Origin',(1.,0.,0.));
#40145=CARTESIAN_POINT('',(-43.5556221990477,18.8944436276912,22.));
#40146=CARTESIAN_POINT('Origin',(-43.5556221990477,0.,0.));
#40147=CARTESIAN_POINT('',(1.00000000000179,-18.8944436276974,-22.));
#40148=CARTESIAN_POINT('',(-43.5556221990477,-18.8944436276912,-22.));
#40149=CARTESIAN_POINT('',(0.999999999999417,-18.8944436276931,22.));
#40150=CARTESIAN_POINT('',(-43.5556221990477,-18.8944436276912,22.));
#40151=CARTESIAN_POINT('Origin',(1.,0.,0.));
#40152=CARTESIAN_POINT('Origin',(1.,0.,0.));
#40153=CARTESIAN_POINT('',(1.73472347597681E-15,-17.3205080756888,22.));
#40154=CARTESIAN_POINT('Ctrl Pts',(-4.16333634234434E-16,-17.3205080756888,
22.));
#40155=CARTESIAN_POINT('Ctrl Pts',(-1.14358188512761E-15,-17.5473641762414,
22.));
#40156=CARTESIAN_POINT('Ctrl Pts',(0.0367928950717865,-17.8170936647807,
22.));
#40157=CARTESIAN_POINT('Ctrl Pts',(0.158531266188312,-18.2019362155735,
22.));
#40158=CARTESIAN_POINT('Ctrl Pts',(0.249736801129751,-18.3934680475977,
22.));
#40159=CARTESIAN_POINT('Ctrl Pts',(0.439141783764513,-18.6399950696597,
22.));
#40160=CARTESIAN_POINT('Ctrl Pts',(0.557443510044933,-18.7490875557919,
22.));
#40161=CARTESIAN_POINT('Ctrl Pts',(0.770253263039461,-18.8611989035074,
22.));
#40162=CARTESIAN_POINT('Ctrl Pts',(0.893568458572327,-18.8944436276912,
22.));
#40163=CARTESIAN_POINT('Ctrl Pts',(1.,-18.8944436276912,22.));
#40164=CARTESIAN_POINT('',(0.,-17.3205080756888,-22.));
#40165=CARTESIAN_POINT('Origin',(0.,0.,0.));
#40166=CARTESIAN_POINT('Ctrl Pts',(1.,-18.8944436276912,-22.));
#40167=CARTESIAN_POINT('Ctrl Pts',(0.893568458572327,-18.8944436276912,
-22.));
#40168=CARTESIAN_POINT('Ctrl Pts',(0.770253263039461,-18.8611989035074,
-22.));
#40169=CARTESIAN_POINT('Ctrl Pts',(0.557443510044933,-18.7490875557919,
-22.));
#40170=CARTESIAN_POINT('Ctrl Pts',(0.439141783764514,-18.6399950696597,
-22.));
#40171=CARTESIAN_POINT('Ctrl Pts',(0.249736801129751,-18.3934680475977,
-22.));
#40172=CARTESIAN_POINT('Ctrl Pts',(0.158531266188313,-18.2019362155735,
-22.));
#40173=CARTESIAN_POINT('Ctrl Pts',(0.0367928950717868,-17.8170936647807,
-22.));
#40174=CARTESIAN_POINT('Ctrl Pts',(-4.16333634234434E-16,-17.5473641762414,
-22.));
#40175=CARTESIAN_POINT('Ctrl Pts',(-4.16333634234434E-16,-17.3205080756888,
-22.));
#40176=CARTESIAN_POINT('Origin',(1.,0.,0.));
#40177=CARTESIAN_POINT('',(0.,17.3205080756888,22.));
#40178=CARTESIAN_POINT('Ctrl Pts',(1.,18.8944436276912,22.));
#40179=CARTESIAN_POINT('Ctrl Pts',(0.893568458572327,18.8944436276912,22.));
#40180=CARTESIAN_POINT('Ctrl Pts',(0.770253263039461,18.8611989035074,22.));
#40181=CARTESIAN_POINT('Ctrl Pts',(0.557443510044933,18.7490875557919,22.));
#40182=CARTESIAN_POINT('Ctrl Pts',(0.439141783764514,18.6399950696597,22.));
#40183=CARTESIAN_POINT('Ctrl Pts',(0.249736801129751,18.3934680475977,22.));
#40184=CARTESIAN_POINT('Ctrl Pts',(0.158531266188312,18.2019362155735,22.));
#40185=CARTESIAN_POINT('Ctrl Pts',(0.0367928950717865,17.8170936647807,
22.));
#40186=CARTESIAN_POINT('Ctrl Pts',(-4.16333634234434E-16,17.5473641762414,
22.));
#40187=CARTESIAN_POINT('Ctrl Pts',(-4.16333634234434E-16,17.3205080756888,
22.));
#40188=CARTESIAN_POINT('',(1.73472347597681E-15,17.3205080756888,-22.));
#40189=CARTESIAN_POINT('Ctrl Pts',(-4.16333634234434E-16,17.3205080756888,
-22.));
#40190=CARTESIAN_POINT('Ctrl Pts',(2.10170270214658E-16,17.5473641762414,
-22.));
#40191=CARTESIAN_POINT('Ctrl Pts',(0.0367928950717868,17.8170936647807,
-22.));
#40192=CARTESIAN_POINT('Ctrl Pts',(0.158531266188313,18.2019362155735,-22.));
#40193=CARTESIAN_POINT('Ctrl Pts',(0.249736801129751,18.3934680475977,-22.));
#40194=CARTESIAN_POINT('Ctrl Pts',(0.439141783764514,18.6399950696597,-22.));
#40195=CARTESIAN_POINT('Ctrl Pts',(0.557443510044933,18.7490875557919,-22.));
#40196=CARTESIAN_POINT('Ctrl Pts',(0.770253263039461,18.8611989035074,-22.));
#40197=CARTESIAN_POINT('Ctrl Pts',(0.893568458572327,18.8944436276912,-22.));
#40198=CARTESIAN_POINT('Ctrl Pts',(1.,18.8944436276912,-22.));
#40199=CARTESIAN_POINT('Origin',(0.,0.,0.));
#40200=CARTESIAN_POINT('Origin',(0.,18.,0.));
#40201=CARTESIAN_POINT('',(0.,18.,22.));
#40202=CARTESIAN_POINT('',(0.,18.,-22.));
#40203=CARTESIAN_POINT('Origin',(-41.,13.,0.));
#40204=CARTESIAN_POINT('Origin',(-40.5,13.,0.));
#40205=CARTESIAN_POINT('Origin',(-41.,12.75,0.));
#40206=CARTESIAN_POINT('Origin',(10.,12.75,0.));
#40207=CARTESIAN_POINT('Origin',(9.5,12.75,0.));
#40208=CARTESIAN_POINT('Origin',(1.73472347597681E-15,29.,-22.));
#40209=CARTESIAN_POINT('Origin',(1.73472347597681E-15,29.,22.));
#40210=CARTESIAN_POINT('',(0.,0.,0.));
#40211=CARTESIAN_POINT('',(475.144454419724,-2.15912705236275E-12,-1.42247325030098E-12));
#40212=CARTESIAN_POINT('',(0.,0.,0.));
#40213=CARTESIAN_POINT('',(0.,0.,0.));
#40214=CARTESIAN_POINT('Origin',(20.,28.,0.));
#40215=CARTESIAN_POINT('',(14.5,12.,-1.95943487863577E-15));
#40216=CARTESIAN_POINT('Origin',(14.5,28.,0.));
#40217=CARTESIAN_POINT('',(20.,12.,-1.95943487863577E-15));
#40218=CARTESIAN_POINT('',(20.,12.,-1.95943487863577E-15));
#40219=CARTESIAN_POINT('Origin',(20.,28.,0.));
#40220=CARTESIAN_POINT('Origin',(20.,28.,0.));
#40221=CARTESIAN_POINT('',(5.5,20.5,-9.18485099360515E-16));
#40222=CARTESIAN_POINT('Origin',(5.5,28.,0.));
#40223=CARTESIAN_POINT('',(14.5,20.5,-9.18485099360515E-16));
#40224=CARTESIAN_POINT('',(20.,20.5,-9.18485099360515E-16));
#40225=CARTESIAN_POINT('Origin',(14.5,28.,0.));
#40226=CARTESIAN_POINT('Origin',(20.,28.,0.));
#40227=CARTESIAN_POINT('',(6.66133814775094E-15,12.,-1.95943487863577E-15));
#40228=CARTESIAN_POINT('Origin',(3.46944695195361E-15,28.,0.));
#40229=CARTESIAN_POINT('',(5.50000000000001,12.,-1.95943487863577E-15));
#40230=CARTESIAN_POINT('',(20.,12.,-1.95943487863577E-15));
#40231=CARTESIAN_POINT('Origin',(5.5,28.,0.));
#40232=CARTESIAN_POINT('Origin',(10.,38.,-27.));
#40233=CARTESIAN_POINT('',(10.,31.5,-32.5));
#40234=CARTESIAN_POINT('Origin',(10.,31.5,-27.));
#40235=CARTESIAN_POINT('',(10.,38.,-32.5));
#40236=CARTESIAN_POINT('',(10.,38.,-32.5));
#40237=CARTESIAN_POINT('Origin',(10.,38.,-27.));
#40238=CARTESIAN_POINT('Origin',(10.,38.,-27.));
#40239=CARTESIAN_POINT('',(10.,0.,-30.3));
#40240=CARTESIAN_POINT('Origin',(10.,0.,-27.));
#40241=CARTESIAN_POINT('',(10.,31.5,-30.3));
#40242=CARTESIAN_POINT('',(10.,38.,-30.3));
#40243=CARTESIAN_POINT('Origin',(10.,31.5,-27.));
#40244=CARTESIAN_POINT('Origin',(10.,38.,27.));
#40245=CARTESIAN_POINT('',(9.99999999999999,31.5,21.5));
#40246=CARTESIAN_POINT('Origin',(10.,31.5,27.));
#40247=CARTESIAN_POINT('',(9.99999999999999,38.,21.5));
#40248=CARTESIAN_POINT('',(9.99999999999999,38.,21.5));
#40249=CARTESIAN_POINT('Origin',(10.,38.,27.));
#40250=CARTESIAN_POINT('Origin',(10.,38.,27.));
#40251=CARTESIAN_POINT('',(10.,0.,23.7));
#40252=CARTESIAN_POINT('Origin',(10.,0.,27.));
#40253=CARTESIAN_POINT('',(10.,31.5,23.7));
#40254=CARTESIAN_POINT('',(10.,38.,23.7));
#40255=CARTESIAN_POINT('Origin',(10.,31.5,27.));
#40256=CARTESIAN_POINT('Origin',(20.,38.,20.));
#40257=CARTESIAN_POINT('',(0.,38.,20.));
#40258=CARTESIAN_POINT('',(0.,38.,34.5));
#40259=CARTESIAN_POINT('',(0.,38.,20.));
#40260=CARTESIAN_POINT('',(20.,38.,34.5));
#40261=CARTESIAN_POINT('',(20.,38.,34.5));
#40262=CARTESIAN_POINT('',(20.,38.,20.));
#40263=CARTESIAN_POINT('',(20.,38.,20.));
#40264=CARTESIAN_POINT('',(20.,38.,20.));
#40265=CARTESIAN_POINT('Origin',(20.,38.,34.5));
#40266=CARTESIAN_POINT('',(0.,37.5,35.));
#40267=CARTESIAN_POINT('',(0.,38.,34.5));
#40268=CARTESIAN_POINT('',(20.,37.5,35.));
#40269=CARTESIAN_POINT('',(20.,37.5,35.));
#40270=CARTESIAN_POINT('',(20.,38.,34.5));
#40271=CARTESIAN_POINT('Origin',(20.,37.5,35.));
#40272=CARTESIAN_POINT('',(0.,-7.70371977754894E-31,35.));
#40273=CARTESIAN_POINT('',(0.,37.5,35.));
#40274=CARTESIAN_POINT('',(20.,-7.70371977754894E-31,35.));
#40275=CARTESIAN_POINT('',(20.,-7.70371977754894E-31,35.));
#40276=CARTESIAN_POINT('',(20.,37.5,35.));
#40277=CARTESIAN_POINT('Origin',(20.,-7.70371977754894E-31,35.));
#40278=CARTESIAN_POINT('',(0.,2.17954046104435E-14,-35.));
#40279=CARTESIAN_POINT('',(0.,-7.70371977754894E-31,35.));
#40280=CARTESIAN_POINT('',(20.,2.17954046104435E-14,-35.));
#40281=CARTESIAN_POINT('',(20.,2.17954046104435E-14,-35.));
#40282=CARTESIAN_POINT('',(20.,-7.70371977754894E-31,35.));
#40283=CARTESIAN_POINT('Origin',(20.,37.5,-35.));
#40284=CARTESIAN_POINT('',(0.,37.5,-35.));
#40285=CARTESIAN_POINT('',(0.,37.5,-35.));
#40286=CARTESIAN_POINT('',(20.,37.5,-35.));
#40287=CARTESIAN_POINT('',(20.,37.5,-35.));
#40288=CARTESIAN_POINT('',(20.,37.5,-35.));
#40289=CARTESIAN_POINT('Origin',(20.,38.,-34.5));
#40290=CARTESIAN_POINT('',(0.,38.,-34.5));
#40291=CARTESIAN_POINT('',(0.,38.,-34.5));
#40292=CARTESIAN_POINT('',(20.,38.,-34.5));
#40293=CARTESIAN_POINT('',(20.,38.,-34.5));
#40294=CARTESIAN_POINT('',(20.,38.,-34.5));
#40295=CARTESIAN_POINT('Origin',(20.,38.,-20.));
#40296=CARTESIAN_POINT('',(0.,38.,-20.));
#40297=CARTESIAN_POINT('',(0.,38.,-20.));
#40298=CARTESIAN_POINT('',(20.,38.,-20.));
#40299=CARTESIAN_POINT('',(20.,38.,-20.));
#40300=CARTESIAN_POINT('',(20.,38.,-20.));
#40301=CARTESIAN_POINT('Origin',(20.,47.5,-20.));
#40302=CARTESIAN_POINT('',(0.,47.5,-20.));
#40303=CARTESIAN_POINT('',(0.,47.5,-20.));
#40304=CARTESIAN_POINT('',(20.,47.5,-20.));
#40305=CARTESIAN_POINT('',(20.,47.5,-20.));
#40306=CARTESIAN_POINT('',(20.,47.5,-20.));
#40307=CARTESIAN_POINT('Origin',(20.,48.,-19.5));
#40308=CARTESIAN_POINT('',(0.,48.,-19.5));
#40309=CARTESIAN_POINT('',(0.,48.,-19.5));
#40310=CARTESIAN_POINT('',(20.,48.,-19.5));
#40311=CARTESIAN_POINT('',(20.,48.,-19.5));
#40312=CARTESIAN_POINT('',(20.,48.,-19.5));
#40313=CARTESIAN_POINT('Origin',(20.,48.,19.5));
#40314=CARTESIAN_POINT('',(0.,48.,19.5));
#40315=CARTESIAN_POINT('',(0.,48.,19.5));
#40316=CARTESIAN_POINT('',(20.,48.,19.5));
#40317=CARTESIAN_POINT('',(20.,48.,19.5));
#40318=CARTESIAN_POINT('',(20.,48.,19.5));
#40319=CARTESIAN_POINT('Origin',(20.,47.5,20.));
#40320=CARTESIAN_POINT('',(0.,47.5,20.));
#40321=CARTESIAN_POINT('',(0.,47.5,20.));
#40322=CARTESIAN_POINT('',(20.,47.5,20.));
#40323=CARTESIAN_POINT('',(20.,47.5,20.));
#40324=CARTESIAN_POINT('',(20.,47.5,20.));
#40325=CARTESIAN_POINT('Origin',(20.,47.5,20.));
#40326=CARTESIAN_POINT('',(0.,47.5,20.));
#40327=CARTESIAN_POINT('',(20.,47.5,20.));
#40328=CARTESIAN_POINT('Origin',(20.,0.,0.));
#40329=CARTESIAN_POINT('Origin',(0.,0.,0.));
#40330=CARTESIAN_POINT('Origin',(13.3,31.5,27.));
#40331=CARTESIAN_POINT('Origin',(13.3,31.5,-27.));
#40332=CARTESIAN_POINT('Origin',(5.5,44.,0.));
#40333=CARTESIAN_POINT('Origin',(14.5,35.5,0.));
#40334=CARTESIAN_POINT('',(0.,0.,0.));
#40335=CARTESIAN_POINT('Origin',(1.,-9.3,2.45));
#40336=CARTESIAN_POINT('',(1.,-9.3,1.6));
#40337=CARTESIAN_POINT('Origin',(1.,-9.3,2.45));
#40338=CARTESIAN_POINT('',(0.,-9.3,1.6));
#40339=CARTESIAN_POINT('',(1.,-9.3,1.6));
#40340=CARTESIAN_POINT('Origin',(0.,-9.3,2.45));
#40341=CARTESIAN_POINT('Origin',(1.,-9.3,-2.45));
#40342=CARTESIAN_POINT('',(1.,-9.3,-3.3));
#40343=CARTESIAN_POINT('Origin',(1.,-9.3,-2.45));
#40344=CARTESIAN_POINT('',(0.,-9.3,-3.3));
#40345=CARTESIAN_POINT('',(1.,-9.3,-3.3));
#40346=CARTESIAN_POINT('Origin',(0.,-9.3,-2.45));
#40347=CARTESIAN_POINT('Origin',(1.,-0.55,0.));
#40348=CARTESIAN_POINT('',(1.,-7.68249605678125,0.499999999999999));
#40349=CARTESIAN_POINT('',(1.,-7.68249605678125,-0.5));
#40350=CARTESIAN_POINT('Origin',(1.,-0.55,0.));
#40351=CARTESIAN_POINT('',(0.,-7.68249605678125,0.499999999999999));
#40352=CARTESIAN_POINT('',(1.,-7.68249605678125,0.499999999999999));
#40353=CARTESIAN_POINT('',(0.,-7.68249605678125,-0.5));
#40354=CARTESIAN_POINT('Origin',(0.,-0.55,0.));
#40355=CARTESIAN_POINT('',(1.,-7.68249605678125,-0.5));
#40356=CARTESIAN_POINT('Origin',(1.,2.60208521396521E-15,2.71050543121376E-16));
#40357=CARTESIAN_POINT('',(1.,-7.14272206303279,-5.14018691588785));
#40358=CARTESIAN_POINT('',(1.,-7.14272206303279,5.14018691588785));
#40359=CARTESIAN_POINT('Origin',(1.,2.60208521396521E-15,2.71050543121376E-16));
#40360=CARTESIAN_POINT('',(0.,-7.14272206303279,-5.14018691588785));
#40361=CARTESIAN_POINT('',(1.,-7.14272206303279,-5.14018691588785));
#40362=CARTESIAN_POINT('',(0.,-7.14272206303279,5.14018691588785));
#40363=CARTESIAN_POINT('Origin',(0.,2.60208521396521E-15,2.71050543121376E-16));
#40364=CARTESIAN_POINT('',(1.,-7.14272206303279,5.14018691588785));
#40365=CARTESIAN_POINT('Origin',(1.,-0.55,0.));
#40366=CARTESIAN_POINT('',(1.,-11.2,-0.500000000000001));
#40367=CARTESIAN_POINT('',(1.,-11.2,-2.45));
#40368=CARTESIAN_POINT('',(1.,-11.2,-2.45));
#40369=CARTESIAN_POINT('',(1.,-9.3,-4.35));
#40370=CARTESIAN_POINT('Origin',(1.,-9.3,-2.45));
#40371=CARTESIAN_POINT('',(1.,-8.6849006902785,-4.35));
#40372=CARTESIAN_POINT('',(1.,-8.6849006902785,-4.35));
#40373=CARTESIAN_POINT('Origin',(1.,-8.6849006902785,-6.25));
#40374=CARTESIAN_POINT('',(1.,-8.6849006902785,4.35));
#40375=CARTESIAN_POINT('Origin',(1.,-8.6849006902785,6.25));
#40376=CARTESIAN_POINT('',(1.,-9.3,4.35));
#40377=CARTESIAN_POINT('',(1.,-8.6849006902785,4.35));
#40378=CARTESIAN_POINT('',(1.,-11.2,2.45));
#40379=CARTESIAN_POINT('Origin',(1.,-9.3,2.45));
#40380=CARTESIAN_POINT('',(1.,-11.2,0.500000000000001));
#40381=CARTESIAN_POINT('',(1.,-11.2,2.45));
#40382=CARTESIAN_POINT('',(1.,-7.68249605678125,0.5));
#40383=CARTESIAN_POINT('',(1.,-7.68249605678125,-0.5));
#40384=CARTESIAN_POINT('Origin',(0.,-0.55,0.));
#40385=CARTESIAN_POINT('',(0.,-11.2,-0.500000000000001));
#40386=CARTESIAN_POINT('',(0.,-11.2,-2.45));
#40387=CARTESIAN_POINT('',(0.,-11.2,-2.45));
#40388=CARTESIAN_POINT('',(0.,-7.68249605678125,-0.5));
#40389=CARTESIAN_POINT('',(0.,-11.2,0.500000000000001));
#40390=CARTESIAN_POINT('',(0.,-7.68249605678125,0.5));
#40391=CARTESIAN_POINT('',(0.,-11.2,2.45));
#40392=CARTESIAN_POINT('',(0.,-11.2,2.45));
#40393=CARTESIAN_POINT('',(0.,-9.3,4.35));
#40394=CARTESIAN_POINT('Origin',(0.,-9.3,2.45));
#40395=CARTESIAN_POINT('',(0.,-8.6849006902785,4.35));
#40396=CARTESIAN_POINT('',(0.,-8.6849006902785,4.35));
#40397=CARTESIAN_POINT('Origin',(0.,-8.6849006902785,6.25));
#40398=CARTESIAN_POINT('',(0.,-8.6849006902785,-4.35));
#40399=CARTESIAN_POINT('Origin',(0.,-8.6849006902785,-6.25));
#40400=CARTESIAN_POINT('',(0.,-9.3,-4.35));
#40401=CARTESIAN_POINT('',(0.,-8.6849006902785,-4.35));
#40402=CARTESIAN_POINT('Origin',(0.,-9.3,-2.45));
#40403=CARTESIAN_POINT('Origin',(1.,-11.2,-2.45));
#40404=CARTESIAN_POINT('',(1.,-11.2,-2.45));
#40405=CARTESIAN_POINT('',(1.,-11.2,-0.500000000000001));
#40406=CARTESIAN_POINT('Origin',(1.,-9.3,-2.45));
#40407=CARTESIAN_POINT('',(1.,-9.3,-4.35));
#40408=CARTESIAN_POINT('Origin',(1.,-8.6849006902785,-4.35));
#40409=CARTESIAN_POINT('',(1.,-8.6849006902785,-4.35));
#40410=CARTESIAN_POINT('Origin',(1.,-8.6849006902785,-6.25));
#40411=CARTESIAN_POINT('Origin',(1.,-8.6849006902785,6.25));
#40412=CARTESIAN_POINT('',(1.,-8.6849006902785,4.35));
#40413=CARTESIAN_POINT('Origin',(1.,-8.6849006902785,4.35));
#40414=CARTESIAN_POINT('',(1.,-9.3,4.35));
#40415=CARTESIAN_POINT('Origin',(1.,-9.3,2.45));
#40416=CARTESIAN_POINT('',(1.,-11.2,2.45));
#40417=CARTESIAN_POINT('Origin',(1.,-11.2,2.45));
#40418=CARTESIAN_POINT('',(1.,-11.2,0.500000000000001));
#40419=CARTESIAN_POINT('Origin',(1.,-7.68249605678125,0.5));
#40420=CARTESIAN_POINT('Origin',(1.,-7.68249605678125,-0.5));
#40421=CARTESIAN_POINT('',(0.,0.,0.));
#40422=CARTESIAN_POINT('',(5.50000000000001,28.55,-7.49263314916189E-16));
#40423=CARTESIAN_POINT('',(0.,0.,0.));
#40424=CARTESIAN_POINT('',(0.,0.,0.));
#40425=CARTESIAN_POINT('Origin',(33.,28.,0.));
#40426=CARTESIAN_POINT('',(27.,28.,14.));
#40427=CARTESIAN_POINT('Origin',(27.,28.,0.));
#40428=CARTESIAN_POINT('',(33.,28.,14.));
#40429=CARTESIAN_POINT('',(33.,28.,14.));
#40430=CARTESIAN_POINT('Origin',(33.,28.,0.));
#40431=CARTESIAN_POINT('Origin',(33.,28.,0.));
#40432=CARTESIAN_POINT('',(24.,28.,9.75));
#40433=CARTESIAN_POINT('Origin',(24.,28.,0.));
#40434=CARTESIAN_POINT('',(27.,28.,9.75));
#40435=CARTESIAN_POINT('',(33.,28.,9.75));
#40436=CARTESIAN_POINT('Origin',(27.,28.,0.));
#40437=CARTESIAN_POINT('Origin',(33.,28.,0.));
#40438=CARTESIAN_POINT('',(6.,28.,7.5));
#40439=CARTESIAN_POINT('Origin',(6.,28.,0.));
#40440=CARTESIAN_POINT('',(24.,28.,7.5));
#40441=CARTESIAN_POINT('',(33.,28.,7.5));
#40442=CARTESIAN_POINT('Origin',(24.,28.,0.));
#40443=CARTESIAN_POINT('Origin',(33.,28.,0.));
#40444=CARTESIAN_POINT('',(2.,28.,9.75));
#40445=CARTESIAN_POINT('Origin',(2.,28.,0.));
#40446=CARTESIAN_POINT('',(6.,28.,9.75));
#40447=CARTESIAN_POINT('',(33.,28.,9.75));
#40448=CARTESIAN_POINT('Origin',(6.,28.,0.));
#40449=CARTESIAN_POINT('Origin',(33.,28.,0.));
#40450=CARTESIAN_POINT('',(0.,28.,14.));
#40451=CARTESIAN_POINT('Origin',(0.,28.,0.));
#40452=CARTESIAN_POINT('',(2.,28.,14.));
#40453=CARTESIAN_POINT('',(33.,28.,14.));
#40454=CARTESIAN_POINT('Origin',(2.,28.,0.));
#40455=CARTESIAN_POINT('Origin',(33.,14.2114177668623,13.7885822331377));
#40456=CARTESIAN_POINT('',(27.,14.2114177668623,10.6885822331377));
#40457=CARTESIAN_POINT('Origin',(27.,14.2114177668623,13.7885822331377));
#40458=CARTESIAN_POINT('',(33.,14.2114177668623,10.6885822331377));
#40459=CARTESIAN_POINT('',(33.,14.2114177668623,10.6885822331377));
#40460=CARTESIAN_POINT('Origin',(33.,14.2114177668623,13.7885822331377));
#40461=CARTESIAN_POINT('Origin',(33.,14.2114177668623,-13.7885822331377));
#40462=CARTESIAN_POINT('',(27.,14.2114177668623,-16.8885822331377));
#40463=CARTESIAN_POINT('Origin',(27.,14.2114177668623,-13.7885822331377));
#40464=CARTESIAN_POINT('',(33.,14.2114177668623,-16.8885822331377));
#40465=CARTESIAN_POINT('',(33.,14.2114177668623,-16.8885822331377));
#40466=CARTESIAN_POINT('Origin',(33.,14.2114177668623,-13.7885822331377));
#40467=CARTESIAN_POINT('Origin',(33.,41.7885822331377,-13.7885822331377));
#40468=CARTESIAN_POINT('',(27.,41.7885822331377,-16.8885822331377));
#40469=CARTESIAN_POINT('Origin',(27.,41.7885822331377,-13.7885822331377));
#40470=CARTESIAN_POINT('',(33.,41.7885822331377,-16.8885822331377));
#40471=CARTESIAN_POINT('',(33.,41.7885822331377,-16.8885822331377));
#40472=CARTESIAN_POINT('Origin',(33.,41.7885822331377,-13.7885822331377));
#40473=CARTESIAN_POINT('Origin',(33.,41.7885822331377,13.7885822331377));
#40474=CARTESIAN_POINT('',(27.,41.7885822331377,10.6885822331377));
#40475=CARTESIAN_POINT('Origin',(27.,41.7885822331377,13.7885822331377));
#40476=CARTESIAN_POINT('',(33.,41.7885822331377,10.6885822331377));
#40477=CARTESIAN_POINT('',(33.,41.7885822331377,10.6885822331377));
#40478=CARTESIAN_POINT('Origin',(33.,41.7885822331377,13.7885822331377));
#40479=CARTESIAN_POINT('Origin',(33.,14.2114177668623,-13.7885822331377));
#40480=CARTESIAN_POINT('',(33.,14.2114177668623,-17.2885822331377));
#40481=CARTESIAN_POINT('Origin',(33.,14.2114177668623,-13.7885822331377));
#40482=CARTESIAN_POINT('',(27.,14.2114177668623,-17.2885822331377));
#40483=CARTESIAN_POINT('',(33.,14.2114177668623,-17.2885822331377));
#40484=CARTESIAN_POINT('Origin',(27.,14.2114177668623,-13.7885822331377));
#40485=CARTESIAN_POINT('Origin',(33.,14.2114177668623,13.7885822331377));
#40486=CARTESIAN_POINT('',(33.,14.2114177668623,10.2885822331377));
#40487=CARTESIAN_POINT('Origin',(33.,14.2114177668623,13.7885822331377));
#40488=CARTESIAN_POINT('',(27.,14.2114177668623,10.2885822331377));
#40489=CARTESIAN_POINT('',(33.,14.2114177668623,10.2885822331377));
#40490=CARTESIAN_POINT('Origin',(27.,14.2114177668623,13.7885822331377));
#40491=CARTESIAN_POINT('Origin',(33.,41.7885822331377,-13.7885822331377));
#40492=CARTESIAN_POINT('',(33.,41.7885822331377,-17.2885822331377));
#40493=CARTESIAN_POINT('Origin',(33.,41.7885822331377,-13.7885822331377));
#40494=CARTESIAN_POINT('',(27.,41.7885822331377,-17.2885822331377));
#40495=CARTESIAN_POINT('',(33.,41.7885822331377,-17.2885822331377));
#40496=CARTESIAN_POINT('Origin',(27.,41.7885822331377,-13.7885822331377));
#40497=CARTESIAN_POINT('Origin',(33.,41.7885822331377,13.7885822331377));
#40498=CARTESIAN_POINT('',(33.,41.7885822331377,10.2885822331377));
#40499=CARTESIAN_POINT('Origin',(33.,41.7885822331377,13.7885822331377));
#40500=CARTESIAN_POINT('',(27.,41.7885822331377,10.2885822331377));
#40501=CARTESIAN_POINT('',(33.,41.7885822331377,10.2885822331377));
#40502=CARTESIAN_POINT('Origin',(27.,41.7885822331377,13.7885822331377));
#40503=CARTESIAN_POINT('Origin',(6.,38.,-27.));
#40504=CARTESIAN_POINT('',(5.99999999999999,31.5,-32.5));
#40505=CARTESIAN_POINT('Origin',(6.,31.5,-27.));
#40506=CARTESIAN_POINT('',(5.99999999999999,38.,-32.5));
#40507=CARTESIAN_POINT('',(5.99999999999999,38.,-32.5));
#40508=CARTESIAN_POINT('Origin',(6.,38.,-27.));
#40509=CARTESIAN_POINT('Origin',(6.,38.,-27.));
#40510=CARTESIAN_POINT('',(6.,0.,-30.3));
#40511=CARTESIAN_POINT('Origin',(6.,0.,-27.));
#40512=CARTESIAN_POINT('',(6.,31.5,-30.3));
#40513=CARTESIAN_POINT('',(6.,38.,-30.3));
#40514=CARTESIAN_POINT('Origin',(6.,31.5,-27.));
#40515=CARTESIAN_POINT('Origin',(6.,38.,27.));
#40516=CARTESIAN_POINT('',(5.99999999999999,31.5,21.5));
#40517=CARTESIAN_POINT('Origin',(6.,31.5,27.));
#40518=CARTESIAN_POINT('',(5.99999999999999,38.,21.5));
#40519=CARTESIAN_POINT('',(5.99999999999999,38.,21.5));
#40520=CARTESIAN_POINT('Origin',(6.,38.,27.));
#40521=CARTESIAN_POINT('Origin',(6.,38.,27.));
#40522=CARTESIAN_POINT('',(6.,0.,23.7));
#40523=CARTESIAN_POINT('Origin',(6.,0.,27.));
#40524=CARTESIAN_POINT('',(6.,31.5,23.7));
#40525=CARTESIAN_POINT('',(6.,38.,23.7));
#40526=CARTESIAN_POINT('Origin',(6.,31.5,27.));
#40527=CARTESIAN_POINT('Origin',(21.,38.,-27.));
#40528=CARTESIAN_POINT('',(21.,31.5,-32.5));
#40529=CARTESIAN_POINT('Origin',(21.,31.5,-27.));
#40530=CARTESIAN_POINT('',(21.,38.,-32.5));
#40531=CARTESIAN_POINT('',(21.,38.,-32.5));
#40532=CARTESIAN_POINT('Origin',(21.,38.,-27.));
#40533=CARTESIAN_POINT('Origin',(21.,38.,-27.));
#40534=CARTESIAN_POINT('',(21.,0.,-30.3));
#40535=CARTESIAN_POINT('Origin',(21.,0.,-27.));
#40536=CARTESIAN_POINT('',(21.,31.5,-30.3));
#40537=CARTESIAN_POINT('',(21.,38.,-30.3));
#40538=CARTESIAN_POINT('Origin',(21.,31.5,-27.));
#40539=CARTESIAN_POINT('Origin',(21.,38.,27.));
#40540=CARTESIAN_POINT('',(21.,31.5,21.5));
#40541=CARTESIAN_POINT('Origin',(21.,31.5,27.));
#40542=CARTESIAN_POINT('',(21.,38.,21.5));
#40543=CARTESIAN_POINT('',(21.,38.,21.5));
#40544=CARTESIAN_POINT('Origin',(21.,38.,27.));
#40545=CARTESIAN_POINT('Origin',(21.,38.,27.));
#40546=CARTESIAN_POINT('',(21.,0.,23.7));
#40547=CARTESIAN_POINT('Origin',(21.,0.,27.));
#40548=CARTESIAN_POINT('',(21.,31.5,23.7));
#40549=CARTESIAN_POINT('',(21.,38.,23.7));
#40550=CARTESIAN_POINT('Origin',(21.,31.5,27.));
#40551=CARTESIAN_POINT('Origin',(27.,0.,0.));
#40552=CARTESIAN_POINT('Origin',(27.,0.,0.));
#40553=CARTESIAN_POINT('Origin',(27.,0.,0.));
#40554=CARTESIAN_POINT('Origin',(27.,0.,0.));
#40555=CARTESIAN_POINT('Origin',(27.,0.,0.));
#40556=CARTESIAN_POINT('',(27.,38.,20.));
#40557=CARTESIAN_POINT('',(27.,38.,34.5));
#40558=CARTESIAN_POINT('',(27.,38.,20.));
#40559=CARTESIAN_POINT('',(27.,37.5,35.));
#40560=CARTESIAN_POINT('',(27.,38.,34.5));
#40561=CARTESIAN_POINT('',(27.,0.,35.));
#40562=CARTESIAN_POINT('',(27.,37.5,35.));
#40563=CARTESIAN_POINT('',(27.,1.53660089149199E-14,-35.));
#40564=CARTESIAN_POINT('',(27.,0.,35.));
#40565=CARTESIAN_POINT('',(27.,37.5,-35.));
#40566=CARTESIAN_POINT('',(27.,37.5,-35.));
#40567=CARTESIAN_POINT('',(27.,38.,-34.5));
#40568=CARTESIAN_POINT('',(27.,38.,-34.5));
#40569=CARTESIAN_POINT('',(27.,38.,-20.));
#40570=CARTESIAN_POINT('',(27.,38.,-20.));
#40571=CARTESIAN_POINT('',(27.,47.5,-20.));
#40572=CARTESIAN_POINT('',(27.,47.5,-20.));
#40573=CARTESIAN_POINT('',(27.,48.,-19.5));
#40574=CARTESIAN_POINT('',(27.,48.,-19.5));
#40575=CARTESIAN_POINT('',(27.,48.,19.5));
#40576=CARTESIAN_POINT('',(27.,48.,19.5));
#40577=CARTESIAN_POINT('',(27.,47.5,20.));
#40578=CARTESIAN_POINT('',(27.,47.5,20.));
#40579=CARTESIAN_POINT('',(27.,47.5,20.));
#40580=CARTESIAN_POINT('',(27.,47.,17.));
#40581=CARTESIAN_POINT('',(27.,45.,19.));
#40582=CARTESIAN_POINT('',(27.,45.,19.));
#40583=CARTESIAN_POINT('',(27.,47.,-17.));
#40584=CARTESIAN_POINT('',(27.,47.,17.));
#40585=CARTESIAN_POINT('',(27.,45.,-19.));
#40586=CARTESIAN_POINT('',(27.,47.,-17.));
#40587=CARTESIAN_POINT('',(27.,11.,-19.));
#40588=CARTESIAN_POINT('',(27.,45.,-19.));
#40589=CARTESIAN_POINT('',(27.,9.,-17.));
#40590=CARTESIAN_POINT('',(27.,11.,-19.));
#40591=CARTESIAN_POINT('',(27.,9.,17.));
#40592=CARTESIAN_POINT('',(27.,9.,17.));
#40593=CARTESIAN_POINT('',(27.,11.,19.));
#40594=CARTESIAN_POINT('',(27.,11.,19.));
#40595=CARTESIAN_POINT('',(27.,45.,19.));
#40596=CARTESIAN_POINT('Origin',(27.,38.,20.));
#40597=CARTESIAN_POINT('',(0.,38.,20.));
#40598=CARTESIAN_POINT('',(0.,38.,34.5));
#40599=CARTESIAN_POINT('',(0.,38.,20.));
#40600=CARTESIAN_POINT('',(27.,38.,34.5));
#40601=CARTESIAN_POINT('',(27.,38.,20.));
#40602=CARTESIAN_POINT('Origin',(27.,38.,34.5));
#40603=CARTESIAN_POINT('',(0.,37.5,35.));
#40604=CARTESIAN_POINT('',(0.,38.,34.5));
#40605=CARTESIAN_POINT('',(27.,37.5,35.));
#40606=CARTESIAN_POINT('Origin',(27.,37.5,35.));
#40607=CARTESIAN_POINT('',(0.,0.,35.));
#40608=CARTESIAN_POINT('',(0.,37.5,35.));
#40609=CARTESIAN_POINT('',(27.,0.,35.));
#40610=CARTESIAN_POINT('Origin',(27.,0.,35.));
#40611=CARTESIAN_POINT('',(0.,1.53660089149199E-14,-35.));
#40612=CARTESIAN_POINT('',(0.,0.,35.));
#40613=CARTESIAN_POINT('',(27.,1.53660089149199E-14,-35.));
#40614=CARTESIAN_POINT('Origin',(27.,37.5,-35.));
#40615=CARTESIAN_POINT('',(0.,37.5,-35.));
#40616=CARTESIAN_POINT('',(0.,37.5,-35.));
#40617=CARTESIAN_POINT('',(27.,37.5,-35.));
#40618=CARTESIAN_POINT('Origin',(27.,38.,-34.5));
#40619=CARTESIAN_POINT('',(0.,38.,-34.5));
#40620=CARTESIAN_POINT('',(0.,38.,-34.5));
#40621=CARTESIAN_POINT('',(27.,38.,-34.5));
#40622=CARTESIAN_POINT('Origin',(27.,38.,-20.));
#40623=CARTESIAN_POINT('',(0.,38.,-20.));
#40624=CARTESIAN_POINT('',(0.,38.,-20.));
#40625=CARTESIAN_POINT('',(27.,38.,-20.));
#40626=CARTESIAN_POINT('Origin',(27.,47.5,-20.));
#40627=CARTESIAN_POINT('',(0.,47.5,-20.));
#40628=CARTESIAN_POINT('',(0.,47.5,-20.));
#40629=CARTESIAN_POINT('',(27.,47.5,-20.));
#40630=CARTESIAN_POINT('Origin',(27.,48.,-19.5));
#40631=CARTESIAN_POINT('',(0.,48.,-19.5));
#40632=CARTESIAN_POINT('',(0.,48.,-19.5));
#40633=CARTESIAN_POINT('',(27.,48.,-19.5));
#40634=CARTESIAN_POINT('Origin',(27.,48.,19.5));
#40635=CARTESIAN_POINT('',(0.,48.,19.5));
#40636=CARTESIAN_POINT('',(0.,48.,19.5));
#40637=CARTESIAN_POINT('',(27.,48.,19.5));
#40638=CARTESIAN_POINT('Origin',(27.,47.5,20.));
#40639=CARTESIAN_POINT('',(0.,47.5,20.));
#40640=CARTESIAN_POINT('',(0.,47.5,20.));
#40641=CARTESIAN_POINT('',(27.,47.5,20.));
#40642=CARTESIAN_POINT('Origin',(27.,47.5,20.));
#40643=CARTESIAN_POINT('',(0.,47.5,20.));
#40644=CARTESIAN_POINT('Origin',(0.,0.,0.));
#40645=CARTESIAN_POINT('Origin',(24.3,31.5,27.));
#40646=CARTESIAN_POINT('Origin',(24.3,31.5,-27.));
#40647=CARTESIAN_POINT('Origin',(9.3,31.5,27.));
#40648=CARTESIAN_POINT('Origin',(9.3,31.5,-27.));
#40649=CARTESIAN_POINT('Origin',(33.,0.,0.));
#40650=CARTESIAN_POINT('',(33.,47.,-17.));
#40651=CARTESIAN_POINT('',(33.,47.,17.));
#40652=CARTESIAN_POINT('',(33.,47.,17.));
#40653=CARTESIAN_POINT('',(33.,45.,19.));
#40654=CARTESIAN_POINT('',(33.,45.,19.));
#40655=CARTESIAN_POINT('',(33.,11.,19.));
#40656=CARTESIAN_POINT('',(33.,45.,19.));
#40657=CARTESIAN_POINT('',(33.,9.,17.));
#40658=CARTESIAN_POINT('',(33.,11.,19.));
#40659=CARTESIAN_POINT('',(33.,9.,-17.));
#40660=CARTESIAN_POINT('',(33.,9.,17.));
#40661=CARTESIAN_POINT('',(33.,11.,-19.));
#40662=CARTESIAN_POINT('',(33.,11.,-19.));
#40663=CARTESIAN_POINT('',(33.,45.,-19.));
#40664=CARTESIAN_POINT('',(33.,45.,-19.));
#40665=CARTESIAN_POINT('',(33.,47.,-17.));
#40666=CARTESIAN_POINT('Origin',(33.,47.,17.));
#40667=CARTESIAN_POINT('',(33.,47.,17.));
#40668=CARTESIAN_POINT('',(33.,47.,-17.));
#40669=CARTESIAN_POINT('Origin',(33.,45.,19.));
#40670=CARTESIAN_POINT('',(33.,45.,19.));
#40671=CARTESIAN_POINT('Origin',(33.,45.,19.));
#40672=CARTESIAN_POINT('',(33.,11.,19.));
#40673=CARTESIAN_POINT('Origin',(33.,11.,19.));
#40674=CARTESIAN_POINT('',(33.,9.,17.));
#40675=CARTESIAN_POINT('Origin',(33.,9.,17.));
#40676=CARTESIAN_POINT('',(33.,9.,-17.));
#40677=CARTESIAN_POINT('Origin',(33.,11.,-19.));
#40678=CARTESIAN_POINT('',(33.,11.,-19.));
#40679=CARTESIAN_POINT('Origin',(33.,45.,-19.));
#40680=CARTESIAN_POINT('',(33.,45.,-19.));
#40681=CARTESIAN_POINT('Origin',(33.,47.,-17.));
#40682=CARTESIAN_POINT('Origin',(33.,41.7885822331377,13.7885822331377));
#40683=CARTESIAN_POINT('',(33.,40.0565314255688,13.7885822331377));
#40684=CARTESIAN_POINT('',(33.,40.9225568293532,12.2885822331377));
#40685=CARTESIAN_POINT('',(33.,40.0565314255688,13.7885822331377));
#40686=CARTESIAN_POINT('',(33.,40.9225568293533,15.2885822331377));
#40687=CARTESIAN_POINT('',(33.,40.9225568293533,15.2885822331377));
#40688=CARTESIAN_POINT('',(33.,42.6546076369221,15.2885822331377));
#40689=CARTESIAN_POINT('',(33.,42.6546076369221,15.2885822331377));
#40690=CARTESIAN_POINT('',(33.,43.5206330407066,13.7885822331377));
#40691=CARTESIAN_POINT('',(33.,43.5206330407066,13.7885822331377));
#40692=CARTESIAN_POINT('',(33.,42.6546076369221,12.2885822331377));
#40693=CARTESIAN_POINT('',(33.,42.6546076369221,12.2885822331377));
#40694=CARTESIAN_POINT('',(33.,40.9225568293532,12.2885822331377));
#40695=CARTESIAN_POINT('Origin',(33.,41.7885822331377,-13.7885822331377));
#40696=CARTESIAN_POINT('',(33.,40.0565314255688,-13.7885822331377));
#40697=CARTESIAN_POINT('',(33.,40.9225568293532,-15.2885822331377));
#40698=CARTESIAN_POINT('',(33.,40.0565314255688,-13.7885822331377));
#40699=CARTESIAN_POINT('',(33.,40.9225568293532,-12.2885822331377));
#40700=CARTESIAN_POINT('',(33.,40.9225568293532,-12.2885822331377));
#40701=CARTESIAN_POINT('',(33.,42.6546076369221,-12.2885822331377));
#40702=CARTESIAN_POINT('',(33.,42.6546076369221,-12.2885822331377));
#40703=CARTESIAN_POINT('',(33.,43.5206330407065,-13.7885822331377));
#40704=CARTESIAN_POINT('',(33.,43.5206330407065,-13.7885822331377));
#40705=CARTESIAN_POINT('',(33.,42.6546076369221,-15.2885822331377));
#40706=CARTESIAN_POINT('',(33.,42.6546076369221,-15.2885822331377));
#40707=CARTESIAN_POINT('',(33.,40.9225568293532,-15.2885822331377));
#40708=CARTESIAN_POINT('Origin',(33.,14.2114177668623,-13.7885822331377));
#40709=CARTESIAN_POINT('',(33.,12.4793669592934,-13.7885822331377));
#40710=CARTESIAN_POINT('',(33.,13.3453923630779,-15.2885822331377));
#40711=CARTESIAN_POINT('',(33.,12.4793669592934,-13.7885822331377));
#40712=CARTESIAN_POINT('',(33.,13.3453923630779,-12.2885822331377));
#40713=CARTESIAN_POINT('',(33.,13.3453923630779,-12.2885822331377));
#40714=CARTESIAN_POINT('',(33.,15.0774431706468,-12.2885822331377));
#40715=CARTESIAN_POINT('',(33.,15.0774431706468,-12.2885822331377));
#40716=CARTESIAN_POINT('',(33.,15.9434685744312,-13.7885822331377));
#40717=CARTESIAN_POINT('',(33.,15.9434685744312,-13.7885822331377));
#40718=CARTESIAN_POINT('',(33.,15.0774431706468,-15.2885822331377));
#40719=CARTESIAN_POINT('',(33.,15.0774431706468,-15.2885822331377));
#40720=CARTESIAN_POINT('',(33.,13.3453923630779,-15.2885822331377));
#40721=CARTESIAN_POINT('Origin',(33.,14.2114177668623,13.7885822331377));
#40722=CARTESIAN_POINT('',(33.,12.4793669592934,13.7885822331377));
#40723=CARTESIAN_POINT('',(33.,13.3453923630779,12.2885822331377));
#40724=CARTESIAN_POINT('',(33.,12.4793669592934,13.7885822331377));
#40725=CARTESIAN_POINT('',(33.,13.3453923630779,15.2885822331377));
#40726=CARTESIAN_POINT('',(33.,13.3453923630779,15.2885822331377));
#40727=CARTESIAN_POINT('',(33.,15.0774431706468,15.2885822331377));
#40728=CARTESIAN_POINT('',(33.,15.0774431706468,15.2885822331377));
#40729=CARTESIAN_POINT('',(33.,15.9434685744312,13.7885822331377));
#40730=CARTESIAN_POINT('',(33.,15.9434685744312,13.7885822331377));
#40731=CARTESIAN_POINT('',(33.,15.0774431706468,12.2885822331377));
#40732=CARTESIAN_POINT('',(33.,15.0774431706468,12.2885822331377));
#40733=CARTESIAN_POINT('',(33.,13.3453923630779,12.2885822331377));
#40734=CARTESIAN_POINT('Origin',(30.,40.0565314255688,13.7885822331377));
#40735=CARTESIAN_POINT('',(30.,40.9225568293532,12.2885822331377));
#40736=CARTESIAN_POINT('',(30.,40.9225568293532,12.2885822331377));
#40737=CARTESIAN_POINT('',(30.,40.0565314255688,13.7885822331377));
#40738=CARTESIAN_POINT('',(30.,40.0565314255688,13.7885822331377));
#40739=CARTESIAN_POINT('',(30.,40.0565314255688,13.7885822331377));
#40740=CARTESIAN_POINT('Origin',(30.,40.9225568293533,15.2885822331377));
#40741=CARTESIAN_POINT('',(30.,40.9225568293533,15.2885822331377));
#40742=CARTESIAN_POINT('',(30.,40.9225568293533,15.2885822331377));
#40743=CARTESIAN_POINT('',(30.,40.9225568293533,15.2885822331377));
#40744=CARTESIAN_POINT('Origin',(30.,42.6546076369221,15.2885822331377));
#40745=CARTESIAN_POINT('',(30.,42.6546076369221,15.2885822331377));
#40746=CARTESIAN_POINT('',(30.,42.6546076369221,15.2885822331377));
#40747=CARTESIAN_POINT('',(30.,42.6546076369221,15.2885822331377));
#40748=CARTESIAN_POINT('Origin',(30.,43.5206330407066,13.7885822331377));
#40749=CARTESIAN_POINT('',(30.,43.5206330407066,13.7885822331377));
#40750=CARTESIAN_POINT('',(30.,43.5206330407066,13.7885822331377));
#40751=CARTESIAN_POINT('',(30.,43.5206330407066,13.7885822331377));
#40752=CARTESIAN_POINT('Origin',(30.,42.6546076369221,12.2885822331377));
#40753=CARTESIAN_POINT('',(30.,42.6546076369221,12.2885822331377));
#40754=CARTESIAN_POINT('',(30.,42.6546076369221,12.2885822331377));
#40755=CARTESIAN_POINT('',(30.,42.6546076369221,12.2885822331377));
#40756=CARTESIAN_POINT('Origin',(30.,40.9225568293532,12.2885822331377));
#40757=CARTESIAN_POINT('',(30.,40.9225568293532,12.2885822331377));
#40758=CARTESIAN_POINT('Origin',(30.,0.,0.));
#40759=CARTESIAN_POINT('Origin',(30.,40.0565314255688,-13.7885822331377));
#40760=CARTESIAN_POINT('',(30.,40.9225568293532,-15.2885822331377));
#40761=CARTESIAN_POINT('',(30.,40.9225568293532,-15.2885822331377));
#40762=CARTESIAN_POINT('',(30.,40.0565314255688,-13.7885822331377));
#40763=CARTESIAN_POINT('',(30.,40.0565314255688,-13.7885822331377));
#40764=CARTESIAN_POINT('',(30.,40.0565314255688,-13.7885822331377));
#40765=CARTESIAN_POINT('Origin',(30.,40.9225568293532,-12.2885822331377));
#40766=CARTESIAN_POINT('',(30.,40.9225568293532,-12.2885822331377));
#40767=CARTESIAN_POINT('',(30.,40.9225568293532,-12.2885822331377));
#40768=CARTESIAN_POINT('',(30.,40.9225568293532,-12.2885822331377));
#40769=CARTESIAN_POINT('Origin',(30.,42.6546076369221,-12.2885822331377));
#40770=CARTESIAN_POINT('',(30.,42.6546076369221,-12.2885822331377));
#40771=CARTESIAN_POINT('',(30.,42.6546076369221,-12.2885822331377));
#40772=CARTESIAN_POINT('',(30.,42.6546076369221,-12.2885822331377));
#40773=CARTESIAN_POINT('Origin',(30.,43.5206330407065,-13.7885822331377));
#40774=CARTESIAN_POINT('',(30.,43.5206330407065,-13.7885822331377));
#40775=CARTESIAN_POINT('',(30.,43.5206330407065,-13.7885822331377));
#40776=CARTESIAN_POINT('',(30.,43.5206330407065,-13.7885822331377));
#40777=CARTESIAN_POINT('Origin',(30.,42.6546076369221,-15.2885822331377));
#40778=CARTESIAN_POINT('',(30.,42.6546076369221,-15.2885822331377));
#40779=CARTESIAN_POINT('',(30.,42.6546076369221,-15.2885822331377));
#40780=CARTESIAN_POINT('',(30.,42.6546076369221,-15.2885822331377));
#40781=CARTESIAN_POINT('Origin',(30.,40.9225568293532,-15.2885822331377));
#40782=CARTESIAN_POINT('',(30.,40.9225568293532,-15.2885822331377));
#40783=CARTESIAN_POINT('Origin',(30.,0.,0.));
#40784=CARTESIAN_POINT('Origin',(30.,12.4793669592934,13.7885822331377));
#40785=CARTESIAN_POINT('',(30.,13.3453923630779,12.2885822331377));
#40786=CARTESIAN_POINT('',(30.,13.3453923630779,12.2885822331377));
#40787=CARTESIAN_POINT('',(30.,12.4793669592934,13.7885822331377));
#40788=CARTESIAN_POINT('',(30.,12.4793669592934,13.7885822331377));
#40789=CARTESIAN_POINT('',(30.,12.4793669592934,13.7885822331377));
#40790=CARTESIAN_POINT('Origin',(30.,13.3453923630779,15.2885822331377));
#40791=CARTESIAN_POINT('',(30.,13.3453923630779,15.2885822331377));
#40792=CARTESIAN_POINT('',(30.,13.3453923630779,15.2885822331377));
#40793=CARTESIAN_POINT('',(30.,13.3453923630779,15.2885822331377));
#40794=CARTESIAN_POINT('Origin',(30.,15.0774431706468,15.2885822331377));
#40795=CARTESIAN_POINT('',(30.,15.0774431706468,15.2885822331377));
#40796=CARTESIAN_POINT('',(30.,15.0774431706468,15.2885822331377));
#40797=CARTESIAN_POINT('',(30.,15.0774431706468,15.2885822331377));
#40798=CARTESIAN_POINT('Origin',(30.,15.9434685744312,13.7885822331377));
#40799=CARTESIAN_POINT('',(30.,15.9434685744312,13.7885822331377));
#40800=CARTESIAN_POINT('',(30.,15.9434685744312,13.7885822331377));
#40801=CARTESIAN_POINT('',(30.,15.9434685744312,13.7885822331377));
#40802=CARTESIAN_POINT('Origin',(30.,15.0774431706468,12.2885822331377));
#40803=CARTESIAN_POINT('',(30.,15.0774431706468,12.2885822331377));
#40804=CARTESIAN_POINT('',(30.,15.0774431706468,12.2885822331377));
#40805=CARTESIAN_POINT('',(30.,15.0774431706468,12.2885822331377));
#40806=CARTESIAN_POINT('Origin',(30.,13.3453923630779,12.2885822331377));
#40807=CARTESIAN_POINT('',(30.,13.3453923630779,12.2885822331377));
#40808=CARTESIAN_POINT('Origin',(30.,0.,0.));
#40809=CARTESIAN_POINT('Origin',(30.,12.4793669592934,-13.7885822331377));
#40810=CARTESIAN_POINT('',(30.,13.3453923630779,-15.2885822331377));
#40811=CARTESIAN_POINT('',(30.,13.3453923630779,-15.2885822331377));
#40812=CARTESIAN_POINT('',(30.,12.4793669592934,-13.7885822331377));
#40813=CARTESIAN_POINT('',(30.,12.4793669592934,-13.7885822331377));
#40814=CARTESIAN_POINT('',(30.,12.4793669592934,-13.7885822331377));
#40815=CARTESIAN_POINT('Origin',(30.,13.3453923630779,-12.2885822331377));
#40816=CARTESIAN_POINT('',(30.,13.3453923630779,-12.2885822331377));
#40817=CARTESIAN_POINT('',(30.,13.3453923630779,-12.2885822331377));
#40818=CARTESIAN_POINT('',(30.,13.3453923630779,-12.2885822331377));
#40819=CARTESIAN_POINT('Origin',(30.,15.0774431706468,-12.2885822331377));
#40820=CARTESIAN_POINT('',(30.,15.0774431706468,-12.2885822331377));
#40821=CARTESIAN_POINT('',(30.,15.0774431706468,-12.2885822331377));
#40822=CARTESIAN_POINT('',(30.,15.0774431706468,-12.2885822331377));
#40823=CARTESIAN_POINT('Origin',(30.,15.9434685744312,-13.7885822331377));
#40824=CARTESIAN_POINT('',(30.,15.9434685744312,-13.7885822331377));
#40825=CARTESIAN_POINT('',(30.,15.9434685744312,-13.7885822331377));
#40826=CARTESIAN_POINT('',(30.,15.9434685744312,-13.7885822331377));
#40827=CARTESIAN_POINT('Origin',(30.,15.0774431706468,-15.2885822331377));
#40828=CARTESIAN_POINT('',(30.,15.0774431706468,-15.2885822331377));
#40829=CARTESIAN_POINT('',(30.,15.0774431706468,-15.2885822331377));
#40830=CARTESIAN_POINT('',(30.,15.0774431706468,-15.2885822331377));
#40831=CARTESIAN_POINT('Origin',(30.,13.3453923630779,-15.2885822331377));
#40832=CARTESIAN_POINT('',(30.,13.3453923630779,-15.2885822331377));
#40833=CARTESIAN_POINT('Origin',(30.,0.,0.));
#40834=CARTESIAN_POINT('Origin',(2.,42.,0.));
#40835=CARTESIAN_POINT('Origin',(6.,37.75,0.));
#40836=CARTESIAN_POINT('Origin',(24.,35.5,0.));
#40837=CARTESIAN_POINT('Origin',(27.,37.75,0.));
#40838=CARTESIAN_POINT('',(0.,0.,0.));
#40839=CARTESIAN_POINT('Origin',(4.5,11.,0.));
#40840=CARTESIAN_POINT('',(4.5,10.3991393809724,0.));
#40841=CARTESIAN_POINT('',(5.5,11.,-1.05815080048794E-15));
#40842=CARTESIAN_POINT('',(5.5,11.,-1.22464679914735E-16));
#40843=CARTESIAN_POINT('',(5.,11.,-0.866025403784437));
#40844=CARTESIAN_POINT('Origin',(4.5,11.,0.));
#40845=CARTESIAN_POINT('',(4.,11.,-0.866025403784436));
#40846=CARTESIAN_POINT('Origin',(4.5,11.,0.));
#40847=CARTESIAN_POINT('',(3.5,11.,1.1953210976178E-15));
#40848=CARTESIAN_POINT('Origin',(4.5,11.,0.));
#40849=CARTESIAN_POINT('',(4.,11.,0.866025403784437));
#40850=CARTESIAN_POINT('Origin',(4.5,11.,0.));
#40851=CARTESIAN_POINT('',(5.,11.,0.866025403784438));
#40852=CARTESIAN_POINT('Origin',(4.5,11.,0.));
#40853=CARTESIAN_POINT('Origin',(4.5,11.,0.));
#40854=CARTESIAN_POINT('Origin',(4.5,6.,0.));
#40855=CARTESIAN_POINT('',(6.5,12.5,-8.13194945164231E-17));
#40856=CARTESIAN_POINT('',(2.5,12.5,-2.44929359829471E-16));
#40857=CARTESIAN_POINT('Ctrl Pts',(6.5,12.5,-4.16333634234434E-16));
#40858=CARTESIAN_POINT('Ctrl Pts',(6.5,12.5,-0.251586765531238));
#40859=CARTESIAN_POINT('Ctrl Pts',(6.44963191709473,12.4916317792714,-0.519649901302406));
#40860=CARTESIAN_POINT('Ctrl Pts',(6.24538925206945,12.461387706165,-1.01228304743543));
#40861=CARTESIAN_POINT('Ctrl Pts',(6.09153840204183,12.4399340066366,-1.23688872270436));
#40862=CARTESIAN_POINT('Ctrl Pts',(5.73688470830492,12.3995502329995,-1.59154241644127));
#40863=CARTESIAN_POINT('Ctrl Pts',(5.51228076000427,12.3779753882153,-1.745390117426));
#40864=CARTESIAN_POINT('Ctrl Pts',(5.01965353321852,12.3474532770021,-1.94963049432274));
#40865=CARTESIAN_POINT('Ctrl Pts',(4.75159246112229,12.3389626792531,-2.));
#40866=CARTESIAN_POINT('Ctrl Pts',(4.24840753887771,12.3389626792531,-2.));
#40867=CARTESIAN_POINT('Ctrl Pts',(3.98034646678147,12.3474532770021,-1.94963049432274));
#40868=CARTESIAN_POINT('Ctrl Pts',(3.48771923999573,12.3779753882153,-1.745390117426));
#40869=CARTESIAN_POINT('Ctrl Pts',(3.26311529169508,12.3995502329995,-1.59154241644127));
#40870=CARTESIAN_POINT('Ctrl Pts',(2.90846159795817,12.4399340066366,-1.23688872270436));
#40871=CARTESIAN_POINT('Ctrl Pts',(2.75461074793055,12.461387706165,-1.01228304743543));
#40872=CARTESIAN_POINT('Ctrl Pts',(2.55036808290527,12.4916317792714,-0.519649901302405));
#40873=CARTESIAN_POINT('Ctrl Pts',(2.5,12.5,-0.251586765531237));
#40874=CARTESIAN_POINT('Ctrl Pts',(2.5,12.5,1.38777878078145E-16));
#40875=CARTESIAN_POINT('',(2.5,12.121,-2.44929359829471E-16));
#40876=CARTESIAN_POINT('',(2.5,6.,-2.44929359829471E-16));
#40877=CARTESIAN_POINT('Origin',(4.5,12.121,0.));
#40878=CARTESIAN_POINT('Ctrl Pts',(2.5,12.5,4.85722573273506E-16));
#40879=CARTESIAN_POINT('Ctrl Pts',(2.5,12.5,0.251586765531237));
#40880=CARTESIAN_POINT('Ctrl Pts',(2.55036808290527,12.4916317792714,0.519649901302406));
#40881=CARTESIAN_POINT('Ctrl Pts',(2.75461074793055,12.461387706165,1.01228304743543));
#40882=CARTESIAN_POINT('Ctrl Pts',(2.90846159795817,12.4399340066366,1.23688872270436));
#40883=CARTESIAN_POINT('Ctrl Pts',(3.26311529169508,12.3995502329995,1.59154241644127));
#40884=CARTESIAN_POINT('Ctrl Pts',(3.48771923999573,12.3779753882153,1.745390117426));
#40885=CARTESIAN_POINT('Ctrl Pts',(3.98034646678147,12.3474532770021,1.94963049432274));
#40886=CARTESIAN_POINT('Ctrl Pts',(4.24840753887771,12.3389626792531,2.));
#40887=CARTESIAN_POINT('Ctrl Pts',(4.5,12.3389626792531,2.));
#40888=CARTESIAN_POINT('Ctrl Pts',(4.75159246112229,12.3389626792531,2.));
#40889=CARTESIAN_POINT('Ctrl Pts',(5.01965353321852,12.3474532770021,1.94963049432274));
#40890=CARTESIAN_POINT('Ctrl Pts',(5.51228076000427,12.3779753882153,1.745390117426));
#40891=CARTESIAN_POINT('Ctrl Pts',(5.73688470830492,12.3995502329995,1.59154241644127));
#40892=CARTESIAN_POINT('Ctrl Pts',(6.09153840204183,12.4399340066366,1.23688872270436));
#40893=CARTESIAN_POINT('Ctrl Pts',(6.24538925206945,12.461387706165,1.01228304743543));
#40894=CARTESIAN_POINT('Ctrl Pts',(6.44963191709473,12.4916317792714,0.519649901302405));
#40895=CARTESIAN_POINT('Ctrl Pts',(6.5,12.5,0.251586765531237));
#40896=CARTESIAN_POINT('Ctrl Pts',(6.5,12.5,-4.85722573273506E-16));
#40897=CARTESIAN_POINT('Origin',(4.5,12.121,0.));
#40898=CARTESIAN_POINT('',(2.879,12.5,-1.98515246141786E-16));
#40899=CARTESIAN_POINT('',(2.5,12.121,-2.44929359829471E-16));
#40900=CARTESIAN_POINT('',(6.121,12.5,1.28142565444101E-23));
#40901=CARTESIAN_POINT('Ctrl Pts',(2.879,12.5,-2.08166817117217E-16));
#40902=CARTESIAN_POINT('Ctrl Pts',(2.879,12.5,-0.209746160767273));
#40903=CARTESIAN_POINT('Ctrl Pts',(2.91655267539617,12.4941981000077,-0.434775598398969));
#40904=CARTESIAN_POINT('Ctrl Pts',(3.07235632722532,12.4725703604218,-0.853817682393516));
#40905=CARTESIAN_POINT('Ctrl Pts',(3.19061611370051,12.4569932358364,-1.04783985285898));
#40906=CARTESIAN_POINT('Ctrl Pts',(3.47117700763803,12.4264861212993,-1.36306503279426));
#40907=CARTESIAN_POINT('Ctrl Pts',(3.65386827011239,12.4094890721184,-1.50458240783022));
#40908=CARTESIAN_POINT('Ctrl Pts',(4.06154772862311,12.3849563429367,-1.69471072657775));
#40909=CARTESIAN_POINT('Ctrl Pts',(4.28664804766627,12.377862104465,-1.74313789553504));
#40910=CARTESIAN_POINT('Ctrl Pts',(4.71335195233373,12.377862104465,-1.74313789553504));
#40911=CARTESIAN_POINT('Ctrl Pts',(4.93845227137689,12.3849563429367,-1.69471072657775));
#40912=CARTESIAN_POINT('Ctrl Pts',(5.34613172988761,12.4094890721184,-1.50458240783022));
#40913=CARTESIAN_POINT('Ctrl Pts',(5.52882299236196,12.4264861212993,-1.36306503279425));
#40914=CARTESIAN_POINT('Ctrl Pts',(5.80938388629949,12.4569932358364,-1.04783985285898));
#40915=CARTESIAN_POINT('Ctrl Pts',(5.92764367277468,12.4725703604218,-0.853817682393517));
#40916=CARTESIAN_POINT('Ctrl Pts',(6.08344732460383,12.4941981000077,-0.43477559839897));
#40917=CARTESIAN_POINT('Ctrl Pts',(6.121,12.5,-0.209746160767274));
#40918=CARTESIAN_POINT('Ctrl Pts',(6.121,12.5,-5.55111512312578E-16));
#40919=CARTESIAN_POINT('Ctrl Pts',(6.121,12.5,-3.46944695195361E-16));
#40920=CARTESIAN_POINT('Ctrl Pts',(6.121,12.5,0.209746160767274));
#40921=CARTESIAN_POINT('Ctrl Pts',(6.08344732460383,12.4941981000077,0.43477559839897));
#40922=CARTESIAN_POINT('Ctrl Pts',(5.92764367277468,12.4725703604218,0.853817682393517));
#40923=CARTESIAN_POINT('Ctrl Pts',(5.80938388629949,12.4569932358364,1.04783985285898));
#40924=CARTESIAN_POINT('Ctrl Pts',(5.52882299236196,12.4264861212993,1.36306503279426));
#40925=CARTESIAN_POINT('Ctrl Pts',(5.34613172988761,12.4094890721184,1.50458240783022));
#40926=CARTESIAN_POINT('Ctrl Pts',(4.93845227137689,12.3849563429367,1.69471072657775));
#40927=CARTESIAN_POINT('Ctrl Pts',(4.71335195233373,12.377862104465,1.74313789553504));
#40928=CARTESIAN_POINT('Ctrl Pts',(4.5,12.377862104465,1.74313789553504));
#40929=CARTESIAN_POINT('Ctrl Pts',(4.28664804766627,12.377862104465,1.74313789553504));
#40930=CARTESIAN_POINT('Ctrl Pts',(4.06154772862311,12.3849563429367,1.69471072657775));
#40931=CARTESIAN_POINT('Ctrl Pts',(3.65386827011239,12.4094890721184,1.50458240783022));
#40932=CARTESIAN_POINT('Ctrl Pts',(3.47117700763804,12.4264861212993,1.36306503279425));
#40933=CARTESIAN_POINT('Ctrl Pts',(3.19061611370051,12.4569932358364,1.04783985285898));
#40934=CARTESIAN_POINT('Ctrl Pts',(3.07235632722532,12.4725703604218,0.853817682393517));
#40935=CARTESIAN_POINT('Ctrl Pts',(2.91655267539617,12.4941981000077,0.43477559839897));
#40936=CARTESIAN_POINT('Ctrl Pts',(2.879,12.5,0.209746160767274));
#40937=CARTESIAN_POINT('Ctrl Pts',(2.879,12.5,6.93889390390723E-17));
#40938=CARTESIAN_POINT('Origin',(4.5,7.5,0.));
#40939=CARTESIAN_POINT('',(2.5,8.25000000000001,2.44929359829471E-16));
#40940=CARTESIAN_POINT('',(6.5,8.25000000000001,-2.44929359829471E-16));
#40941=CARTESIAN_POINT('Origin',(4.5,8.25000000000001,0.));
#40942=CARTESIAN_POINT('',(5.75,7.5,-1.53080849893419E-16));
#40943=CARTESIAN_POINT('',(5.75,7.5,-1.53080849893419E-16));
#40944=CARTESIAN_POINT('Origin',(4.5,7.5,0.));
#40945=CARTESIAN_POINT('Origin',(4.5,8.25000000000001,0.));
#40946=CARTESIAN_POINT('Origin',(4.5,6.,0.));
#40947=CARTESIAN_POINT('',(2.5,6.9585,-2.6124255799288E-16));
#40948=CARTESIAN_POINT('',(2.5,6.,-2.44929359829471E-16));
#40949=CARTESIAN_POINT('',(6.5,6.9585,5.51554030451387E-17));
#40950=CARTESIAN_POINT('Ctrl Pts',(2.5,6.9585,-2.77555756156289E-16));
#40951=CARTESIAN_POINT('Ctrl Pts',(2.5,6.9585,-0.252637698086405));
#40952=CARTESIAN_POINT('Ctrl Pts',(2.55078010677237,6.94337565665523,-0.521159230418503));
#40953=CARTESIAN_POINT('Ctrl Pts',(2.75533748034076,6.88874841306866,-1.01351751722741));
#40954=CARTESIAN_POINT('Ctrl Pts',(2.90903822842602,6.84996260038966,-1.23746535317221));
#40955=CARTESIAN_POINT('Ctrl Pts',(3.26257869425884,6.77657914101289,-1.59100581900503));
#40956=CARTESIAN_POINT('Ctrl Pts',(3.48650851036758,6.7370684472136,-1.74467239254521));
#40957=CARTESIAN_POINT('Ctrl Pts',(3.9788017352627,6.68076154284702,-1.94920461648384));
#40958=CARTESIAN_POINT('Ctrl Pts',(4.2472993420588,6.66488726461296,-2.));
#40959=CARTESIAN_POINT('Ctrl Pts',(4.7527006579412,6.66488726461296,-2.));
#40960=CARTESIAN_POINT('Ctrl Pts',(5.0211982647373,6.68076154284702,-1.94920461648384));
#40961=CARTESIAN_POINT('Ctrl Pts',(5.51349148963242,6.7370684472136,-1.74467239254521));
#40962=CARTESIAN_POINT('Ctrl Pts',(5.73742130574116,6.77657914101289,-1.59100581900503));
#40963=CARTESIAN_POINT('Ctrl Pts',(6.09096177157398,6.84996260038966,-1.23746535317221));
#40964=CARTESIAN_POINT('Ctrl Pts',(6.24466251965925,6.88874841306866,-1.01351751722741));
#40965=CARTESIAN_POINT('Ctrl Pts',(6.44921989322763,6.94337565665523,-0.521159230418501));
#40966=CARTESIAN_POINT('Ctrl Pts',(6.5,6.9585,-0.252637698086404));
#40967=CARTESIAN_POINT('Ctrl Pts',(6.5,6.9585,-6.93889390390723E-17));
#40968=CARTESIAN_POINT('Ctrl Pts',(6.5,6.9585,2.08166817117217E-16));
#40969=CARTESIAN_POINT('Ctrl Pts',(6.5,6.9585,0.252637698086405));
#40970=CARTESIAN_POINT('Ctrl Pts',(6.44921989322763,6.94337565665523,0.521159230418502));
#40971=CARTESIAN_POINT('Ctrl Pts',(6.24466251965925,6.88874841306866,1.01351751722741));
#40972=CARTESIAN_POINT('Ctrl Pts',(6.09096177157398,6.84996260038966,1.23746535317221));
#40973=CARTESIAN_POINT('Ctrl Pts',(5.73742130574116,6.77657914101289,1.59100581900503));
#40974=CARTESIAN_POINT('Ctrl Pts',(5.51349148963242,6.7370684472136,1.74467239254521));
#40975=CARTESIAN_POINT('Ctrl Pts',(5.0211982647373,6.68076154284702,1.94920461648384));
#40976=CARTESIAN_POINT('Ctrl Pts',(4.7527006579412,6.66488726461296,2.));
#40977=CARTESIAN_POINT('Ctrl Pts',(4.5,6.66488726461296,2.));
#40978=CARTESIAN_POINT('Ctrl Pts',(4.2472993420588,6.66488726461296,2.));
#40979=CARTESIAN_POINT('Ctrl Pts',(3.9788017352627,6.68076154284702,1.94920461648384));
#40980=CARTESIAN_POINT('Ctrl Pts',(3.48650851036758,6.7370684472136,1.74467239254521));
#40981=CARTESIAN_POINT('Ctrl Pts',(3.26257869425884,6.77657914101289,1.59100581900503));
#40982=CARTESIAN_POINT('Ctrl Pts',(2.90903822842602,6.84996260038966,1.23746535317221));
#40983=CARTESIAN_POINT('Ctrl Pts',(2.75533748034075,6.88874841306866,1.01351751722741));
#40984=CARTESIAN_POINT('Ctrl Pts',(2.55078010677237,6.94337565665523,0.521159230418502));
#40985=CARTESIAN_POINT('Ctrl Pts',(2.5,6.9585,0.252637698086404));
#40986=CARTESIAN_POINT('Ctrl Pts',(2.5,6.9585,-2.08166817117217E-16));
#40987=CARTESIAN_POINT('Origin',(7.4585,0.,0.));
#40988=CARTESIAN_POINT('',(7.4585,8.52170475186686E-16,-6.9585));
#40989=CARTESIAN_POINT('',(7.4585,-8.52170475186686E-16,6.9585));
#40990=CARTESIAN_POINT('Origin',(7.4585,0.,0.));
#40991=CARTESIAN_POINT('',(8.,-9.18485099360515E-16,7.5));
#40992=CARTESIAN_POINT('',(7.4585,-8.52170475186686E-16,6.9585));
#40993=CARTESIAN_POINT('Origin',(8.,0.,0.));
#40994=CARTESIAN_POINT('Origin',(7.4585,0.,0.));
#40995=CARTESIAN_POINT('Origin',(0.,0.,0.));
#40996=CARTESIAN_POINT('',(0.5415,-8.52170475186686E-16,-6.9585));
#40997=CARTESIAN_POINT('Origin',(0.541499999999999,0.,0.));
#40998=CARTESIAN_POINT('',(-5.77101208116537E-16,-9.18485099360515E-16,
-7.5));
#40999=CARTESIAN_POINT('',(0.,-9.18485099360515E-16,-7.5));
#41000=CARTESIAN_POINT('Origin',(0.,0.,0.));
#41001=CARTESIAN_POINT('Origin',(-0.4,0.,0.));
#41002=CARTESIAN_POINT('',(8.,-3.57996068711535,11.9763884989887));
#41003=CARTESIAN_POINT('',(8.,3.57996068711535,11.9763884989887));
#41004=CARTESIAN_POINT('Origin',(8.,0.,0.));
#41005=CARTESIAN_POINT('',(1.,3.57996068711535,11.9763884989887));
#41006=CARTESIAN_POINT('',(-0.4,3.57996068711535,11.9763884989887));
#41007=CARTESIAN_POINT('',(1.,-3.57996068711536,11.9763884989887));
#41008=CARTESIAN_POINT('Origin',(1.,0.,0.));
#41009=CARTESIAN_POINT('',(-0.4,-3.57996068711536,11.9763884989887));
#41010=CARTESIAN_POINT('Origin',(-0.4,0.,0.));
#41011=CARTESIAN_POINT('',(0.,-1.28587913910472E-15,-10.5));
#41012=CARTESIAN_POINT('Origin',(0.,0.,0.));
#41013=CARTESIAN_POINT('',(1.,-1.28587913910472E-15,-10.5));
#41014=CARTESIAN_POINT('',(-0.4,-1.28587913910472E-15,-10.5));
#41015=CARTESIAN_POINT('Origin',(1.,0.,0.));
#41016=CARTESIAN_POINT('Origin',(0.,0.,0.));
#41017=CARTESIAN_POINT('',(0.,-8.52170475186686E-16,-6.9585));
#41018=CARTESIAN_POINT('Origin',(-0.4,0.,0.));
#41019=CARTESIAN_POINT('',(5.5,12.4866595479602,-0.577350269189626));
#41020=CARTESIAN_POINT('',(5.5,12.4866595479602,0.577350269189624));
#41021=CARTESIAN_POINT('Origin',(5.5,0.,0.));
#41022=CARTESIAN_POINT('',(4.5,12.4465524008324,1.15470053837925));
#41023=CARTESIAN_POINT('Origin',(6.49474644070762,-37.2251671136432,0.00303314386277891));
#41024=CARTESIAN_POINT('',(3.5,12.4866595479602,0.577350269189625));
#41025=CARTESIAN_POINT('Origin',(2.50525355929134,-37.2251671136413,0.00303314386722944));
#41026=CARTESIAN_POINT('',(3.5,12.4866595479602,-0.577350269189624));
#41027=CARTESIAN_POINT('Origin',(3.5,0.,0.));
#41028=CARTESIAN_POINT('',(4.5,12.4465524008324,-1.15470053837925));
#41029=CARTESIAN_POINT('Origin',(2.505253559288,-37.2251671136122,-0.00303314386702086));
#41030=CARTESIAN_POINT('Origin',(6.49474644071747,-37.2251671136628,-0.00303314387395726));
#41031=CARTESIAN_POINT('Origin',(-0.4,0.,0.));
#41032=CARTESIAN_POINT('',(8.,11.9763884989887,3.57996068711535));
#41033=CARTESIAN_POINT('',(8.,11.9763884989887,-3.57996068711535));
#41034=CARTESIAN_POINT('Origin',(8.,0.,0.));
#41035=CARTESIAN_POINT('',(1.,11.9763884989887,-3.57996068711535));
#41036=CARTESIAN_POINT('',(-0.4,11.9763884989887,-3.57996068711535));
#41037=CARTESIAN_POINT('',(1.,11.9763884989887,3.57996068711535));
#41038=CARTESIAN_POINT('Origin',(1.,0.,0.));
#41039=CARTESIAN_POINT('',(-0.4,11.9763884989887,3.57996068711535));
#41040=CARTESIAN_POINT('Origin',(-0.4,0.,0.));
#41041=CARTESIAN_POINT('',(8.,-11.9763884989887,-3.57996068711537));
#41042=CARTESIAN_POINT('',(8.,-11.9763884989887,3.57996068711536));
#41043=CARTESIAN_POINT('Origin',(8.,0.,0.));
#41044=CARTESIAN_POINT('',(1.,-11.9763884989887,3.57996068711537));
#41045=CARTESIAN_POINT('',(-0.4,-11.9763884989887,3.57996068711536));
#41046=CARTESIAN_POINT('',(1.,-11.9763884989887,-3.57996068711537));
#41047=CARTESIAN_POINT('Origin',(1.,0.,0.));
#41048=CARTESIAN_POINT('',(-0.4,-11.9763884989887,-3.57996068711537));
#41049=CARTESIAN_POINT('Origin',(-0.4,0.,0.));
#41050=CARTESIAN_POINT('',(8.,3.57996068711536,-11.9763884989887));
#41051=CARTESIAN_POINT('',(8.,-3.57996068711536,-11.9763884989887));
#41052=CARTESIAN_POINT('Origin',(8.,0.,0.));
#41053=CARTESIAN_POINT('',(1.,-3.57996068711536,-11.9763884989887));
#41054=CARTESIAN_POINT('',(-0.4,-3.57996068711536,-11.9763884989887));
#41055=CARTESIAN_POINT('',(1.,3.57996068711536,-11.9763884989887));
#41056=CARTESIAN_POINT('Origin',(1.,0.,0.));
#41057=CARTESIAN_POINT('',(-0.4,3.57996068711536,-11.9763884989887));
#41058=CARTESIAN_POINT('Origin',(0.,0.,0.));
#41059=CARTESIAN_POINT('Origin',(1.,10.5,0.));
#41060=CARTESIAN_POINT('',(1.,-2.52817459305202,13.028174593052));
#41061=CARTESIAN_POINT('',(1.,13.028174593052,2.52817459305202));
#41062=CARTESIAN_POINT('',(1.,13.028174593052,-2.52817459305202));
#41063=CARTESIAN_POINT('',(1.,-2.52817459305202,-13.028174593052));
#41064=CARTESIAN_POINT('Origin',(8.,12.5,0.));
#41065=CARTESIAN_POINT('',(8.,-1.52817459305202,14.028174593052));
#41066=CARTESIAN_POINT('',(8.,-1.52817459305202,-14.028174593052));
#41067=CARTESIAN_POINT('',(8.,14.028174593052,-1.52817459305202));
#41068=CARTESIAN_POINT('',(8.,14.028174593052,1.52817459305202));
#41069=CARTESIAN_POINT('Origin',(8.,15.556349186104,0.));
#41070=CARTESIAN_POINT('Origin',(8.,-5.42101086242754E-17,-15.556349186104));
#41071=CARTESIAN_POINT('Origin',(8.,-5.42101086242754E-17,-15.556349186104));
#41072=CARTESIAN_POINT('Origin',(8.,-15.5563491861041,-3.52365706057789E-15));
#41073=CARTESIAN_POINT('Origin',(3.25,7.5,0.));
#41074=CARTESIAN_POINT('Origin',(4.5,11.,1.15470053837925));
#41075=CARTESIAN_POINT('',(5.5,11.,0.577350269189624));
#41076=CARTESIAN_POINT('',(5.5,11.,0.577350269189624));
#41077=CARTESIAN_POINT('',(4.5,11.,1.15470053837925));
#41078=CARTESIAN_POINT('',(4.5,11.,1.15470053837925));
#41079=CARTESIAN_POINT('',(4.5,11.,1.15470053837925));
#41080=CARTESIAN_POINT('',(4.5,11.,1.15470053837925));
#41081=CARTESIAN_POINT('Origin',(3.5,11.,0.577350269189625));
#41082=CARTESIAN_POINT('',(3.5,11.,0.577350269189625));
#41083=CARTESIAN_POINT('',(3.5,11.,0.577350269189625));
#41084=CARTESIAN_POINT('',(3.5,11.,0.577350269189625));
#41085=CARTESIAN_POINT('',(3.5,11.,0.577350269189625));
#41086=CARTESIAN_POINT('Origin',(3.5,11.,-0.577350269189624));
#41087=CARTESIAN_POINT('',(3.5,11.,-0.577350269189624));
#41088=CARTESIAN_POINT('',(3.5,11.,-0.577350269189624));
#41089=CARTESIAN_POINT('',(3.5,11.,-0.577350269189624));
#41090=CARTESIAN_POINT('',(3.5,11.,-0.577350269189624));
#41091=CARTESIAN_POINT('Origin',(4.5,11.,-1.15470053837925));
#41092=CARTESIAN_POINT('',(4.5,11.,-1.15470053837925));
#41093=CARTESIAN_POINT('',(4.5,11.,-1.15470053837925));
#41094=CARTESIAN_POINT('',(4.5,11.,-1.15470053837925));
#41095=CARTESIAN_POINT('',(4.5,11.,-1.15470053837925));
#41096=CARTESIAN_POINT('Origin',(5.5,11.,-0.577350269189626));
#41097=CARTESIAN_POINT('',(5.5,11.,-0.577350269189626));
#41098=CARTESIAN_POINT('',(5.5,11.,-0.577350269189626));
#41099=CARTESIAN_POINT('',(5.5,11.,-0.577350269189626));
#41100=CARTESIAN_POINT('',(5.5,11.,-0.577350269189626));
#41101=CARTESIAN_POINT('Origin',(5.5,11.,0.577350269189624));
#41102=CARTESIAN_POINT('',(5.5,11.,0.577350269189624));
#41103=CARTESIAN_POINT('',(5.5,11.,0.577350269189624));
#41104=CARTESIAN_POINT('Origin',(0.,11.,0.));
#41105=CARTESIAN_POINT('Origin',(0.,11.,0.));
#41106=CARTESIAN_POINT('Origin',(0.,11.,0.));
#41107=CARTESIAN_POINT('Origin',(0.,11.,0.));
#41108=CARTESIAN_POINT('Origin',(0.,11.,0.));
#41109=CARTESIAN_POINT('Origin',(0.,11.,0.));
#41110=CARTESIAN_POINT('',(0.,0.,0.));
#41111=CARTESIAN_POINT('Origin',(-0.25,0.,0.));
#41112=CARTESIAN_POINT('',(-3.12250225675825E-16,-1.19403062916867E-15,
-9.75));
#41113=CARTESIAN_POINT('Origin',(-3.25260651745651E-16,0.,0.));
#41114=CARTESIAN_POINT('',(6.,-1.19403062916867E-15,-9.75));
#41115=CARTESIAN_POINT('',(-0.25,-1.19403062916867E-15,-9.75));
#41116=CARTESIAN_POINT('Origin',(6.,0.,0.));
#41117=CARTESIAN_POINT('Origin',(-0.25,0.,0.));
#41118=CARTESIAN_POINT('',(6.,-9.18485099360515E-16,-7.5));
#41119=CARTESIAN_POINT('Origin',(6.,0.,0.));
#41120=CARTESIAN_POINT('',(0.,-9.18485099360515E-16,-7.5));
#41121=CARTESIAN_POINT('',(-0.25,-9.18485099360515E-16,-7.5));
#41122=CARTESIAN_POINT('Origin',(0.,0.,0.));
#41123=CARTESIAN_POINT('Origin',(-1.53080849893419E-16,9.75,0.));
#41124=CARTESIAN_POINT('Origin',(6.,7.5,0.));
#41125=CARTESIAN_POINT('',(0.,0.,0.));
#41126=CARTESIAN_POINT('',(6.00000000000001,28.,1.28627882350956E-15));
#41127=CARTESIAN_POINT('',(30.,28.,9.86076131526265E-29));
#41128=CARTESIAN_POINT('',(24.,28.,9.86076131526265E-29));
#41129=CARTESIAN_POINT('',(0.,0.,0.));
#41130=CARTESIAN_POINT('Origin',(-24.,0.999999999999997,1.5));
#41131=CARTESIAN_POINT('',(-27.,0.999999999999996,-3.5));
#41132=CARTESIAN_POINT('Origin',(-24.,0.999999999999997,-3.5));
#41133=CARTESIAN_POINT('',(-27.,0.999999999999996,1.5));
#41134=CARTESIAN_POINT('',(-27.,0.999999999999996,1.5));
#41135=CARTESIAN_POINT('Origin',(-24.,0.999999999999997,1.5));
#41136=CARTESIAN_POINT('Origin',(0.,-14.,1.5));
#41137=CARTESIAN_POINT('',(-3.,-14.,-3.5));
#41138=CARTESIAN_POINT('Origin',(0.,-14.,-3.5));
#41139=CARTESIAN_POINT('',(-3.,-14.,1.5));
#41140=CARTESIAN_POINT('',(-3.,-14.,1.5));
#41141=CARTESIAN_POINT('Origin',(0.,-14.,1.5));
#41142=CARTESIAN_POINT('Origin',(15.,-14.,-3.5));
#41143=CARTESIAN_POINT('',(11.75,-14.,-3.5));
#41144=CARTESIAN_POINT('Origin',(15.,-14.,-3.5));
#41145=CARTESIAN_POINT('',(11.75,-14.,1.5));
#41146=CARTESIAN_POINT('',(11.75,-14.,-3.5));
#41147=CARTESIAN_POINT('Origin',(15.,-14.,1.5));
#41148=CARTESIAN_POINT('Origin',(-39.,0.999999999999997,-3.5));
#41149=CARTESIAN_POINT('',(-42.25,0.999999999999996,-3.5));
#41150=CARTESIAN_POINT('Origin',(-39.,0.999999999999997,-3.5));
#41151=CARTESIAN_POINT('',(-42.25,0.999999999999996,1.5));
#41152=CARTESIAN_POINT('',(-42.25,0.999999999999996,-3.5));
#41153=CARTESIAN_POINT('Origin',(-39.,0.999999999999997,1.5));
#41154=CARTESIAN_POINT('Origin',(15.,0.999999999999997,-3.5));
#41155=CARTESIAN_POINT('',(11.75,0.999999999999996,-3.5));
#41156=CARTESIAN_POINT('Origin',(15.,0.999999999999997,-3.5));
#41157=CARTESIAN_POINT('',(11.75,0.999999999999996,1.5));
#41158=CARTESIAN_POINT('',(11.75,0.999999999999996,-3.5));
#41159=CARTESIAN_POINT('Origin',(15.,0.999999999999997,1.5));
#41160=CARTESIAN_POINT('Origin',(-39.,-14.,-3.5));
#41161=CARTESIAN_POINT('',(-42.25,-14.,-3.5));
#41162=CARTESIAN_POINT('Origin',(-39.,-14.,-3.5));
#41163=CARTESIAN_POINT('',(-42.25,-14.,1.5));
#41164=CARTESIAN_POINT('',(-42.25,-14.,-3.5));
#41165=CARTESIAN_POINT('Origin',(-39.,-14.,1.5));
#41166=CARTESIAN_POINT('Origin',(0.,0.,3.5));
#41167=CARTESIAN_POINT('',(23.,-12.,3.5));
#41168=CARTESIAN_POINT('',(23.,8.,3.5));
#41169=CARTESIAN_POINT('',(23.,8.,3.5));
#41170=CARTESIAN_POINT('',(25.5,-12.,3.5));
#41171=CARTESIAN_POINT('',(23.,-12.,3.5));
#41172=CARTESIAN_POINT('',(25.5,8.,3.5));
#41173=CARTESIAN_POINT('',(25.5,8.,3.5));
#41174=CARTESIAN_POINT('',(-48.,8.,3.5));
#41175=CARTESIAN_POINT('Origin',(25.5,8.,3.5));
#41176=CARTESIAN_POINT('',(25.5,-12.,1.5));
#41177=CARTESIAN_POINT('',(25.5,-12.,1.5));
#41178=CARTESIAN_POINT('',(25.5,-22.,1.5));
#41179=CARTESIAN_POINT('',(25.5,-22.,1.5));
#41180=CARTESIAN_POINT('',(25.5,-22.,-3.5));
#41181=CARTESIAN_POINT('',(25.5,-22.,3.5));
#41182=CARTESIAN_POINT('',(25.5,8.,-3.5));
#41183=CARTESIAN_POINT('',(25.5,8.,-3.5));
#41184=CARTESIAN_POINT('',(25.5,8.,3.5));
#41185=CARTESIAN_POINT('Origin',(-48.,8.,3.5));
#41186=CARTESIAN_POINT('',(23.,8.,1.5));
#41187=CARTESIAN_POINT('',(-48.,8.,1.5));
#41188=CARTESIAN_POINT('',(-48.,8.,1.5));
#41189=CARTESIAN_POINT('',(23.,8.,1.5));
#41190=CARTESIAN_POINT('',(-48.,8.,-3.5));
#41191=CARTESIAN_POINT('',(-48.,8.,-3.5));
#41192=CARTESIAN_POINT('',(-48.,8.,3.5));
#41193=CARTESIAN_POINT('Origin',(-48.,8.,3.5));
#41194=CARTESIAN_POINT('',(-48.,-20.,3.5));
#41195=CARTESIAN_POINT('',(-48.,-22.,3.5));
#41196=CARTESIAN_POINT('',(-48.,8.,3.5));
#41197=CARTESIAN_POINT('',(-48.,-20.,1.5));
#41198=CARTESIAN_POINT('',(-48.,-20.,1.5));
#41199=CARTESIAN_POINT('',(-48.,8.,1.5));
#41200=CARTESIAN_POINT('',(-48.,-22.,-3.5));
#41201=CARTESIAN_POINT('',(-48.,8.,-3.5));
#41202=CARTESIAN_POINT('',(-48.,-22.,3.5));
#41203=CARTESIAN_POINT('Origin',(-48.,-22.,3.5));
#41204=CARTESIAN_POINT('',(5.49999999999999,-22.,1.5));
#41205=CARTESIAN_POINT('',(5.49999999999999,-22.,1.5));
#41206=CARTESIAN_POINT('',(5.49999999999999,-22.,3.5));
#41207=CARTESIAN_POINT('',(5.49999999999999,-22.,1.5));
#41208=CARTESIAN_POINT('',(-48.,-22.,3.5));
#41209=CARTESIAN_POINT('',(-48.,-22.,-3.5));
#41210=CARTESIAN_POINT('Origin',(0.,0.,3.5));
#41211=CARTESIAN_POINT('',(5.49999999999998,-20.,3.5));
#41212=CARTESIAN_POINT('',(5.49999999999998,-20.,3.5));
#41213=CARTESIAN_POINT('',(-48.,-20.,3.5));
#41214=CARTESIAN_POINT('Origin',(0.,0.,-3.5));
#41215=CARTESIAN_POINT('Origin',(23.,8.,1.5));
#41216=CARTESIAN_POINT('',(23.,-12.,1.5));
#41217=CARTESIAN_POINT('',(23.,8.,1.5));
#41218=CARTESIAN_POINT('',(23.,-12.,1.5));
#41219=CARTESIAN_POINT('Origin',(23.,-12.,1.5));
#41220=CARTESIAN_POINT('',(23.,-12.,1.5));
#41221=CARTESIAN_POINT('Origin',(5.49999999999998,-20.,1.5));
#41222=CARTESIAN_POINT('',(5.49999999999998,-20.,1.5));
#41223=CARTESIAN_POINT('',(5.49999999999998,-20.,1.5));
#41224=CARTESIAN_POINT('',(5.49999999999998,-20.,1.5));
#41225=CARTESIAN_POINT('Origin',(-48.,-20.,1.5));
#41226=CARTESIAN_POINT('',(-48.,-20.,1.5));
#41227=CARTESIAN_POINT('Origin',(0.,0.,1.5));
#41228=CARTESIAN_POINT('',(0.,0.,0.));
#41229=CARTESIAN_POINT('',(0.,0.,0.));
#41230=CARTESIAN_POINT('',(0.,0.,0.));
#41231=CARTESIAN_POINT('Origin',(8.3,0.,0.));
#41232=CARTESIAN_POINT('',(8.3,-16.1678918191954,6.69696006579904));
#41233=CARTESIAN_POINT('Origin',(8.3,-18.015650884246,7.46232693046164));
#41234=CARTESIAN_POINT('Origin',(8.3,-18.015650884246,7.46232693046164));
#41235=CARTESIAN_POINT('',(7.,-16.1678918191954,6.69696006579904));
#41236=CARTESIAN_POINT('',(8.3,-16.1678918191954,6.69696006579904));
#41237=CARTESIAN_POINT('Origin',(7.,-18.015650884246,7.46232693046164));
#41238=CARTESIAN_POINT('Origin',(-8.3,0.,0.));
#41239=CARTESIAN_POINT('',(-8.3,-6.69696006698037,16.1678918187026));
#41240=CARTESIAN_POINT('Origin',(-8.3,-7.46232693177812,18.0156508836972));
#41241=CARTESIAN_POINT('Origin',(-7.,-7.46232693177812,18.0156508836972));
#41242=CARTESIAN_POINT('',(-7.,-6.69696006698037,16.1678918187026));
#41243=CARTESIAN_POINT('Origin',(-7.,-7.46232693177812,18.0156508836972));
#41244=CARTESIAN_POINT('',(-7.,-6.69696006698036,16.1678918187026));
#41245=CARTESIAN_POINT('Ctrl Pts',(7.10525808636416,14.3565635298793,7.16063659654178));
#41246=CARTESIAN_POINT('Ctrl Pts',(7.10575876444043,14.3387789637918,7.19592366196931));
#41247=CARTESIAN_POINT('Ctrl Pts',(7.10223937876377,14.2836777370554,7.30797308590476));
#41248=CARTESIAN_POINT('Ctrl Pts',(7.06770483392813,14.1927233116185,7.50815817028447));
#41249=CARTESIAN_POINT('Ctrl Pts',(6.97267785327267,14.0924356480638,7.75900571169227));
#41250=CARTESIAN_POINT('Ctrl Pts',(6.81702606252464,14.010417021847,8.00596596099621));
#41251=CARTESIAN_POINT('Ctrl Pts',(6.60785644388706,13.9583672553273,8.22304070094113));
#41252=CARTESIAN_POINT('Ctrl Pts',(6.40912170184387,13.9451967772279,8.35867896670148));
#41253=CARTESIAN_POINT('Ctrl Pts',(6.28621415412844,13.9496957605692,8.41828411660249));
#41254=CARTESIAN_POINT('Ctrl Pts',(6.24974104220345,13.9520455424819,8.43403152063555));
#41255=CARTESIAN_POINT('Ctrl Pts',(6.81652863846456,13.838553574665,6.9039568015009));
#41256=CARTESIAN_POINT('Ctrl Pts',(6.81697830810448,13.8228760451423,6.93504899056999));
#41257=CARTESIAN_POINT('Ctrl Pts',(6.81382002318898,13.7743041309446,7.03391985983529));
#41258=CARTESIAN_POINT('Ctrl Pts',(6.78271672624039,13.6942666755865,7.21111662303983));
#41259=CARTESIAN_POINT('Ctrl Pts',(6.69707233669569,13.606593950197,7.43348605086638));
#41260=CARTESIAN_POINT('Ctrl Pts',(6.5570604709967,13.5357964998358,7.6522164860747));
#41261=CARTESIAN_POINT('Ctrl Pts',(6.36965839370619,13.4919926525689,7.84392391935531));
#41262=CARTESIAN_POINT('Ctrl Pts',(6.19259577880842,13.4820718993109,7.96318830858491));
#41263=CARTESIAN_POINT('Ctrl Pts',(6.08364035524788,13.4867937044583,8.01543121257244));
#41264=CARTESIAN_POINT('Ctrl Pts',(6.05135731015642,13.4890581680742,8.02922278350448));
#41265=CARTESIAN_POINT('Ctrl Pts',(7.059396511537,13.3051669887233,6.63188003220261));
#41266=CARTESIAN_POINT('Ctrl Pts',(7.05998753389128,13.2848957072356,6.67210384463059));
#41267=CARTESIAN_POINT('Ctrl Pts',(7.05582531382928,13.2222257804441,6.79953300552684));
#41268=CARTESIAN_POINT('Ctrl Pts',(7.01532499205948,13.1191751284561,7.02616529659645));
#41269=CARTESIAN_POINT('Ctrl Pts',(6.90406234216587,13.0054588505149,7.31013013126185));
#41270=CARTESIAN_POINT('Ctrl Pts',(6.72098844767873,12.9119197076438,7.59124630672048));
#41271=CARTESIAN_POINT('Ctrl Pts',(6.47267893719941,12.8520752435282,7.8409976590492));
#41272=CARTESIAN_POINT('Ctrl Pts',(6.23373408548986,12.8370545490279,7.9994819202324));
#41273=CARTESIAN_POINT('Ctrl Pts',(6.08428318984346,12.8428248784391,8.07006964139502));
#41274=CARTESIAN_POINT('Ctrl Pts',(6.0397814795314,12.8457670018725,8.08880192603315));
#41275=CARTESIAN_POINT('Ctrl Pts',(7.66907949078917,13.1178290552721,6.52876987767165));
#41276=CARTESIAN_POINT('Ctrl Pts',(7.66990836900527,13.0893786582693,6.58525885810878));
#41277=CARTESIAN_POINT('Ctrl Pts',(7.66405799361575,13.001544514722,6.76361524924263));
#41278=CARTESIAN_POINT('Ctrl Pts',(7.60770496051459,12.8571579080423,7.07858023439957));
#41279=CARTESIAN_POINT('Ctrl Pts',(7.45319621673626,12.6964022703982,7.47244067179396));
#41280=CARTESIAN_POINT('Ctrl Pts',(7.19756079194026,12.5615820193213,7.86424907202288));
#41281=CARTESIAN_POINT('Ctrl Pts',(6.8469730169815,12.4722893095407,8.21609142295753));
#41282=CARTESIAN_POINT('Ctrl Pts',(6.5045565862393,12.4472780949918,8.44279153754262));
#41283=CARTESIAN_POINT('Ctrl Pts',(6.28762425993378,12.4542118419042,8.54499034275498));
#41284=CARTESIAN_POINT('Ctrl Pts',(6.22278112148675,12.4581351147872,8.57220928430822));
#41285=CARTESIAN_POINT('',(6.26385989006508,13.9442649556658,8.42071839528551));
#41286=CARTESIAN_POINT('',(6.24996405537491,12.462652577598,8.55168635783618));
#41287=CARTESIAN_POINT('Origin',(6.527841919986,13.2547471496042,9.09516599269981));
#41288=CARTESIAN_POINT('',(6.99999974236212,12.522062102245,8.04447864893747));
#41289=CARTESIAN_POINT('Ctrl Pts',(6.99999974236211,12.522062102245,8.04447864893747));
#41290=CARTESIAN_POINT('Ctrl Pts',(6.96024020545819,12.5123170532408,8.0837285342973));
#41291=CARTESIAN_POINT('Ctrl Pts',(6.91936977290025,12.503714608425,8.1213744417));
#41292=CARTESIAN_POINT('Ctrl Pts',(6.87744629964271,12.4962259287422,8.15746842834184));
#41293=CARTESIAN_POINT('Ctrl Pts',(6.86099027054929,12.4932864315786,8.17163623573287));
#41294=CARTESIAN_POINT('Ctrl Pts',(6.84437149112919,12.4905187525983,8.18556475250955));
#41295=CARTESIAN_POINT('Ctrl Pts',(6.82759161373763,12.4879220071344,8.19925635360236));
#41296=CARTESIAN_POINT('Ctrl Pts',(6.78468135220824,12.4812814921664,8.23426913527763));
#41297=CARTESIAN_POINT('Ctrl Pts',(6.74072035702834,12.475757087696,8.26773445620468));
#41298=CARTESIAN_POINT('Ctrl Pts',(6.69574230972554,12.4713366684958,8.29968211651214));
#41299=CARTESIAN_POINT('Ctrl Pts',(6.6800137959596,12.4697908783068,8.31085399357369));
#41300=CARTESIAN_POINT('Ctrl Pts',(6.66416056770558,12.4683803043908,8.32184004829003));
#41301=CARTESIAN_POINT('Ctrl Pts',(6.64818302246812,12.4671051370951,8.33264074697925));
#41302=CARTESIAN_POINT('Ctrl Pts',(6.60309229515852,12.4635064478127,8.36312173464732));
#41303=CARTESIAN_POINT('Ctrl Pts',(6.55702091386446,12.4609871974691,8.39212045625367));
#41304=CARTESIAN_POINT('Ctrl Pts',(6.50995241026026,12.4595681035583,8.41963042001002));
#41305=CARTESIAN_POINT('Ctrl Pts',(6.47702541470063,12.4585753696636,8.43887514599639));
#41306=CARTESIAN_POINT('Ctrl Pts',(6.44360979526878,12.4581215517176,8.45739066466166));
#41307=CARTESIAN_POINT('Ctrl Pts',(6.40969282388381,12.4582216998138,8.47516391515914));
#41308=CARTESIAN_POINT('Ctrl Pts',(6.36201368421857,12.4583624840547,8.50014884919573));
#41309=CARTESIAN_POINT('Ctrl Pts',(6.31334405099426,12.4595968496478,8.52366882448567));
#41310=CARTESIAN_POINT('Ctrl Pts',(6.26366968657578,12.4619696814476,8.54566654336259));
#41311=CARTESIAN_POINT('Ctrl Pts',(6.25912282970996,12.4621868744945,8.54768006643991));
#41312=CARTESIAN_POINT('Ctrl Pts',(6.2545675471324,12.4624136250554,8.54968080571952));
#41313=CARTESIAN_POINT('Ctrl Pts',(6.25000382373019,12.4626499791555,8.55166869888726));
#41314=CARTESIAN_POINT('',(6.99999606125493,13.9487024276541,6.97712715716362));
#41315=CARTESIAN_POINT('Ctrl Pts',(6.99999606125493,13.9487024276541,6.97712715716362));
#41316=CARTESIAN_POINT('Ctrl Pts',(6.99999606606441,13.9358724268105,6.98267129810995));
#41317=CARTESIAN_POINT('Ctrl Pts',(7.00000000000004,13.9229986563094,6.9881153971666));
#41318=CARTESIAN_POINT('Ctrl Pts',(7.00000000000004,13.6749072302415,7.09781423197374));
#41319=CARTESIAN_POINT('Ctrl Pts',(7.,13.4053213379188,7.2183592608038));
#41320=CARTESIAN_POINT('Ctrl Pts',(7.,12.7992520694899,7.66953465501947));
#41321=CARTESIAN_POINT('Ctrl Pts',(7.,12.6300164231238,7.87643705196837));
#41322=CARTESIAN_POINT('Ctrl Pts',(7.,12.5220620628349,8.04447855424198));
#41323=CARTESIAN_POINT('Ctrl Pts',(6.99999606140003,13.9486969304546,6.97712309905536));
#41324=CARTESIAN_POINT('Ctrl Pts',(6.99999536779159,13.9433045112521,7.01221037447256));
#41325=CARTESIAN_POINT('Ctrl Pts',(6.99896236212046,13.9382287844098,7.04671544578038));
#41326=CARTESIAN_POINT('Ctrl Pts',(6.99701513979328,13.9334693017443,7.08055243275489));
#41327=CARTESIAN_POINT('Ctrl Pts',(6.99449897394573,13.9273191834102,7.12427598184388));
#41328=CARTESIAN_POINT('Ctrl Pts',(6.9904577666072,13.9216970366755,7.16688325413103));
#41329=CARTESIAN_POINT('Ctrl Pts',(6.98515768913276,13.9165800087812,7.20824924966308));
#41330=CARTESIAN_POINT('Ctrl Pts',(6.97960905378658,13.9112230074962,7.25155518736795));
#41331=CARTESIAN_POINT('Ctrl Pts',(6.97268032573301,13.9064197080891,7.29350069158915));
#41332=CARTESIAN_POINT('Ctrl Pts',(6.96463852783938,13.9021395728506,7.33398304499541));
#41333=CARTESIAN_POINT('Ctrl Pts',(6.96415125729609,13.9018802298715,7.33643596144504));
#41334=CARTESIAN_POINT('Ctrl Pts',(6.96365989003301,13.9016228061328,7.3388835179058));
#41335=CARTESIAN_POINT('Ctrl Pts',(6.96316448163874,13.9013672942434,7.34132569605035));
#41336=CARTESIAN_POINT('Ctrl Pts',(6.95799163377406,13.8986993456442,7.36682590183251));
#41337=CARTESIAN_POINT('Ctrl Pts',(6.95237869952793,13.8962398510606,7.39173933731414));
#41338=CARTESIAN_POINT('Ctrl Pts',(6.9463938451743,13.8939765412023,7.41605279480567));
#41339=CARTESIAN_POINT('Ctrl Pts',(6.93615532258882,13.8901046091998,7.45764677002194));
#41340=CARTESIAN_POINT('Ctrl Pts',(6.92483052998138,13.8868069446777,7.49748294940497));
#41341=CARTESIAN_POINT('Ctrl Pts',(6.91272362793161,13.8840207080244,7.53552531468417));
#41342=CARTESIAN_POINT('Ctrl Pts',(6.90315152938264,13.881817821463,7.56560280833131));
#41343=CARTESIAN_POINT('Ctrl Pts',(6.89308951924174,13.8799346003301,7.59455980286787));
#41344=CARTESIAN_POINT('Ctrl Pts',(6.8826706408791,13.8783389004979,7.62239342398978));
#41345=CARTESIAN_POINT('Ctrl Pts',(6.87533228532583,13.8772149971066,7.64199755036675));
#41346=CARTESIAN_POINT('Ctrl Pts',(6.86781666408516,13.8762336651835,7.66104471293685));
#41347=CARTESIAN_POINT('Ctrl Pts',(6.86017007183178,13.8753814225812,7.67953970156442));
#41348=CARTESIAN_POINT('Ctrl Pts',(6.85479764883003,13.8747826450332,7.69253410469556));
#41349=CARTESIAN_POINT('Ctrl Pts',(6.84936048743326,13.8742475952939,7.70525598262344));
#41350=CARTESIAN_POINT('Ctrl Pts',(6.84387352152024,13.873771654449,7.71770759717752));
#41351=CARTESIAN_POINT('Ctrl Pts',(6.84113003856374,13.8735336840265,7.72393340445457));
#41352=CARTESIAN_POINT('Ctrl Pts',(6.83837409665091,13.8733104945881,7.73009164254231));
#41353=CARTESIAN_POINT('Ctrl Pts',(6.83560747470963,13.8731015090751,7.73618264957294));
#41354=CARTESIAN_POINT('Ctrl Pts',(6.834224163739,13.8729970163186,7.73922815308825));
#41355=CARTESIAN_POINT('Ctrl Pts',(6.83283818228316,13.872896074765,7.74225684864267));
#41356=CARTESIAN_POINT('Ctrl Pts',(6.83144974880931,13.8727986130004,7.74526877931514));
#41357=CARTESIAN_POINT('Ctrl Pts',(6.83037192053051,13.872722954319,7.74760691370453));
#41358=CARTESIAN_POINT('Ctrl Pts',(6.82975121547303,13.8726804790969,7.74894835834072));
#41359=CARTESIAN_POINT('Ctrl Pts',(6.82852034694564,13.8725984441275,7.75159111902282));
#41360=CARTESIAN_POINT('Ctrl Pts',(6.8281656390886,13.8725748035456,7.75235270156179));
#41361=CARTESIAN_POINT('Ctrl Pts',(6.82776004912312,13.8725479813548,7.75322223757905));
#41362=CARTESIAN_POINT('Ctrl Pts',(6.82727730836574,13.8725165961712,7.75425432019889));
#41363=CARTESIAN_POINT('Ctrl Pts',(6.8030109284669,13.8709389278715,7.80613497986339));
#41364=CARTESIAN_POINT('Ctrl Pts',(6.7766335741503,13.8703548649644,7.85606962617251));
#41365=CARTESIAN_POINT('Ctrl Pts',(6.7484292363882,13.8708003188642,7.90384512223861));
#41366=CARTESIAN_POINT('Ctrl Pts',(6.7167315359438,13.8713009462639,7.95753804620159));
#41367=CARTESIAN_POINT('Ctrl Pts',(6.68272740983891,13.8731013428253,8.00850413011352));
#41368=CARTESIAN_POINT('Ctrl Pts',(6.64688040419033,13.8761972878495,8.05653888670308));
#41369=CARTESIAN_POINT('Ctrl Pts',(6.62069061176507,13.8784591827018,8.09163303979949));
#41370=CARTESIAN_POINT('Ctrl Pts',(6.5935158735721,13.8814130955261,8.12516272712827));
#41371=CARTESIAN_POINT('Ctrl Pts',(6.56552118186522,13.8850622912798,8.15705338823882));
#41372=CARTESIAN_POINT('Ctrl Pts',(6.5257680754455,13.8902442332231,8.2023388608633));
#41373=CARTESIAN_POINT('Ctrl Pts',(6.48436398694375,13.8968272260797,8.24431925736261));
#41374=CARTESIAN_POINT('Ctrl Pts',(6.4418307408238,13.9047546569829,8.28288850294924));
#41375=CARTESIAN_POINT('Ctrl Pts',(6.41084892356005,13.9105291096292,8.31098288623228));
#41376=CARTESIAN_POINT('Ctrl Pts',(6.37926681377584,13.9170173724247,8.33726749311037));
#41377=CARTESIAN_POINT('Ctrl Pts',(6.3472701253487,13.9242018519261,8.36170618883195));
#41378=CARTESIAN_POINT('Ctrl Pts',(6.31974251564985,13.9303828524397,8.38273145458419));
#41379=CARTESIAN_POINT('Ctrl Pts',(6.29190792468545,13.9370791086268,8.40239070177926));
#41380=CARTESIAN_POINT('Ctrl Pts',(6.26389359063877,13.9442618466046,8.42068885095676));
#41381=CARTESIAN_POINT('Ctrl Pts',(6.99933866930047,24.2330493761347,10.8743218589222));
#41382=CARTESIAN_POINT('Ctrl Pts',(6.99933866930047,24.1955798268354,10.8803485939721));
#41383=CARTESIAN_POINT('Ctrl Pts',(6.99933866930047,23.5851360656717,10.9752954456166));
#41384=CARTESIAN_POINT('Ctrl Pts',(6.99933866930047,22.3847716450475,11.0599202839285));
#41385=CARTESIAN_POINT('Ctrl Pts',(6.99933866930047,20.6450523072803,10.9047326082907));
#41386=CARTESIAN_POINT('Ctrl Pts',(6.99933866930047,18.949091407574,10.4757482566013));
#41387=CARTESIAN_POINT('Ctrl Pts',(6.99933866930047,17.3424628342019,9.78232775497157));
#41388=CARTESIAN_POINT('Ctrl Pts',(6.99933866930047,15.866963491147,8.84436513563102));
#41389=CARTESIAN_POINT('Ctrl Pts',(6.99933866930047,14.7344858431782,7.8388947861151));
#41390=CARTESIAN_POINT('Ctrl Pts',(6.99933866930047,14.1224303484372,7.13859345335349));
#41391=CARTESIAN_POINT('Ctrl Pts',(6.99933866930047,13.9057057558426,6.86526372126548));
#41392=CARTESIAN_POINT('Ctrl Pts',(7.01706607775066,24.3104707875623,11.3553300652331));
#41393=CARTESIAN_POINT('Ctrl Pts',(7.01706607775066,24.2713372052229,11.3616240778769));
#41394=CARTESIAN_POINT('Ctrl Pts',(7.01706607775066,23.6337964680017,11.4607818239098));
#41395=CARTESIAN_POINT('Ctrl Pts',(7.01706607775066,22.3805053518595,11.5491624475826));
#41396=CARTESIAN_POINT('Ctrl Pts',(7.01706607775066,20.5628206844035,11.3870392019886));
#41397=CARTESIAN_POINT('Ctrl Pts',(7.01706607775066,18.7918025555526,10.9390217567355));
#41398=CARTESIAN_POINT('Ctrl Pts',(7.01706607775066,17.1135755732343,10.2147680382133));
#41399=CARTESIAN_POINT('Ctrl Pts',(7.01706607775066,15.5722878143257,9.23492874463336));
#41400=CARTESIAN_POINT('Ctrl Pts',(7.01706607775066,14.3895391493755,8.18482486590383));
#41401=CARTESIAN_POINT('Ctrl Pts',(7.01706607775066,13.7503337411648,7.45348156383166));
#41402=CARTESIAN_POINT('Ctrl Pts',(7.01706607775066,13.5239371293929,7.16794926614792));
#41403=CARTESIAN_POINT('Ctrl Pts',(6.72659992294722,24.3728605839284,11.7429489873457));
#41404=CARTESIAN_POINT('Ctrl Pts',(6.72659992294722,24.3323860458921,11.749458384781));
#41405=CARTESIAN_POINT('Ctrl Pts',(6.72659992294722,23.6730092973298,11.8520094665702));
#41406=CARTESIAN_POINT('Ctrl Pts',(6.72659992294722,22.377067373154,11.9434166778419));
#41407=CARTESIAN_POINT('Ctrl Pts',(6.72659992294722,20.4965545945406,11.7757044254197));
#41408=CARTESIAN_POINT('Ctrl Pts',(6.72659992294722,18.6650518380346,11.3123492226921));
#41409=CARTESIAN_POINT('Ctrl Pts',(6.72659992294722,16.9291275072387,10.563248655114));
#41410=CARTESIAN_POINT('Ctrl Pts',(6.72659992294722,15.3348243641778,9.54966317775517));
#41411=CARTESIAN_POINT('Ctrl Pts',(6.72659992294722,14.111564961231,8.46359151249178));
#41412=CARTESIAN_POINT('Ctrl Pts',(6.72659992294722,13.4504808822296,7.70723313889616));
#41413=CARTESIAN_POINT('Ctrl Pts',(6.72659992294722,13.2162901047889,7.41186744281947));
#41414=CARTESIAN_POINT('Ctrl Pts',(6.25333238742997,24.3925555985452,11.8653113090695));
#41415=CARTESIAN_POINT('Ctrl Pts',(6.25333238742997,24.3516577518376,11.8718886985001));
#41416=CARTESIAN_POINT('Ctrl Pts',(6.25333238742997,23.6853878799162,11.9755109778418));
#41417=CARTESIAN_POINT('Ctrl Pts',(6.25333238742997,22.3759820828512,12.0678736127627));
#41418=CARTESIAN_POINT('Ctrl Pts',(6.25333238742997,20.4756359237962,11.8983970402517));
#41419=CARTESIAN_POINT('Ctrl Pts',(6.25333238742997,18.6250395703447,11.4302000625049));
#41420=CARTESIAN_POINT('Ctrl Pts',(6.25333238742997,16.8709015221175,10.6732559197938));
#41421=CARTESIAN_POINT('Ctrl Pts',(6.25333238742997,15.2598626493954,9.64901755331904));
#41422=CARTESIAN_POINT('Ctrl Pts',(6.25333238742997,14.0238149441382,8.55159169037091));
#41423=CARTESIAN_POINT('Ctrl Pts',(6.25333238742997,13.3558242751811,7.78733663770481));
#41424=CARTESIAN_POINT('Ctrl Pts',(6.25333238742997,13.1191730600493,7.48886676536423));
#41425=CARTESIAN_POINT('',(7.,24.1259420764688,10.92778018982));
#41426=CARTESIAN_POINT('Ctrl Pts',(7.00000000000002,24.1259420781411,10.9277802009508));
#41427=CARTESIAN_POINT('Ctrl Pts',(7.00000000000002,23.9636071437087,10.9521697339675));
#41428=CARTESIAN_POINT('Ctrl Pts',(7.00000000006073,23.8012468343643,10.9728907888933));
#41429=CARTESIAN_POINT('Ctrl Pts',(6.99999999867344,23.6387645225613,10.989991664534));
#41430=CARTESIAN_POINT('Ctrl Pts',(6.99999999728331,23.4759486337289,11.0071276483612));
#41431=CARTESIAN_POINT('Ctrl Pts',(6.99999999422997,23.3130097833915,11.0206285917113));
#41432=CARTESIAN_POINT('Ctrl Pts',(6.99999999314808,23.1498443962042,11.0304911374634));
#41433=CARTESIAN_POINT('Ctrl Pts',(6.99999999207001,22.987253229421,11.0403189744142));
#41434=CARTESIAN_POINT('Ctrl Pts',(6.9999999947222,22.8244366655206,11.0465339774628));
#41435=CARTESIAN_POINT('Ctrl Pts',(6.99999999803543,22.6612927248816,11.0490812228026));
#41436=CARTESIAN_POINT('Ctrl Pts',(6.99999999907234,22.6102348488692,11.0498784141431));
#41437=CARTESIAN_POINT('Ctrl Pts',(7.00000000000002,22.5591449386156,11.0503159845158));
#41438=CARTESIAN_POINT('Ctrl Pts',(7.00000000000002,22.5080199866575,11.0503912040686));
#41439=CARTESIAN_POINT('Ctrl Pts',(7.00000000000002,22.4670944974344,11.0504514172694));
#41440=CARTESIAN_POINT('Ctrl Pts',(6.99999999938402,22.4261461216709,11.0502844809917));
#41441=CARTESIAN_POINT('Ctrl Pts',(6.9999999984721,22.3851800827051,11.04988913167));
#41442=CARTESIAN_POINT('Ctrl Pts',(6.99999999416127,22.1915272268588,11.0480202537617));
#41443=CARTESIAN_POINT('Ctrl Pts',(6.99999998574681,21.9974791816599,11.0410431158288));
#41444=CARTESIAN_POINT('Ctrl Pts',(6.99999998500532,21.8035299183916,11.0289289304663));
#41445=CARTESIAN_POINT('Ctrl Pts',(6.99999998426226,21.6091706679596,11.0167891370638));
#41446=CARTESIAN_POINT('Ctrl Pts',(6.99999998984224,21.4149110357627,10.9994905471205));
#41447=CARTESIAN_POINT('Ctrl Pts',(6.99999999473001,21.221250784181,10.9770564362198));
#41448=CARTESIAN_POINT('Ctrl Pts',(6.99999999759809,21.1076129763808,10.9638923348521));
#41449=CARTESIAN_POINT('Ctrl Pts',(7.00000000000002,20.9941815671557,10.9489609450939));
#41450=CARTESIAN_POINT('Ctrl Pts',(7.00000000000002,20.881057063376,10.932275312452));
#41451=CARTESIAN_POINT('Ctrl Pts',(7.00000000000002,20.8030386971055,10.9207677631995));
#41452=CARTESIAN_POINT('Ctrl Pts',(6.99999999890227,20.7251678797296,10.9084197072691));
#41453=CARTESIAN_POINT('Ctrl Pts',(6.99999999758225,20.6474551518283,10.8952337790289));
#41454=CARTESIAN_POINT('Ctrl Pts',(6.99999999346296,20.4049430664632,10.8540854749948));
#41455=CARTESIAN_POINT('Ctrl Pts',(6.9999999892588,20.1639700234044,10.8047816167284));
#41456=CARTESIAN_POINT('Ctrl Pts',(6.99999999152161,19.9249049441579,10.7474302395335));
#41457=CARTESIAN_POINT('Ctrl Pts',(6.99999999354309,19.7113353073924,10.6961951832294));
#41458=CARTESIAN_POINT('Ctrl Pts',(7.00000000000002,19.499288118559,10.6385367924637));
#41459=CARTESIAN_POINT('Ctrl Pts',(7.00000000000002,19.2890338727372,10.5744977121983));
#41460=CARTESIAN_POINT('Ctrl Pts',(7.00000000000002,19.1765541929259,10.5402387358075));
#41461=CARTESIAN_POINT('Ctrl Pts',(6.99999999803037,19.0645809749219,10.5041682245751));
#41462=CARTESIAN_POINT('Ctrl Pts',(6.99999999636324,18.9531931449385,10.4663010056192));
#41463=CARTESIAN_POINT('Ctrl Pts',(6.99999999271541,18.709465928779,10.3834439119742));
#41464=CARTESIAN_POINT('Ctrl Pts',(6.99999999204987,18.4685424549483,10.2919812981329));
#41465=CARTESIAN_POINT('Ctrl Pts',(6.99999999506635,18.2311664503793,10.19223200664));
#41466=CARTESIAN_POINT('Ctrl Pts',(6.99999999705716,18.0745037563495,10.1263997724123));
#41467=CARTESIAN_POINT('Ctrl Pts',(7.00000000000002,17.9193859910228,10.056959169959));
#41468=CARTESIAN_POINT('Ctrl Pts',(7.00000000000002,17.7660225335621,9.9840134765408));
#41469=CARTESIAN_POINT('Ctrl Pts',(7.00000000000002,17.6246298314655,9.91676154528239));
#41470=CARTESIAN_POINT('Ctrl Pts',(6.99999999722481,17.4847359912375,9.84651984572386));
#41471=CARTESIAN_POINT('Ctrl Pts',(6.99999999446473,17.3464266497251,9.77332726001044));
#41472=CARTESIAN_POINT('Ctrl Pts',(6.9999999900828,17.1268453052524,9.6571259521259));
#41473=CARTESIAN_POINT('Ctrl Pts',(6.99999998784248,16.9112559387415,9.53348886601782));
#41474=CARTESIAN_POINT('Ctrl Pts',(6.99999999262692,16.7000168930179,9.40257873636276));
#41475=CARTESIAN_POINT('Ctrl Pts',(6.99999999531398,16.58137961056,9.32905623972729));
#41476=CARTESIAN_POINT('Ctrl Pts',(7.00000000000002,16.4641150846931,9.25323890923894));
#41477=CARTESIAN_POINT('Ctrl Pts',(7.00000000000002,16.3482916764188,9.17515025230581));
#41478=CARTESIAN_POINT('Ctrl Pts',(7.00000000000002,16.1866097165453,9.06614355594835));
#41479=CARTESIAN_POINT('Ctrl Pts',(6.9999999901482,16.0276912247442,8.9527563196008));
#41480=CARTESIAN_POINT('Ctrl Pts',(6.99999998525263,15.8719358528285,8.83523144981877));
#41481=CARTESIAN_POINT('Ctrl Pts',(6.99999998003391,15.7058991336856,8.70994881233221));
#41482=CARTESIAN_POINT('Ctrl Pts',(6.99999998145009,15.5434575723926,8.5799641511856));
#41483=CARTESIAN_POINT('Ctrl Pts',(6.99999998835947,15.3849965664812,8.44567633217485));
#41484=CARTESIAN_POINT('Ctrl Pts',(6.99999999308645,15.2765870454925,8.35380465655442));
#41485=CARTESIAN_POINT('Ctrl Pts',(7.00000000000002,15.170039918213,8.25991974581256));
#41486=CARTESIAN_POINT('Ctrl Pts',(7.00000000000002,15.0654684156701,8.1641590081593));
#41487=CARTESIAN_POINT('Ctrl Pts',(7.00000000000002,14.9424780843168,8.05153133648764));
#41488=CARTESIAN_POINT('Ctrl Pts',(6.99999999283352,14.822282594585,7.9362684620195));
#41489=CARTESIAN_POINT('Ctrl Pts',(6.99999999157257,14.7047659435611,7.81832386853829));
#41490=CARTESIAN_POINT('Ctrl Pts',(6.99999999107894,14.6587611849019,7.77215158136899));
#41491=CARTESIAN_POINT('Ctrl Pts',(6.99999999110871,14.6131673062471,7.72556786584807));
#41492=CARTESIAN_POINT('Ctrl Pts',(6.99999999149981,14.5679787260292,7.67856824982574));
#41493=CARTESIAN_POINT('Ctrl Pts',(6.99999999249457,14.453039403995,7.55902247132562));
#41494=CARTESIAN_POINT('Ctrl Pts',(6.99999999551026,14.3407195515746,7.43678843307566));
#41495=CARTESIAN_POINT('Ctrl Pts',(6.99999999717045,14.2309770599541,7.31179318524976));
#41496=CARTESIAN_POINT('Ctrl Pts',(6.99999999862373,14.1349114849696,7.2023757647465));
#41497=CARTESIAN_POINT('Ctrl Pts',(6.99999999923215,14.0408212492114,7.09084181894597));
#41498=CARTESIAN_POINT('Ctrl Pts',(6.99999999922773,13.9487034978523,6.97712164368536));
#41499=CARTESIAN_POINT('',(6.27159471697284,24.2690139179361,11.8794981306053));
#41500=CARTESIAN_POINT('Origin',(5.999999877385,24.1259420367213,10.9277801432448));
#41501=CARTESIAN_POINT('Ctrl Pts',(6.27159470457053,24.26901364136,11.8794980693503));
#41502=CARTESIAN_POINT('Ctrl Pts',(6.2719396690107,24.039518107917,11.9138782735934));
#41503=CARTESIAN_POINT('Ctrl Pts',(6.27225782568409,23.8113319140033,11.941274195107));
#41504=CARTESIAN_POINT('Ctrl Pts',(6.27254917030223,23.5849163742437,11.9620370266173));
#41505=CARTESIAN_POINT('Ctrl Pts',(6.27284515820514,23.3548923524162,11.9831307643245));
#41506=CARTESIAN_POINT('Ctrl Pts',(6.27311347261641,23.1266958261604,11.9973783297609));
#41507=CARTESIAN_POINT('Ctrl Pts',(6.27335410997358,22.9007562998605,12.0051465943053));
#41508=CARTESIAN_POINT('Ctrl Pts',(6.27354178810334,22.7245413171485,12.0112052270059));
#41509=CARTESIAN_POINT('Ctrl Pts',(6.27371263094327,22.5496981016224,12.0133226279267));
#41510=CARTESIAN_POINT('Ctrl Pts',(6.2738666371627,22.3764084710344,12.0116720903062));
#41511=CARTESIAN_POINT('Ctrl Pts',(6.2740686874815,22.1490590481532,12.009506647549));
#41512=CARTESIAN_POINT('Ctrl Pts',(6.27424175783396,21.9243852735233,12.0008569230838));
#41513=CARTESIAN_POINT('Ctrl Pts',(6.27438584596713,21.7027333503043,11.9862082337932));
#41514=CARTESIAN_POINT('Ctrl Pts',(6.27447251904989,21.5694034565529,11.9773966333418));
#41515=CARTESIAN_POINT('Ctrl Pts',(6.27454870533157,21.4371659929971,11.9664140729929));
#41516=CARTESIAN_POINT('Ctrl Pts',(6.27461440446078,21.3060877225297,11.9533633529954));
#41517=CARTESIAN_POINT('Ctrl Pts',(6.27472591349752,21.0836127544107,11.931212782157));
#41518=CARTESIAN_POINT('Ctrl Pts',(6.27480721195824,20.8644797540508,11.903105353766));
#41519=CARTESIAN_POINT('Ctrl Pts',(6.27485829878145,20.6489747471807,11.8695299304313));
#41520=CARTESIAN_POINT('Ctrl Pts',(6.27487121247856,20.5944995183722,11.8610427546804));
#41521=CARTESIAN_POINT('Ctrl Pts',(6.27488219573365,20.5402558626649,11.8522061026172));
#41522=CARTESIAN_POINT('Ctrl Pts',(6.27489124853762,20.4862479066121,11.8430276976365));
#41523=CARTESIAN_POINT('Ctrl Pts',(6.274928126599,20.2662377612205,11.8056379802344));
#41524=CARTESIAN_POINT('Ctrl Pts',(6.27493296929566,20.0501427221489,11.7625788981377));
#41525=CARTESIAN_POINT('Ctrl Pts',(6.2749057765612,19.8381869495583,11.7143943058079));
#41526=CARTESIAN_POINT('Ctrl Pts',(6.2748825774797,19.6573599992307,11.6732863294727));
#41527=CARTESIAN_POINT('Ctrl Pts',(6.27483606174957,19.4795448826768,11.6284473784717));
#41528=CARTESIAN_POINT('Ctrl Pts',(6.27476622983678,19.3048541889533,11.5802014292858));
#41529=CARTESIAN_POINT('Ctrl Pts',(6.27472435185361,19.2000927175969,11.5512684820523));
#41530=CARTESIAN_POINT('Ctrl Pts',(6.27467408860072,19.0964544407097,11.5211100139507));
#41531=CARTESIAN_POINT('Ctrl Pts',(6.27461544159147,18.9939596224219,11.4897937642906));
#41532=CARTESIAN_POINT('Ctrl Pts',(6.27458611808684,18.942712213278,11.4741356394605));
#41533=CARTESIAN_POINT('Ctrl Pts',(6.27455469601115,18.89175067152,11.4581880604393));
#41534=CARTESIAN_POINT('Ctrl Pts',(6.27452117880938,18.8410772027574,11.4419593294567));
#41535=CARTESIAN_POINT('Ctrl Pts',(6.27450442020849,18.8157404683761,11.4338449639654));
#41536=CARTESIAN_POINT('Ctrl Pts',(6.27448713764832,18.7904757524208,11.4256603098872));
#41537=CARTESIAN_POINT('Ctrl Pts',(6.27446933112943,18.7652833218196,11.4174063983605));
#41538=CARTESIAN_POINT('Ctrl Pts',(6.27445391930054,18.743478867389,11.4102625049979));
#41539=CARTESIAN_POINT('Ctrl Pts',(6.27443872964694,18.7225457056324,11.403338948886));
#41540=CARTESIAN_POINT('Ctrl Pts',(6.27442216592055,18.7003621707754,11.3959298239849));
#41541=CARTESIAN_POINT('Ctrl Pts',(6.27441959224871,18.6969152930875,11.3947785941438));
#41542=CARTESIAN_POINT('Ctrl Pts',(6.27441698540273,18.6934382597025,11.3936155447334));
#41543=CARTESIAN_POINT('Ctrl Pts',(6.27441433939461,18.6899231479741,11.3924379185985));
#41544=CARTESIAN_POINT('Ctrl Pts',(6.27440279742353,18.6745901195145,11.3873010761774));
#41545=CARTESIAN_POINT('Ctrl Pts',(6.27439106562786,18.6592579780417,11.382129846888));
#41546=CARTESIAN_POINT('Ctrl Pts',(6.27437914400858,18.6439268888218,11.3769241436729));
#41547=CARTESIAN_POINT('Ctrl Pts',(6.27420011122339,18.4136924266768,11.2987475534373));
#41548=CARTESIAN_POINT('Ctrl Pts',(6.27397826832473,18.1836911572812,11.2127950683308));
#41549=CARTESIAN_POINT('Ctrl Pts',(6.27371361959025,17.9544926702115,11.1188688297047));
#41550=CARTESIAN_POINT('Ctrl Pts',(6.27345239281417,17.7282577631024,11.0261570751799));
#41551=CARTESIAN_POINT('Ctrl Pts',(6.27314946001023,17.5028049754159,10.925676404779));
#41552=CARTESIAN_POINT('Ctrl Pts',(6.27280482713072,17.2787307745671,10.8172504627899));
#41553=CARTESIAN_POINT('Ctrl Pts',(6.27260798324538,17.1507463629782,10.7553208415578));
#41554=CARTESIAN_POINT('Ctrl Pts',(6.27239753537388,17.0232125920257,10.6907994538667));
#41555=CARTESIAN_POINT('Ctrl Pts',(6.27217348492361,16.8962479574614,10.6236555852893));
#41556=CARTESIAN_POINT('Ctrl Pts',(6.27177013690949,16.6676791991513,10.5027794789503));
#41557=CARTESIAN_POINT('Ctrl Pts',(6.27132270387729,16.4409516512944,10.3734026114263));
#41558=CARTESIAN_POINT('Ctrl Pts',(6.2708311960293,16.2167886981205,10.2354141987361));
#41559=CARTESIAN_POINT('Ctrl Pts',(6.27036732517286,16.0052302021626,10.1051847355933));
#41560=CARTESIAN_POINT('Ctrl Pts',(6.26986419786731,15.7959563703179,9.96728507323921));
#41561=CARTESIAN_POINT('Ctrl Pts',(6.26932182415434,15.5896233810682,9.82164183491594));
#41562=CARTESIAN_POINT('Ctrl Pts',(6.26905884857566,15.4895806689094,9.75102518450816));
#41563=CARTESIAN_POINT('Ctrl Pts',(6.26878664660819,15.3902300307254,9.67858839365913));
#41564=CARTESIAN_POINT('Ctrl Pts',(6.26850521961789,15.2916503517775,9.60432480011758));
#41565=CARTESIAN_POINT('Ctrl Pts',(6.26791729668106,15.0857097122666,9.44918235991527));
#41566=CARTESIAN_POINT('Ctrl Pts',(6.26728911325593,14.8831313073574,9.28606507446861));
#41567=CARTESIAN_POINT('Ctrl Pts',(6.26662068408126,14.684548134728,9.11502581381811));
#41568=CARTESIAN_POINT('Ctrl Pts',(6.26595956673244,14.488137227508,8.94585752070546));
#41569=CARTESIAN_POINT('Ctrl Pts',(6.2652590792745,14.2956345992665,8.76893957558176));
#41570=CARTESIAN_POINT('Ctrl Pts',(6.2645192393273,14.1076929658034,8.5843545277584));
#41571=CARTESIAN_POINT('Ctrl Pts',(6.26430323424039,14.0528211668106,8.53046272393284));
#41572=CARTESIAN_POINT('Ctrl Pts',(6.26408387470152,13.9983384205356,8.47591757105517));
#41573=CARTESIAN_POINT('Ctrl Pts',(6.26386116120914,13.9442616338432,8.42072164456287));
#41574=CARTESIAN_POINT('Ctrl Pts',(6.99999999998952,24.7867299441601,9.33248386901283));
#41575=CARTESIAN_POINT('Ctrl Pts',(6.99999999998952,24.7867268023266,9.33249195739188));
#41576=CARTESIAN_POINT('Ctrl Pts',(6.99999999998952,24.68190835415,9.60233773525705));
#41577=CARTESIAN_POINT('Ctrl Pts',(6.99999999998952,24.4674877122422,10.1365860426111));
#41578=CARTESIAN_POINT('Ctrl Pts',(6.99999999998952,24.2412750070288,10.6659267308771));
#41579=CARTESIAN_POINT('Ctrl Pts',(6.99999999998952,24.1259369154038,10.9277807259288));
#41580=CARTESIAN_POINT('Ctrl Pts',(7.00000270566332,25.3377021368914,9.54650237055708));
#41581=CARTESIAN_POINT('Ctrl Pts',(7.00000270566332,25.33769894728,9.5465105819364));
#41582=CARTESIAN_POINT('Ctrl Pts',(7.00000270566332,25.2312865215935,9.8204599139257));
#41583=CARTESIAN_POINT('Ctrl Pts',(7.00000270566332,25.0136084416684,10.362824287923));
#41584=CARTESIAN_POINT('Ctrl Pts',(7.00000270566332,24.7839592082931,10.9002066230296));
#41585=CARTESIAN_POINT('Ctrl Pts',(7.00000270566332,24.6668671666914,11.1660426394581));
#41586=CARTESIAN_POINT('Ctrl Pts',(6.57967197777962,25.725143338898,9.69699923153085));
#41587=CARTESIAN_POINT('Ctrl Pts',(6.57967197777962,25.7251401156893,9.69700752940341));
#41588=CARTESIAN_POINT('Ctrl Pts',(6.57967197777962,25.617606812089,9.97384246245126));
#41589=CARTESIAN_POINT('Ctrl Pts',(6.57967197777962,25.3976381162041,10.5219140185141));
#41590=CARTESIAN_POINT('Ctrl Pts',(6.57967197777962,25.1655723314695,11.0649512040096));
#41591=CARTESIAN_POINT('Ctrl Pts',(6.57967197777962,25.0472469200172,11.3335873602045));
#41592=CARTESIAN_POINT('Ctrl Pts',(5.98852435812819,25.7188194279223,9.69454278460176));
#41593=CARTESIAN_POINT('Ctrl Pts',(5.98852435812819,25.718816205262,9.69455108106255));
#41594=CARTESIAN_POINT('Ctrl Pts',(5.98852435812819,25.6113011969081,9.97133891461738));
#41595=CARTESIAN_POINT('Ctrl Pts',(5.98852435812819,25.3913698890145,10.5193173166418));
#41596=CARTESIAN_POINT('Ctrl Pts',(5.98852435812819,25.1593435478338,11.0622622022752));
#41597=CARTESIAN_POINT('Ctrl Pts',(5.98852435812819,25.0410382677488,11.3308526538974));
#41598=CARTESIAN_POINT('',(6.99999999994009,24.7867180661821,9.33250873276066));
#41599=CARTESIAN_POINT('',(5.98852583812743,25.7188097531253,9.69456766830281));
#41600=CARTESIAN_POINT('Origin',(5.999999999061,24.7867247845918,9.33250979146072));
#41601=CARTESIAN_POINT('',(5.9885258135532,25.0410389643412,11.3308503205391));
#41602=CARTESIAN_POINT('Origin',(5.98846855808858,-11.4751154935115,-4.75314843118749));
#41603=CARTESIAN_POINT('Origin',(6.,24.1259421517583,10.9277801936249));
#41604=CARTESIAN_POINT('Origin',(6.99999997874242,-11.4664779467208,-4.74946027036764));
#41605=CARTESIAN_POINT('Origin',(5.999999877385,24.1259420367213,10.9277801432448));
#41606=CARTESIAN_POINT('Origin',(5.99999764421527,24.1259401206149,10.9277792069261));
#41607=CARTESIAN_POINT('Ctrl Pts',(-6.09415743589287,25.0685176670397,11.2705948926489));
#41608=CARTESIAN_POINT('Ctrl Pts',(-6.05606588732271,25.0626152520279,11.2828610723339));
#41609=CARTESIAN_POINT('Ctrl Pts',(-5.71207088618283,25.0098877697791,11.3926635700215));
#41610=CARTESIAN_POINT('Ctrl Pts',(-5.02599367392107,24.9149190577036,11.5942416721674));
#41611=CARTESIAN_POINT('Ctrl Pts',(-3.98564775783899,24.7979400134299,11.8483582951752));
#41612=CARTESIAN_POINT('Ctrl Pts',(-2.81213472137221,24.6988235435346,12.0680547776604));
#41613=CARTESIAN_POINT('Ctrl Pts',(-1.52041606170006,24.629776117468,12.2244388462329));
#41614=CARTESIAN_POINT('Ctrl Pts',(-0.18938368979716,24.6028735621445,12.2876144937024));
#41615=CARTESIAN_POINT('Ctrl Pts',(1.08604876859294,24.6176047392936,12.2527453884866));
#41616=CARTESIAN_POINT('Ctrl Pts',(2.24115591625819,24.6651918941777,12.143937035736));
#41617=CARTESIAN_POINT('Ctrl Pts',(3.27282426521286,24.735605003468,11.9862434179946));
#41618=CARTESIAN_POINT('Ctrl Pts',(4.19977149222157,24.8213849139756,11.797279536956));
#41619=CARTESIAN_POINT('Ctrl Pts',(5.05677934758209,24.9199603491257,11.5836987166178));
#41620=CARTESIAN_POINT('Ctrl Pts',(5.68020727784929,25.0054672272717,11.4020597285418));
#41621=CARTESIAN_POINT('Ctrl Pts',(6.02208888462226,25.0573454648108,11.2938086928354));
#41622=CARTESIAN_POINT('Ctrl Pts',(6.09402271352824,25.0684922274053,11.2706461600882));
#41623=CARTESIAN_POINT('Ctrl Pts',(-6.21832045053098,24.9356363004755,11.6022681603765));
#41624=CARTESIAN_POINT('Ctrl Pts',(-6.17949927506643,24.9295088225807,11.6147172343648));
#41625=CARTESIAN_POINT('Ctrl Pts',(-5.82891139943057,24.8747368508288,11.726143286659));
#41626=CARTESIAN_POINT('Ctrl Pts',(-5.12960176764218,24.7754946259934,11.9304638300121));
#41627=CARTESIAN_POINT('Ctrl Pts',(-4.06864373240013,24.6520241911184,12.1875933298324));
#41628=CARTESIAN_POINT('Ctrl Pts',(-2.87116826711582,24.5463532301321,12.4094995450073));
#41629=CARTESIAN_POINT('Ctrl Pts',(-1.55239219352023,24.4718951869516,12.5670902012212));
#41630=CARTESIAN_POINT('Ctrl Pts',(-0.193327228898783,24.4423488465848,
12.6304801584094));
#41631=CARTESIAN_POINT('Ctrl Pts',(1.10884029560539,24.458591025936,12.595525156871));
#41632=CARTESIAN_POINT('Ctrl Pts',(2.28827733619991,24.5101590878462,12.4860015055859));
#41633=CARTESIAN_POINT('Ctrl Pts',(3.34130595899083,24.5856379456193,12.3268930309681));
#41634=CARTESIAN_POINT('Ctrl Pts',(4.28702500002799,24.6768035896854,12.1359205564239));
#41635=CARTESIAN_POINT('Ctrl Pts',(5.16096421537736,24.7807262870167,11.9197644114018));
#41636=CARTESIAN_POINT('Ctrl Pts',(5.79643509966697,24.8701221577978,11.7356686956827));
#41637=CARTESIAN_POINT('Ctrl Pts',(6.14487117451663,24.9240358177971,11.6258273593906));
#41638=CARTESIAN_POINT('Ctrl Pts',(6.21818308061221,24.935607236778,11.6023191866738));
#41639=CARTESIAN_POINT('Ctrl Pts',(-6.32908148189132,24.6417686601331,11.8134211097232));
#41640=CARTESIAN_POINT('Ctrl Pts',(-6.28955536353039,24.6354614716029,11.8259897628201));
#41641=CARTESIAN_POINT('Ctrl Pts',(-5.9326099399111,24.5790644008174,11.9384537675389));
#41642=CARTESIAN_POINT('Ctrl Pts',(-5.22075534857246,24.4765500531428,12.1441201140726));
#41643=CARTESIAN_POINT('Ctrl Pts',(-4.14076534440852,24.3483246298362,12.4018806751728));
#41644=CARTESIAN_POINT('Ctrl Pts',(-2.92177802351305,24.2380190316229,12.623417756821));
#41645=CARTESIAN_POINT('Ctrl Pts',(-1.57939308859398,24.1598585351471,12.7799736491164));
#41646=CARTESIAN_POINT('Ctrl Pts',(-0.196603179997715,24.1285646331443,
12.8424291350917));
#41647=CARTESIAN_POINT('Ctrl Pts',(1.12799353750622,24.145800396657,12.8080494910814));
#41648=CARTESIAN_POINT('Ctrl Pts',(2.32845047098897,24.2000621596312,12.6994858356328));
#41649=CARTESIAN_POINT('Ctrl Pts',(3.40035685412353,24.2790638500178,12.541010654418));
#41650=CARTESIAN_POINT('Ctrl Pts',(4.36306687247048,24.37407672428,12.3501091583462));
#41651=CARTESIAN_POINT('Ctrl Pts',(5.25267862906944,24.4819336875387,12.1333190695919));
#41652=CARTESIAN_POINT('Ctrl Pts',(5.89955400274272,24.5743007947612,11.9480450763936));
#41653=CARTESIAN_POINT('Ctrl Pts',(6.25429750719079,24.6298264279853,11.8372049534228));
#41654=CARTESIAN_POINT('Ctrl Pts',(6.32894084676985,24.6417369929965,11.8134705227596));
#41655=CARTESIAN_POINT('Ctrl Pts',(-6.3948835653583,24.2701531214398,11.8436584888777));
#41656=CARTESIAN_POINT('Ctrl Pts',(-6.35487788326796,24.2637628345041,11.8562492153957));
#41657=CARTESIAN_POINT('Ctrl Pts',(-5.99362024492343,24.2066236152637,11.9688687058286));
#41658=CARTESIAN_POINT('Ctrl Pts',(-5.27348028276714,24.1027722982909,12.1740977236281));
#41659=CARTESIAN_POINT('Ctrl Pts',(-4.18145907214454,23.9728859143447,12.4299220155458));
#41660=CARTESIAN_POINT('Ctrl Pts',(-2.94953904132581,23.8611893602657,12.6486097593309));
#41661=CARTESIAN_POINT('Ctrl Pts',(-1.59372167501731,23.7820925676294,12.8021784804847));
#41662=CARTESIAN_POINT('Ctrl Pts',(-0.198277517951755,23.7504469244805,
12.8628138246229));
#41663=CARTESIAN_POINT('Ctrl Pts',(1.13804826101955,23.7678747864035,12.8295086797204));
#41664=CARTESIAN_POINT('Ctrl Pts',(2.35022440053216,23.822773196571,12.7233112457001));
#41665=CARTESIAN_POINT('Ctrl Pts',(3.43314706917537,23.9027483421861,12.5673423471683));
#41666=CARTESIAN_POINT('Ctrl Pts',(4.40622700507742,23.9989711658464,12.3785763590503));
#41667=CARTESIAN_POINT('Ctrl Pts',(5.30578879644537,24.1082261614275,12.163278950266));
#41668=CARTESIAN_POINT('Ctrl Pts',(5.96018277708729,24.201798828066,11.9784436509294));
#41669=CARTESIAN_POINT('Ctrl Pts',(6.31919090105992,24.2580531508172,11.8674819873968));
#41670=CARTESIAN_POINT('Ctrl Pts',(6.39473997516368,24.2701206149759,11.8437053722807));
#41671=CARTESIAN_POINT('',(-5.98852245733775,25.0410395152739,11.3308498383567));
#41672=CARTESIAN_POINT('Ctrl Pts',(-5.98852261949159,25.0410393033428,11.3308502493368));
#41673=CARTESIAN_POINT('Ctrl Pts',(-5.87207793491996,25.0233585862853,11.367676505058));
#41674=CARTESIAN_POINT('Ctrl Pts',(-5.74893720729897,25.0052500193778,11.4056119122923));
#41675=CARTESIAN_POINT('Ctrl Pts',(-5.6190981775558,24.986894679695,11.4442931780282));
#41676=CARTESIAN_POINT('Ctrl Pts',(-5.51159709980728,24.9716972556058,11.4763195861391));
#41677=CARTESIAN_POINT('Ctrl Pts',(-5.3995042185231,24.9563309052265,11.508856518002));
#41678=CARTESIAN_POINT('Ctrl Pts',(-5.28282127163981,24.9409034536848,11.5416713122482));
#41679=CARTESIAN_POINT('Ctrl Pts',(-5.21054205127972,24.9313469229375,11.5619984278014));
#41680=CARTESIAN_POINT('Ctrl Pts',(-5.13650113482633,24.9217682042197,11.582429041541));
#41681=CARTESIAN_POINT('Ctrl Pts',(-5.06069864646884,24.9121968136603,11.6028960441539));
#41682=CARTESIAN_POINT('Ctrl Pts',(-5.00141638199723,24.90471139044,11.6189025142333));
#41683=CARTESIAN_POINT('Ctrl Pts',(-4.94105673142941,24.8972304452503,11.6349311595742));
#41684=CARTESIAN_POINT('Ctrl Pts',(-4.87961956272349,24.8897694846537,11.6509486356637));
#41685=CARTESIAN_POINT('Ctrl Pts',(-4.80962202785255,24.8812689488946,11.6691979115456));
#41686=CARTESIAN_POINT('Ctrl Pts',(-4.73822586615999,24.872794473703,11.6874324435812));
#41687=CARTESIAN_POINT('Ctrl Pts',(-4.66543107683349,24.8643703477828,11.7055991591889));
#41688=CARTESIAN_POINT('Ctrl Pts',(-4.62903368217023,24.8601582848227,11.7146825169927));
#41689=CARTESIAN_POINT('Ctrl Pts',(-4.59228663064168,24.8559588042056,11.7237489184915));
#41690=CARTESIAN_POINT('Ctrl Pts',(-4.55518992231137,24.8517750652626,11.7327913774651));
#41691=CARTESIAN_POINT('Ctrl Pts',(-4.53664156814622,24.8496831957911,11.7373126069519));
#41692=CARTESIAN_POINT('Ctrl Pts',(-4.51800579978205,24.8475952614153,11.7418278506626));
#41693=CARTESIAN_POINT('Ctrl Pts',(-4.49928261723233,24.8455116586679,11.7463362265013));
#41694=CARTESIAN_POINT('Ctrl Pts',(-4.48992102595747,24.8444698572942,11.7485904144207));
#41695=CARTESIAN_POINT('Ctrl Pts',(-4.48053758113626,24.8434291388063,11.7508428853625));
#41696=CARTESIAN_POINT('Ctrl Pts',(-4.47113228277049,24.8423895531611,11.7530935278688));
#41697=CARTESIAN_POINT('Ctrl Pts',(-4.46172698440472,24.8413499675159,11.7553441703752));
#41698=CARTESIAN_POINT('Ctrl Pts',(-4.45105740215062,24.8401751261721,11.7578884213725));
#41699=CARTESIAN_POINT('Ctrl Pts',(-4.44285082704132,24.8392742447742,11.7598398582553));
#41700=CARTESIAN_POINT('Ctrl Pts',(-4.30874234749329,24.82455241101,11.7917294382317));
#41701=CARTESIAN_POINT('Ctrl Pts',(-4.17030708102564,24.8100278948711,11.8233188134517));
#41702=CARTESIAN_POINT('Ctrl Pts',(-4.02753713404441,24.7958393518128,11.854288220348));
#41703=CARTESIAN_POINT('Ctrl Pts',(-3.89073584503476,24.7822439767314,11.8839629164088));
#41704=CARTESIAN_POINT('Ctrl Pts',(-3.74995452320826,24.7689570371205,11.9130681133127));
#41705=CARTESIAN_POINT('Ctrl Pts',(-3.60520088693431,24.7561100633647,11.9413069555636));
#41706=CARTESIAN_POINT('Ctrl Pts',(-3.45728944070361,24.7429828320437,11.9701618299883));
#41707=CARTESIAN_POINT('Ctrl Pts',(-3.30522643392144,24.7303154547137,11.9981112189699));
#41708=CARTESIAN_POINT('Ctrl Pts',(-3.14901186672775,24.7182538149112,12.024819615501));
#41709=CARTESIAN_POINT('Ctrl Pts',(-3.07090458313091,24.7122229950099,12.0381738137665));
#41710=CARTESIAN_POINT('Ctrl Pts',(-2.99175940932096,24.7063436716989,12.0512175142174));
#41711=CARTESIAN_POINT('Ctrl Pts',(-2.91157634444144,24.700634331209,12.063907458552));
#41712=CARTESIAN_POINT('Ctrl Pts',(-2.89518327517228,24.6994670820614,12.0665018609587));
#41713=CARTESIAN_POINT('Ctrl Pts',(-2.87874682718898,24.6983069354887,12.0690814800435));
#41714=CARTESIAN_POINT('Ctrl Pts',(-2.86226699502409,24.6971540534798,12.0716459347082));
#41715=CARTESIAN_POINT('Ctrl Pts',(-2.8384431040123,24.6954874020809,12.0753532108399));
#41716=CARTESIAN_POINT('Ctrl Pts',(-2.81452854523531,24.6938359325218,12.0790287957438));
#41717=CARTESIAN_POINT('Ctrl Pts',(-2.79052332865339,24.6922001294037,12.0826715709229));
#41718=CARTESIAN_POINT('Ctrl Pts',(-2.77021808960921,24.6908164562663,12.0857528770442));
#41719=CARTESIAN_POINT('Ctrl Pts',(-2.74984798236282,24.6894439939256,12.0888107047357));
#41720=CARTESIAN_POINT('Ctrl Pts',(-2.72941300692308,24.6880830383011,12.0918443696352));
#41721=CARTESIAN_POINT('Ctrl Pts',(-2.71919551920321,24.6874025604888,12.093361202085));
#41722=CARTESIAN_POINT('Ctrl Pts',(-2.70896181443498,24.6867249593443,12.0948719938314));
#41723=CARTESIAN_POINT('Ctrl Pts',(-2.69871189261957,24.6860502718866,12.0963766590913));
#41724=CARTESIAN_POINT('Ctrl Pts',(-2.68846197080415,24.6853755844289,12.0978813243511));
#41725=CARTESIAN_POINT('Ctrl Pts',(-2.67679403336437,24.6846126296739,12.0995833127281));
#41726=CARTESIAN_POINT('Ctrl Pts',(-2.66791347603294,24.6840349875721,12.1008721895521));
#41727=CARTESIAN_POINT('Ctrl Pts',(-2.4821521808828,24.6719520133897,12.1278325952085));
#41728=CARTESIAN_POINT('Ctrl Pts',(-2.29149550277842,24.6608332437257,12.1527602433646));
#41729=CARTESIAN_POINT('Ctrl Pts',(-2.09593759986156,24.650876181895,12.1751838538152));
#41730=CARTESIAN_POINT('Ctrl Pts',(-1.99233080678487,24.6456009195335,12.1870639074123));
#41731=CARTESIAN_POINT('Ctrl Pts',(-1.8873486430624,24.6406519782498,12.1982403723087));
#41732=CARTESIAN_POINT('Ctrl Pts',(-1.78099278865241,24.6360604107183,12.2086380279229));
#41733=CARTESIAN_POINT('Ctrl Pts',(-1.70012356698525,24.6325691455261,12.2165440366833));
#41734=CARTESIAN_POINT('Ctrl Pts',(-1.61846022911966,24.6292839247932,12.224000922958));
#41735=CARTESIAN_POINT('Ctrl Pts',(-1.53600131366634,24.6262173530196,12.2309772469221));
#41736=CARTESIAN_POINT('Ctrl Pts',(-1.46189047453595,24.623461238582,12.2372472932862));
#41737=CARTESIAN_POINT('Ctrl Pts',(-1.38713698026269,24.6208817564744,12.2431291335178));
#41738=CARTESIAN_POINT('Ctrl Pts',(-1.31174209049372,24.6184872332426,12.2485996392047));
#41739=CARTESIAN_POINT('Ctrl Pts',(-1.23210084282666,24.6159578467241,12.2543782523125));
#41740=CARTESIAN_POINT('Ctrl Pts',(-1.15174319434939,24.6136348616426,12.2596978632149));
#41741=CARTESIAN_POINT('Ctrl Pts',(-1.07066914350866,24.6115276457487,12.2645315222443));
#41742=CARTESIAN_POINT('Ctrl Pts',(-1.0301321180883,24.6104740378018,12.266948351759));
#41743=CARTESIAN_POINT('Ctrl Pts',(-0.989415992075765,24.6094743681992,
12.2692436913045));
#41744=CARTESIAN_POINT('Ctrl Pts',(-0.948520765373996,24.6085297687523,
12.2714141896979));
#41745=CARTESIAN_POINT('Ctrl Pts',(-0.928073152023112,24.6080574690288,
12.2724994388946));
#41746=CARTESIAN_POINT('Ctrl Pts',(-0.907580763500364,24.6075989365854,
12.2735534776725));
#41747=CARTESIAN_POINT('Ctrl Pts',(-0.887043599803289,24.6071543101594,
12.2745758886923));
#41748=CARTESIAN_POINT('Ctrl Pts',(-0.876775017954752,24.6069319969463,
12.2750870942022));
#41749=CARTESIAN_POINT('Ctrl Pts',(-0.866495242312671,24.6067131602211,
12.2755903927643));
#41750=CARTESIAN_POINT('Ctrl Pts',(-0.856204272877411,24.606497817139,12.2760857323367));
#41751=CARTESIAN_POINT('Ctrl Pts',(-0.845913303442152,24.6062824740569,
12.276581071909));
#41752=CARTESIAN_POINT('Ctrl Pts',(-0.833923452112789,24.6060365318656,
12.2771468969945));
#41753=CARTESIAN_POINT('Ctrl Pts',(-0.825297783192767,24.6058622858817,
12.2775478220662));
#41754=CARTESIAN_POINT('Ctrl Pts',(-0.603448600429803,24.6013807402201,
12.2878594744521));
#41755=CARTESIAN_POINT('Ctrl Pts',(-0.37948689987281,24.5986967762817,12.2941000099995));
#41756=CARTESIAN_POINT('Ctrl Pts',(-0.153407991024057,24.5978627736661,
12.2960214975774));
#41757=CARTESIAN_POINT('Ctrl Pts',(-0.0982029330636953,24.5976591228127,
12.2964906958483));
#41758=CARTESIAN_POINT('Ctrl Pts',(-0.0428716688643059,24.5975658351456,
12.2967021493351));
#41759=CARTESIAN_POINT('Ctrl Pts',(0.0125852473994843,24.5975839691981,
12.2966545842673));
#41760=CARTESIAN_POINT('Ctrl Pts',(0.153868872215892,24.5976301680285,12.296533406141));
#41761=CARTESIAN_POINT('Ctrl Pts',(0.295970723308233,24.5984017381627,12.2947266476478));
#41762=CARTESIAN_POINT('Ctrl Pts',(0.438890814847712,24.5999222771681,12.2912014538534));
#41763=CARTESIAN_POINT('Ctrl Pts',(0.510350860617452,24.6006825466707,12.2894388569562));
#41764=CARTESIAN_POINT('Ctrl Pts',(0.582015466023035,24.601630062137,12.2872466528321));
#41765=CARTESIAN_POINT('Ctrl Pts',(0.653884631028569,24.6027671760295,12.2846220155009));
#41766=CARTESIAN_POINT('Ctrl Pts',(0.689819213531337,24.6033357329758,12.2833096968352));
#41767=CARTESIAN_POINT('Ctrl Pts',(0.725804935920057,24.6039516899836,12.2818892701023));
#41768=CARTESIAN_POINT('Ctrl Pts',(0.761841798120305,24.6046153250416,12.2803604223681));
#41769=CARTESIAN_POINT('Ctrl Pts',(0.779860229220428,24.6049471425706,12.279595998501));
#41770=CARTESIAN_POINT('Ctrl Pts',(0.797891445272787,24.605290879649,12.2788044694029));
#41771=CARTESIAN_POINT('Ctrl Pts',(0.815935446265884,24.6056465689519,12.2779858007266));
#41772=CARTESIAN_POINT('Ctrl Pts',(0.83397944725898,24.6060022582549,12.2771671320502));
#41773=CARTESIAN_POINT('Ctrl Pts',(0.853658583894958,24.6064039841691,12.2762429440323));
#41774=CARTESIAN_POINT('Ctrl Pts',(0.87010580405451,24.6067495256734,12.2754483431328));
#41775=CARTESIAN_POINT('Ctrl Pts',(0.954941294067503,24.6085318440561,12.2713497565011));
#41776=CARTESIAN_POINT('Ctrl Pts',(1.03915646094878,24.6105620309033,12.2666905034544));
#41777=CARTESIAN_POINT('Ctrl Pts',(1.12274548009874,24.6128302696018,12.2614976172157));
#41778=CARTESIAN_POINT('Ctrl Pts',(1.34023153233054,24.6187318854487,12.2479865084693));
#41779=CARTESIAN_POINT('Ctrl Pts',(1.55347748717843,24.6262439843172,12.2308663947161));
#41780=CARTESIAN_POINT('Ctrl Pts',(1.762483134133,24.6351832068705,12.2106215991613));
#41781=CARTESIAN_POINT('Ctrl Pts',(1.93916409218177,24.6427398945867,12.1935078516322));
#41782=CARTESIAN_POINT('Ctrl Pts',(2.11281537507269,24.651316669607,12.1741602852205));
#41783=CARTESIAN_POINT('Ctrl Pts',(2.28344819732607,24.6608102578807,12.1528458878894));
#41784=CARTESIAN_POINT('Ctrl Pts',(2.31468206971439,24.6625480333024,12.1489443456335));
#41785=CARTESIAN_POINT('Ctrl Pts',(2.34581483060569,24.6643165454681,12.1449768417802));
#41786=CARTESIAN_POINT('Ctrl Pts',(2.37684657670109,24.6661151441892,12.14094498894));
#41787=CARTESIAN_POINT('Ctrl Pts',(2.47767146802531,24.6719589507231,12.1278451419897));
#41788=CARTESIAN_POINT('Ctrl Pts',(2.57829977290601,24.6781690799161,12.1139563702973));
#41789=CARTESIAN_POINT('Ctrl Pts',(2.67796169946932,24.6846878928205,12.0994139041198));
#41790=CARTESIAN_POINT('Ctrl Pts',(2.7797715261016,24.6913471982798,12.0845580207209));
#41791=CARTESIAN_POINT('Ctrl Pts',(2.88057272277316,24.6983286237912,12.0690200677786));
#41792=CARTESIAN_POINT('Ctrl Pts',(2.97955491921082,24.7055476241427,12.0529926455354));
#41793=CARTESIAN_POINT('Ctrl Pts',(3.01344853081799,24.7080195635714,12.0475045149005));
#41794=CARTESIAN_POINT('Ctrl Pts',(3.04712895742347,24.7105191649477,12.041959394733));
#41795=CARTESIAN_POINT('Ctrl Pts',(3.08056397514964,24.7130424427068,12.0363662321172));
#41796=CARTESIAN_POINT('Ctrl Pts',(3.15906127928106,24.7189664862736,12.023234844226));
#41797=CARTESIAN_POINT('Ctrl Pts',(3.23641909095361,24.7250360856396,12.0098052009448));
#41798=CARTESIAN_POINT('Ctrl Pts',(3.31263593447761,24.7312319284034,11.9961212804716));
#41799=CARTESIAN_POINT('Ctrl Pts',(3.45649514762954,24.742926575198,11.9702928947618));
#41800=CARTESIAN_POINT('Ctrl Pts',(3.59628911990336,24.7550705254824,11.9435601098344));
#41801=CARTESIAN_POINT('Ctrl Pts',(3.73202210256371,24.7675395543834,11.9162079919652));
#41802=CARTESIAN_POINT('Ctrl Pts',(3.83584437063496,24.7770771246613,11.8952863349142));
#41803=CARTESIAN_POINT('Ctrl Pts',(3.93728959584421,24.7868049511524,11.8740020174483));
#41804=CARTESIAN_POINT('Ctrl Pts',(4.03635777754101,24.7966696197805,11.8524749977332));
#41805=CARTESIAN_POINT('Ctrl Pts',(4.06112482296521,24.7991357869376,11.8470932428044));
#41806=CARTESIAN_POINT('Ctrl Pts',(4.08675526253289,24.8017100309838,11.8414789509819));
#41807=CARTESIAN_POINT('Ctrl Pts',(4.11470923698786,24.8045497714992,11.8352904735459));
#41808=CARTESIAN_POINT('Ctrl Pts',(4.14266321144283,24.8073895120145,11.82910199611));
#41809=CARTESIAN_POINT('Ctrl Pts',(4.17043865119258,24.8102415991542,11.8228911837828));
#41810=CARTESIAN_POINT('Ctrl Pts',(4.19803555625679,24.8131048456758,11.8166606647739));
#41811=CARTESIAN_POINT('Ctrl Pts',(4.20574811713802,24.8139050427654,11.8149194094749));
#41812=CARTESIAN_POINT('Ctrl Pts',(4.21344673423827,24.8147061117068,11.8131766143782));
#41813=CARTESIAN_POINT('Ctrl Pts',(4.22113140699254,24.8155080272097,11.8114323353406));
#41814=CARTESIAN_POINT('Ctrl Pts',(4.26844096707861,24.820444902322,11.8006939374182));
#41815=CARTESIAN_POINT('Ctrl Pts',(4.31522201697745,24.8254138542797,11.7898993285224));
#41816=CARTESIAN_POINT('Ctrl Pts',(4.36147457069009,24.8304091817874,11.7790615486346));
#41817=CARTESIAN_POINT('Ctrl Pts',(4.51942902572204,24.8474684395116,11.7420500654077));
#41818=CARTESIAN_POINT('Ctrl Pts',(4.67122070919016,24.8648335220303,11.7045405147502));
#41819=CARTESIAN_POINT('Ctrl Pts',(4.81684736731411,24.8822895362551,11.6670123777528));
#41820=CARTESIAN_POINT('Ctrl Pts',(4.86949798788909,24.8886006745696,11.6534442596116));
#41821=CARTESIAN_POINT('Ctrl Pts',(4.92134287229698,24.8949238271383,11.639873245553));
#41822=CARTESIAN_POINT('Ctrl Pts',(4.97238230295595,24.9012492749469,11.6263204404126));
#41823=CARTESIAN_POINT('Ctrl Pts',(5.00462682834192,24.9052454218437,11.6177583588266));
#41824=CARTESIAN_POINT('Ctrl Pts',(5.03654983709019,24.9092421091841,11.609204372807));
#41825=CARTESIAN_POINT('Ctrl Pts',(5.06815129371138,24.9132371956239,11.600663060826));
#41826=CARTESIAN_POINT('Ctrl Pts',(5.21039120872686,24.931219302034,11.5622181402369));
#41827=CARTESIAN_POINT('Ctrl Pts',(5.34611635892373,24.9491683164726,11.5240340989402));
#41828=CARTESIAN_POINT('Ctrl Pts',(5.47532628982706,24.9669060425853,11.4865024016981));
#41829=CARTESIAN_POINT('Ctrl Pts',(5.60705266944068,24.9849892226247,11.4482397498733));
#41830=CARTESIAN_POINT('Ctrl Pts',(5.73200777566556,25.0028526551875,11.4106549774584));
#41831=CARTESIAN_POINT('Ctrl Pts',(5.85019315529358,25.0203177622383,11.3741100912551));
#41832=CARTESIAN_POINT('Ctrl Pts',(5.86232961592042,25.0221112546714,11.3703572956562));
#41833=CARTESIAN_POINT('Ctrl Pts',(5.87439468833947,25.0239005565685,11.3666154218325));
#41834=CARTESIAN_POINT('Ctrl Pts',(5.88638837412032,25.025685481493,11.3628848318741));
#41835=CARTESIAN_POINT('Ctrl Pts',(5.92102986643391,25.0308408994504,11.3521097285629));
#41836=CARTESIAN_POINT('Ctrl Pts',(5.95507582044337,25.0359598050818,11.3414287803088));
#41837=CARTESIAN_POINT('Ctrl Pts',(5.98852582161158,25.0410382878129,11.330850113083));
#41838=CARTESIAN_POINT('',(-6.27159361731522,24.2690120888703,11.879497561603));
#41839=CARTESIAN_POINT('Origin',(-5.999994980806,24.1259380084193,10.9277770011849));
#41840=CARTESIAN_POINT('Ctrl Pts',(-6.27159386307668,24.269012372504,11.8794985003143));
#41841=CARTESIAN_POINT('Ctrl Pts',(-6.19708064355491,24.257447552827,11.9025009420341));
#41842=CARTESIAN_POINT('Ctrl Pts',(-6.11543893234907,24.2450493535732,11.9272858599129));
#41843=CARTESIAN_POINT('Ctrl Pts',(-6.02658469700067,24.2319368708288,11.9536191464949));
#41844=CARTESIAN_POINT('Ctrl Pts',(-5.93855993474233,24.2189467958857,11.9797066062742));
#41845=CARTESIAN_POINT('Ctrl Pts',(-5.84345652710574,24.2052557303348,12.0073137939348));
#41846=CARTESIAN_POINT('Ctrl Pts',(-5.74118379376358,24.1909996650877,12.0361672876422));
#41847=CARTESIAN_POINT('Ctrl Pts',(-5.64049529917842,24.176964431047,12.0645738311068));
#41848=CARTESIAN_POINT('Ctrl Pts',(-5.53285770076121,24.1623816026613,12.0941884706608));
#41849=CARTESIAN_POINT('Ctrl Pts',(-5.41817811424983,24.1474001738651,12.1247040182081));
#41850=CARTESIAN_POINT('Ctrl Pts',(-5.37925230863917,24.1423150126535,12.13506194073));
#41851=CARTESIAN_POINT('Ctrl Pts',(-5.33951512841442,24.1371840902973,12.1455232546647));
#41852=CARTESIAN_POINT('Ctrl Pts',(-5.29896282541134,24.1320137374897,12.1560746713286));
#41853=CARTESIAN_POINT('Ctrl Pts',(-5.21821392328632,24.1217183835418,12.1770849530728));
#41854=CARTESIAN_POINT('Ctrl Pts',(-5.13423307029617,24.1112663286752,12.1984531632364));
#41855=CARTESIAN_POINT('Ctrl Pts',(-5.04699092036662,24.100713815105,12.2200666333059));
#41856=CARTESIAN_POINT('Ctrl Pts',(-4.92201158417912,24.0855967399048,12.2510291570879));
#41857=CARTESIAN_POINT('Ctrl Pts',(-4.79033922609239,24.0702724377968,12.2824971537965));
#41858=CARTESIAN_POINT('Ctrl Pts',(-4.65188793009117,24.0549260394076,12.3140996072383));
#41859=CARTESIAN_POINT('Ctrl Pts',(-4.51343663408995,24.0395796410183,12.3457020606801));
#41860=CARTESIAN_POINT('Ctrl Pts',(-4.36820620262285,24.0242110240233,12.3774392325216));
#41861=CARTESIAN_POINT('Ctrl Pts',(-4.21611372758432,24.0090302236472,12.4088898513687));
#41862=CARTESIAN_POINT('Ctrl Pts',(-4.07083064523525,23.9945290889224,12.438932382051));
#41863=CARTESIAN_POINT('Ctrl Pts',(-3.9192856554265,23.9801993615862,12.4687131290188));
#41864=CARTESIAN_POINT('Ctrl Pts',(-3.7614235687259,23.9662478755224,12.4978242922883));
#41865=CARTESIAN_POINT('Ctrl Pts',(-3.73054864789812,23.963519221438,12.503517900424));
#41866=CARTESIAN_POINT('Ctrl Pts',(-3.69943212037155,23.9608051084921,12.5091857580551));
#41867=CARTESIAN_POINT('Ctrl Pts',(-3.66807362860842,23.9581071913898,12.514824611152));
#41868=CARTESIAN_POINT('Ctrl Pts',(-3.58017498071281,23.9505448613129,12.5306304594259));
#41869=CARTESIAN_POINT('Ctrl Pts',(-3.49037513304142,23.9431096153184,12.5462087339496));
#41870=CARTESIAN_POINT('Ctrl Pts',(-3.39866711183985,23.9358394491402,12.5614848729961));
#41871=CARTESIAN_POINT('Ctrl Pts',(-3.35281310123906,23.9322043660511,12.5691229425193));
#41872=CARTESIAN_POINT('Ctrl Pts',(-3.30648203830319,23.9286105462567,12.5766854205411));
#41873=CARTESIAN_POINT('Ctrl Pts',(-3.25967322154924,23.92506300707,12.5841625650012));
#41874=CARTESIAN_POINT('Ctrl Pts',(-3.23626881317227,23.9232892374766,12.5879011372313));
#41875=CARTESIAN_POINT('Ctrl Pts',(-3.21274496574493,23.9215270376051,12.591618372388));
#41876=CARTESIAN_POINT('Ctrl Pts',(-3.18910159554922,23.9197770412036,12.5953130281382));
#41877=CARTESIAN_POINT('Ctrl Pts',(-3.17727991045136,23.9189020430028,12.5971603560134));
#41878=CARTESIAN_POINT('Ctrl Pts',(-3.16542834462672,23.9180300956426,12.5990020388008));
#41879=CARTESIAN_POINT('Ctrl Pts',(-3.15354688824311,23.9171612793004,12.6008379195334));
#41880=CARTESIAN_POINT('Ctrl Pts',(-3.14166543185951,23.9162924629581,12.6026738002661));
#41881=CARTESIAN_POINT('Ctrl Pts',(-3.12814004122944,23.9153102008938,12.6047504367141));
#41882=CARTESIAN_POINT('Ctrl Pts',(-3.11781283770736,23.9145643037385,12.6063279975685));
#41883=CARTESIAN_POINT('Ctrl Pts',(-3.07662183306194,23.9115892240741,12.6126202446754));
#41884=CARTESIAN_POINT('Ctrl Pts',(-3.03569007115575,23.9086934856334,12.6187479999135));
#41885=CARTESIAN_POINT('Ctrl Pts',(-2.99501928702404,23.9058749439134,12.6247156162381));
#41886=CARTESIAN_POINT('Ctrl Pts',(-2.79740326461739,23.8921798796164,12.6537117771556));
#41887=CARTESIAN_POINT('Ctrl Pts',(-2.60595262443292,23.8803068051101,12.6789288382829));
#41888=CARTESIAN_POINT('Ctrl Pts',(-2.42086041740396,23.8700053894468,12.7008770362872));
#41889=CARTESIAN_POINT('Ctrl Pts',(-2.23093226975246,23.8594348266634,12.7233986791924));
#41890=CARTESIAN_POINT('Ctrl Pts',(-2.04769883486201,23.8505189268116,12.7424787292335));
#41891=CARTESIAN_POINT('Ctrl Pts',(-1.87131988108705,23.8429960706186,12.7586446085497));
#41892=CARTESIAN_POINT('Ctrl Pts',(-1.78117209842544,23.8391511175186,12.7669070352391));
#41893=CARTESIAN_POINT('Ctrl Pts',(-1.69281414034322,23.8356702230497,12.7744077954315));
#41894=CARTESIAN_POINT('Ctrl Pts',(-1.60626302545199,23.8325195648083,12.7812145895975));
#41895=CARTESIAN_POINT('Ctrl Pts',(-1.43906926035782,23.8264333299335,12.794363507971));
#41896=CARTESIAN_POINT('Ctrl Pts',(-1.27862001152862,23.8215783542681,12.8049253098459));
#41897=CARTESIAN_POINT('Ctrl Pts',(-1.12501483737541,23.8177149735438,12.8133805318948));
#41898=CARTESIAN_POINT('Ctrl Pts',(-0.969937943776955,23.8138145770577,
12.8219167649825));
#41899=CARTESIAN_POINT('Ctrl Pts',(-0.821836508844503,23.8109247554415,
12.82830598725));
#41900=CARTESIAN_POINT('Ctrl Pts',(-0.68078060386382,23.8088158620706,12.8330037588192));
#41901=CARTESIAN_POINT('Ctrl Pts',(-0.538386326148549,23.8066869590064,
12.8377461039877));
#41902=CARTESIAN_POINT('Ctrl Pts',(-0.403171528273148,23.8053537628513,
12.8407648857556));
#41903=CARTESIAN_POINT('Ctrl Pts',(-0.275181359097709,23.804598937094,12.8424872539434));
#41904=CARTESIAN_POINT('Ctrl Pts',(-0.236216706984929,23.8043691419212,
12.8430116026312));
#41905=CARTESIAN_POINT('Ctrl Pts',(-0.197921471761721,23.8041930881746,
12.8434155026696));
#41906=CARTESIAN_POINT('Ctrl Pts',(-0.160296520170288,23.8040650105823,
12.8437102229334));
#41907=CARTESIAN_POINT('Ctrl Pts',(-0.153989049541499,23.8040435395739,
12.8437596300244));
#41908=CARTESIAN_POINT('Ctrl Pts',(-0.147700415760366,23.8040234172524,
12.8438059679572));
#41909=CARTESIAN_POINT('Ctrl Pts',(-0.141430622130303,23.8040046157402,
12.8438492897956));
#41910=CARTESIAN_POINT('Ctrl Pts',(-0.103047756612804,23.8038895153152,
12.8441145004857));
#41911=CARTESIAN_POINT('Ctrl Pts',(-0.0662555271181962,23.8038251183766,
12.8442644027209));
#41912=CARTESIAN_POINT('Ctrl Pts',(-0.0289807949193498,23.803801947349,
12.8443170163513));
#41913=CARTESIAN_POINT('Ctrl Pts',(-0.0185588386823882,23.8037954687663,
12.8443317270392));
#41914=CARTESIAN_POINT('Ctrl Pts',(-0.00809916138173642,23.8037923566792,
12.8443385556309));
#41915=CARTESIAN_POINT('Ctrl Pts',(0.00244355159875256,23.8037927379189,
12.8443372526226));
#41916=CARTESIAN_POINT('Ctrl Pts',(0.127127933612357,23.8037972466852,12.8443218424727));
#41917=CARTESIAN_POINT('Ctrl Pts',(0.258986326506927,23.8042924730393,12.8431696778079));
#41918=CARTESIAN_POINT('Ctrl Pts',(0.397985511715484,23.8054910530804,12.8404650188549));
#41919=CARTESIAN_POINT('Ctrl Pts',(0.535666539858683,23.8066782667474,12.8377860087235));
#41920=CARTESIAN_POINT('Ctrl Pts',(0.680353891965151,23.8085556400841,12.8335836971678));
#41921=CARTESIAN_POINT('Ctrl Pts',(0.831993331814887,23.8113495659765,12.8274126597883));
#41922=CARTESIAN_POINT('Ctrl Pts',(0.942271900153292,23.8133814262087,12.8229248222703));
#41923=CARTESIAN_POINT('Ctrl Pts',(1.05622686550899,23.815898445416,12.8173949054093));
#41924=CARTESIAN_POINT('Ctrl Pts',(1.17382842541542,23.8189939856533,12.8106381116661));
#41925=CARTESIAN_POINT('Ctrl Pts',(1.33438952036287,23.8232203184531,12.8014130792551));
#41926=CARTESIAN_POINT('Ctrl Pts',(1.5017497937385,23.8285247626977,12.7899019055094));
#41927=CARTESIAN_POINT('Ctrl Pts',(1.67579823257016,23.8351501275165,12.7756189141176));
#41928=CARTESIAN_POINT('Ctrl Pts',(1.84379921228085,23.8415452884728,12.7618321972523));
#41929=CARTESIAN_POINT('Ctrl Pts',(2.01803188912892,23.8491713462831,12.7454626456316));
#41930=CARTESIAN_POINT('Ctrl Pts',(2.19835974409792,23.8582571099095,12.7260476068924));
#41931=CARTESIAN_POINT('Ctrl Pts',(2.26108749646338,23.8614176284601,12.7192940094384));
#41932=CARTESIAN_POINT('Ctrl Pts',(2.32455242973094,23.8647548580991,12.7121716847517));
#41933=CARTESIAN_POINT('Ctrl Pts',(2.38874762162472,23.8682786803638,12.7046604832679));
#41934=CARTESIAN_POINT('Ctrl Pts',(2.47500692939018,23.8730136528792,12.694567655108));
#41935=CARTESIAN_POINT('Ctrl Pts',(2.56258480368602,23.8780855236188,12.6837727027421));
#41936=CARTESIAN_POINT('Ctrl Pts',(2.65146457977943,23.8835179280606,12.6722277590264));
#41937=CARTESIAN_POINT('Ctrl Pts',(2.72897715545603,23.8882555599372,12.6621593456845));
#41938=CARTESIAN_POINT('Ctrl Pts',(2.80747992660754,23.893267461597,12.6515204889937));
#41939=CARTESIAN_POINT('Ctrl Pts',(2.88696060483214,23.8985693823657,12.6402790380552));
#41940=CARTESIAN_POINT('Ctrl Pts',(2.92670094394444,23.90122034275,12.6346583125859));
#41941=CARTESIAN_POINT('Ctrl Pts',(2.96668575863641,23.9039438070294,12.6288869308983));
#41942=CARTESIAN_POINT('Ctrl Pts',(3.00691339184227,23.9067417699088,12.622960840973));
#41943=CARTESIAN_POINT('Ctrl Pts',(3.02702720844519,23.9081407513484,12.6199977960103));
#41944=CARTESIAN_POINT('Ctrl Pts',(3.04720172962192,23.9095583573876,12.616996073527));
#41945=CARTESIAN_POINT('Ctrl Pts',(3.06743674365025,23.9109948367397,12.6139551648845));
#41946=CARTESIAN_POINT('Ctrl Pts',(3.07755425066441,23.9117130764157,12.6124347105632));
#41947=CARTESIAN_POINT('Ctrl Pts',(3.08768688088734,23.9124360344167,12.6109044596733));
#41948=CARTESIAN_POINT('Ctrl Pts',(3.09783460737601,23.9131637418684,12.609364348521));
#41949=CARTESIAN_POINT('Ctrl Pts',(3.10798233386467,23.9138914493201,12.6078242373688));
#41950=CARTESIAN_POINT('Ctrl Pts',(3.11649242505667,23.9145041902963,12.6065275687504));
#41951=CARTESIAN_POINT('Ctrl Pts',(3.1283230485401,23.9153611437042,12.6047143704876));
#41952=CARTESIAN_POINT('Ctrl Pts',(3.24396953136792,23.9237380181527,12.5869900297497));
#41953=CARTESIAN_POINT('Ctrl Pts',(3.3568243586389,23.9324158983593,12.5687080553323));
#41954=CARTESIAN_POINT('Ctrl Pts',(3.46689563032691,23.9413247217354,12.5500051077454));
#41955=CARTESIAN_POINT('Ctrl Pts',(3.63913334366982,23.9552651018488,12.5207390433515));
#41956=CARTESIAN_POINT('Ctrl Pts',(3.80455492701866,23.9697695395805,12.490444984664));
#41957=CARTESIAN_POINT('Ctrl Pts',(3.96321661984212,23.9845904106421,12.4596112646828));
#41958=CARTESIAN_POINT('Ctrl Pts',(4.12187831266557,23.9994112817037,12.4287775447016));
#41959=CARTESIAN_POINT('Ctrl Pts',(4.27378038616038,24.0145487274433,12.3974038969458));
#41960=CARTESIAN_POINT('Ctrl Pts',(4.41899134479992,24.0297826839403,12.3659258747014));
#41961=CARTESIAN_POINT('Ctrl Pts',(4.56352096943963,24.0449451622747,12.3345955482439));
#41962=CARTESIAN_POINT('Ctrl Pts',(4.70142263439583,24.0602034826833,12.3031616819607));
#41963=CARTESIAN_POINT('Ctrl Pts',(4.83277716212323,24.0753674355567,12.2720080573813));
#41964=CARTESIAN_POINT('Ctrl Pts',(4.9053251093476,24.0837425838808,12.2548017109314));
#41965=CARTESIAN_POINT('Ctrl Pts',(4.9758759694648,24.0920893585459,12.237679993631));
#41966=CARTESIAN_POINT('Ctrl Pts',(5.04444366271275,24.1003786573682,12.2207014769521));
#41967=CARTESIAN_POINT('Ctrl Pts',(5.13538874063298,24.1113732073027,12.1981819426176));
#41968=CARTESIAN_POINT('Ctrl Pts',(5.22284501885468,24.1222664368161,12.175914753616));
#41969=CARTESIAN_POINT('Ctrl Pts',(5.3068450680899,24.1329958452549,12.1540254663863));
#41970=CARTESIAN_POINT('Ctrl Pts',(5.42689981753904,24.1483305558126,12.1227408074139));
#41971=CARTESIAN_POINT('Ctrl Pts',(5.5398950609485,24.1633299521138,12.0922300430563));
#41972=CARTESIAN_POINT('Ctrl Pts',(5.6459278454596,24.1778363423683,12.062817169183));
#41973=CARTESIAN_POINT('Ctrl Pts',(5.75378710239914,24.1925926130909,12.0328976425474));
#41974=CARTESIAN_POINT('Ctrl Pts',(5.85444212010429,24.2068387252984,12.0041140585228));
#41975=CARTESIAN_POINT('Ctrl Pts',(5.94798769898028,24.2204300315958,11.9767579553003));
#41976=CARTESIAN_POINT('Ctrl Pts',(6.02496474147653,24.2316140829963,11.9542470900558));
#41977=CARTESIAN_POINT('Ctrl Pts',(6.0971276192275,24.242355142051,11.932701864461));
#41978=CARTESIAN_POINT('Ctrl Pts',(6.16452450090078,24.2525832703824,11.9122610048017));
#41979=CARTESIAN_POINT('Ctrl Pts',(6.20165912102731,24.2582188079735,11.900998413126));
#41980=CARTESIAN_POINT('Ctrl Pts',(6.23734677868856,24.2636988328348,11.8900707158152));
#41981=CARTESIAN_POINT('Ctrl Pts',(6.27159479316366,24.2690136880232,11.8794983798008));
#41982=CARTESIAN_POINT('Ctrl Pts',(-6.390311350216,24.5118553841645,11.8061920238492));
#41983=CARTESIAN_POINT('Ctrl Pts',(-4.260207566811,24.1870632643171,12.4817966807133));
#41984=CARTESIAN_POINT('Ctrl Pts',(0.0001663376446825,23.8622675910407,
13.1582619392195));
#41985=CARTESIAN_POINT('Ctrl Pts',(4.2605402421,24.1870886272834,12.4817438562278));
#41986=CARTESIAN_POINT('Ctrl Pts',(6.39081036315,24.511931475205,11.806033745832));
#41987=CARTESIAN_POINT('Ctrl Pts',(-6.390311350216,23.5459013914926,11.972049816479));
#41988=CARTESIAN_POINT('Ctrl Pts',(-4.260207566811,23.2652611637952,12.607762371841));
#41989=CARTESIAN_POINT('Ctrl Pts',(0.0001663376446825,22.9846427151217,
13.246147024971));
#41990=CARTESIAN_POINT('Ctrl Pts',(4.2605402421,23.2652830770076,12.6077125210326));
#41991=CARTESIAN_POINT('Ctrl Pts',(6.39081036315,23.5459671387971,11.9719008842438));
#41992=CARTESIAN_POINT('Ctrl Pts',(-6.390311350216,21.4528944638882,12.0713624052953));
#41993=CARTESIAN_POINT('Ctrl Pts',(-4.260207566811,21.2792418481892,12.6592431178696));
#41994=CARTESIAN_POINT('Ctrl Pts',(0.0001663376446825,21.1056362242977,
13.2456913466391));
#41995=CARTESIAN_POINT('Ctrl Pts',(4.2605402421,21.2792554048749,12.6591973227215));
#41996=CARTESIAN_POINT('Ctrl Pts',(6.39081036315,21.452935146549,12.0712246788794));
#41997=CARTESIAN_POINT('Ctrl Pts',(-6.390311350216,18.3168609136256,11.387980855255));
#41998=CARTESIAN_POINT('Ctrl Pts',(-4.260207566811,18.3050659001773,12.0191856806278));
#41999=CARTESIAN_POINT('Ctrl Pts',(0.0001663376446825,18.2929947474349,
12.6510858022935));
#42000=CARTESIAN_POINT('Ctrl Pts',(4.2605402421,18.3050668428002,12.019136336187));
#42001=CARTESIAN_POINT('Ctrl Pts',(6.39081036315,18.3168636769111,11.3878329790519));
#42002=CARTESIAN_POINT('Ctrl Pts',(-6.390311350216,15.6639828127201,9.9696585797627));
#42003=CARTESIAN_POINT('Ctrl Pts',(-4.260207566811,15.7525582543281,10.7489240488924));
#42004=CARTESIAN_POINT('Ctrl Pts',(0.0001663376446825,15.8420472730181,
11.5272475946804));
#42005=CARTESIAN_POINT('Ctrl Pts',(4.2605402421,15.7525512662236,10.748863270397));
#42006=CARTESIAN_POINT('Ctrl Pts',(6.39081036315,15.6639620616126,9.96947601647265));
#42007=CARTESIAN_POINT('Ctrl Pts',(-6.390311350216,14.2540946963906,8.71288811092588));
#42008=CARTESIAN_POINT('Ctrl Pts',(-4.260207566811,14.3565358989963,9.62694787697193));
#42009=CARTESIAN_POINT('Ctrl Pts',(0.0001663376446825,14.4576055194805,
10.542393035863));
#42010=CARTESIAN_POINT('Ctrl Pts',(4.2605402421,14.3565280065696,9.62687639078721));
#42011=CARTESIAN_POINT('Ctrl Pts',(6.39081036315,14.2540706968538,8.71267396857703));
#42012=CARTESIAN_POINT('Ctrl Pts',(-6.390311350216,13.724648700715,8.13903540228875));
#42013=CARTESIAN_POINT('Ctrl Pts',(-4.260207566811,13.8218533779545,9.11395898716084));
#42014=CARTESIAN_POINT('Ctrl Pts',(0.0001663376446825,13.9179753162775,
10.089995002773));
#42015=CARTESIAN_POINT('Ctrl Pts',(4.2605402421,13.8218458718956,9.11388276950054));
#42016=CARTESIAN_POINT('Ctrl Pts',(6.39081036315,13.7246259279729,8.13880700099865));
#42017=CARTESIAN_POINT('',(-6.26386060039021,13.9442583526775,8.42071136781886));
#42018=CARTESIAN_POINT('Ctrl Pts',(-6.27159552384944,24.2690121660566,11.8794980574134));
#42019=CARTESIAN_POINT('Ctrl Pts',(-6.27195777359875,24.0278185402074,11.915653438685));
#42020=CARTESIAN_POINT('Ctrl Pts',(-6.27229031327705,23.7878332541021,11.9441024445887));
#42021=CARTESIAN_POINT('Ctrl Pts',(-6.27259314313041,23.5495553889474,11.9652318805794));
#42022=CARTESIAN_POINT('Ctrl Pts',(-6.27289863582021,23.3091823043902,11.9865471114371));
#42023=CARTESIAN_POINT('Ctrl Pts',(-6.27317389390043,23.0705467110858,12.0004135052685));
#42024=CARTESIAN_POINT('Ctrl Pts',(-6.27341891762367,22.8341074530425,12.0072245125909));
#42025=CARTESIAN_POINT('Ctrl Pts',(-6.2736675427923,22.5941929271239,12.014135630509));
#42026=CARTESIAN_POINT('Ctrl Pts',(-6.27388503828152,22.3565397309245,12.0137824613571));
#42027=CARTESIAN_POINT('Ctrl Pts',(-6.27407140435525,22.1215733217137,12.0065719180718));
#42028=CARTESIAN_POINT('Ctrl Pts',(-6.27421804489091,21.9366920318044,12.0008983643582));
#42029=CARTESIAN_POINT('Ctrl Pts',(-6.27434541260364,21.7534730872847,11.9909791988217));
#42030=CARTESIAN_POINT('Ctrl Pts',(-6.27445350762203,21.5721011929276,11.9770107164691));
#42031=CARTESIAN_POINT('Ctrl Pts',(-6.2745026299563,21.4896791631684,11.9706629266297));
#42032=CARTESIAN_POINT('Ctrl Pts',(-6.27454777223563,21.4076383057737,11.963478898258));
#42033=CARTESIAN_POINT('Ctrl Pts',(-6.27458893447209,21.3259943042553,11.9554821771386));
#42034=CARTESIAN_POINT('Ctrl Pts',(-6.27470712627363,21.0915645829234,11.9325206726958));
#42035=CARTESIAN_POINT('Ctrl Pts',(-6.27479250328971,20.8604106337727,11.9028603060025));
#42036=CARTESIAN_POINT('Ctrl Pts',(-6.27484506552035,20.6328684194097,11.8670439018405));
#42037=CARTESIAN_POINT('Ctrl Pts',(-6.27489762775099,20.4053262050468,11.8312274976785));
#42038=CARTESIAN_POINT('Ctrl Pts',(-6.27491737519619,20.1813955353361,11.7892550171273));
#42039=CARTESIAN_POINT('Ctrl Pts',(-6.27490430785594,19.9613622611599,11.7416481083875));
#42040=CARTESIAN_POINT('Ctrl Pts',(-6.27489476770969,19.800721336778,11.7068914659862));
#42041=CARTESIAN_POINT('Ctrl Pts',(-6.27486753862054,19.6418692732658,11.669064473988));
#42042=CARTESIAN_POINT('Ctrl Pts',(-6.27482283777318,19.485219732692,11.6284222396903));
#42043=CARTESIAN_POINT('Ctrl Pts',(-6.27477792003791,19.32781013067,11.5875828098224));
#42044=CARTESIAN_POINT('Ctrl Pts',(-6.27471536058765,19.1726247739736,11.5439009383169));
#42045=CARTESIAN_POINT('Ctrl Pts',(-6.27463537978378,19.0200566298959,11.4976809493562));
#42046=CARTESIAN_POINT('Ctrl Pts',(-6.2745769103504,18.9085227054517,11.4638921346092));
#42047=CARTESIAN_POINT('Ctrl Pts',(-6.27450913052138,18.7983869345835,11.4287478520123));
#42048=CARTESIAN_POINT('Ctrl Pts',(-6.27443212638912,18.6897925869713,11.3923813180313));
#42049=CARTESIAN_POINT('Ctrl Pts',(-6.274356354692,18.5829362693268,11.3565968228697));
#42050=CARTESIAN_POINT('Ctrl Pts',(-6.27427024754847,18.4758583327785,11.3190562070229));
#42051=CARTESIAN_POINT('Ctrl Pts',(-6.27417380495852,18.3686262100774,11.2797074661865));
#42052=CARTESIAN_POINT('Ctrl Pts',(-6.27399075528872,18.1650978243038,11.2050228893736));
#42053=CARTESIAN_POINT('Ctrl Pts',(-6.27377047250067,17.9610111107778,11.1238234851248));
#42054=CARTESIAN_POINT('Ctrl Pts',(-6.27351295659435,17.7568354136725,11.0358411780908));
#42055=CARTESIAN_POINT('Ctrl Pts',(-6.27325823283633,17.5548735169924,10.9488128301787));
#42056=CARTESIAN_POINT('Ctrl Pts',(-6.27296707899227,17.3528244668957,10.8551477982201));
#42057=CARTESIAN_POINT('Ctrl Pts',(-6.27263949506218,17.1511911386934,10.7546004677717));
#42058=CARTESIAN_POINT('Ctrl Pts',(-6.27231699830121,16.9526890472353,10.6556145731159));
#42059=CARTESIAN_POINT('Ctrl Pts',(-6.27195919414059,16.7545898242303,10.5499584205239));
#42060=CARTESIAN_POINT('Ctrl Pts',(-6.27156608258035,16.5574215753287,10.4374120685186));
#42061=CARTESIAN_POINT('Ctrl Pts',(-6.27136275125215,16.4554391205203,10.3791990787438));
#42062=CARTESIAN_POINT('Ctrl Pts',(-6.271149974038,16.3537065297169,10.3191429768495));
#42063=CARTESIAN_POINT('Ctrl Pts',(-6.27092775093789,16.2523021361105,10.2572149522302));
#42064=CARTESIAN_POINT('Ctrl Pts',(-6.27050608269128,16.0598873384097,10.1397065494349));
#42065=CARTESIAN_POINT('Ctrl Pts',(-6.27005040505914,15.8686512520362,10.0154573241263));
#42066=CARTESIAN_POINT('Ctrl Pts',(-6.26956071763076,15.6791659370351,9.88428219016649));
#42067=CARTESIAN_POINT('Ctrl Pts',(-6.2693850513209,15.6111915841536,9.8372255364886));
#42068=CARTESIAN_POINT('Ctrl Pts',(-6.26920500834835,15.5434429948885,9.78927774773558));
#42069=CARTESIAN_POINT('Ctrl Pts',(-6.26902058869414,15.4759481427354,9.74043078888112));
#42070=CARTESIAN_POINT('Ctrl Pts',(-6.26850854120704,15.2885463737326,9.60480553439552));
#42071=CARTESIAN_POINT('Ctrl Pts',(-6.26796275325752,15.1030977555619,9.46224615032455));
#42072=CARTESIAN_POINT('Ctrl Pts',(-6.26738322443976,14.9201595432571,9.31269267423412));
#42073=CARTESIAN_POINT('Ctrl Pts',(-6.26681231188111,14.7399412009397,9.16536271397456));
#42074=CARTESIAN_POINT('Ctrl Pts',(-6.26620865429388,14.5621591566521,9.01124503746522));
#42075=CARTESIAN_POINT('Ctrl Pts',(-6.26557225129009,14.3873869151172,8.85031163435012));
#42076=CARTESIAN_POINT('Ctrl Pts',(-6.2650258403793,14.2373287615404,8.71213540505762));
#42077=CARTESIAN_POINT('Ctrl Pts',(-6.26445529016119,14.0894899890531,8.56893517534428));
#42078=CARTESIAN_POINT('Ctrl Pts',(-6.26386060039021,13.9442583526775,8.42071136781886));
#42079=CARTESIAN_POINT('Ctrl Pts',(6.26385989006508,13.9442649556658,8.42071839528551));
#42080=CARTESIAN_POINT('Ctrl Pts',(5.97553496877593,13.9555618354838,8.54505430197946));
#42081=CARTESIAN_POINT('Ctrl Pts',(5.6853707846613,13.9652272416059,8.6607532436919));
#42082=CARTESIAN_POINT('Ctrl Pts',(5.39385482794471,13.9735175248353,8.76768516072829));
#42083=CARTESIAN_POINT('Ctrl Pts',(5.12004274101568,13.9813043361571,8.86812306365763));
#42084=CARTESIAN_POINT('Ctrl Pts',(4.84503808318898,13.9878781560399,8.96082580983451));
#42085=CARTESIAN_POINT('Ctrl Pts',(4.5692448129743,13.9934626776619,9.04572743851788));
#42086=CARTESIAN_POINT('Ctrl Pts',(4.3128000449903,13.9986554126063,9.12467272406537));
#42087=CARTESIAN_POINT('Ctrl Pts',(4.05567343468833,14.0029929135767,9.1968728374423));
#42088=CARTESIAN_POINT('Ctrl Pts',(3.79818974563082,14.0066630216774,9.26231788137843));
#42089=CARTESIAN_POINT('Ctrl Pts',(3.57801043857143,14.0098014024479,9.31828121046181));
#42090=CARTESIAN_POINT('Ctrl Pts',(3.35757002508127,14.0124518967487,9.36930547712606));
#42091=CARTESIAN_POINT('Ctrl Pts',(3.13707157603067,14.0147362856601,9.41541459537568));
#42092=CARTESIAN_POINT('Ctrl Pts',(2.89171879902103,14.0172781682249,9.46672107964674));
#42093=CARTESIAN_POINT('Ctrl Pts',(2.64632878443407,14.019382025325,9.51194774108423));
#42094=CARTESIAN_POINT('Ctrl Pts',(2.40114096253886,14.0211091486273,9.551085447327));
#42095=CARTESIAN_POINT('Ctrl Pts',(2.15971436100687,14.0228097775822,9.58962277490271));
#42096=CARTESIAN_POINT('Ctrl Pts',(1.91848379641032,14.0241451642015,9.62225648551632));
#42097=CARTESIAN_POINT('Ctrl Pts',(1.67767784848676,14.0251785145865,9.6490282183982));
#42098=CARTESIAN_POINT('Ctrl Pts',(1.43858372990708,14.0262045191416,9.67560963771709));
#42099=CARTESIAN_POINT('Ctrl Pts',(1.19990821247035,14.0269327812144,9.69641204968543));
#42100=CARTESIAN_POINT('Ctrl Pts',(0.961875035736572,14.0274295673342,9.71152720644804));
#42101=CARTESIAN_POINT('Ctrl Pts',(0.725661536800911,14.0279225557033,9.72652681328793));
#42102=CARTESIAN_POINT('Ctrl Pts',(0.490080595180857,14.0281876071765,9.73592574969795));
#42103=CARTESIAN_POINT('Ctrl Pts',(0.25535085833806,14.0282936152756,9.73986490944068));
#42104=CARTESIAN_POINT('Ctrl Pts',(0.170488783179417,14.0283319404891,9.74128903777927));
#42105=CARTESIAN_POINT('Ctrl Pts',(0.0857379644516537,14.0283495164129,
9.74200003828909));
#42106=CARTESIAN_POINT('Ctrl Pts',(0.00110873407505763,14.0283497281836,
9.74200624557126));
#42107=CARTESIAN_POINT('Ctrl Pts',(0.000739158498271593,14.0283497291084,
9.74200627267844));
#42108=CARTESIAN_POINT('Ctrl Pts',(0.000369580473237724,14.0283497297032,
9.74200628634741));
#42109=CARTESIAN_POINT('Ctrl Pts',(8.91737066575231E-13,14.0283497299677,
9.7420062865774));
#42110=CARTESIAN_POINT('Ctrl Pts',(-0.229875715873488,14.0283498944901,
9.74200642962535));
#42111=CARTESIAN_POINT('Ctrl Pts',(-0.460698230103008,14.0282219407555,
9.7368030522104));
#42112=CARTESIAN_POINT('Ctrl Pts',(-0.692242317170722,14.0278986126043,
9.7262389182912));
#42113=CARTESIAN_POINT('Ctrl Pts',(-0.925634833270699,14.0275727033069,
9.71559045031673));
#42114=CARTESIAN_POINT('Ctrl Pts',(-1.15976048890447,14.0270482745718,9.69949530223137));
#42115=CARTESIAN_POINT('Ctrl Pts',(-1.39438862141758,14.0262607078353,9.67784538975412));
#42116=CARTESIAN_POINT('Ctrl Pts',(-1.63050058604344,14.0254681603796,9.65605855918853));
#42117=CARTESIAN_POINT('Ctrl Pts',(-1.86712140316056,14.0244091222216,9.6286465415942));
#42118=CARTESIAN_POINT('Ctrl Pts',(-2.10401600611877,14.0230222437544,9.59555206923531));
#42119=CARTESIAN_POINT('Ctrl Pts',(-2.34376748131239,14.0216186399818,9.56205848825154));
#42120=CARTESIAN_POINT('Ctrl Pts',(-2.58379938570262,14.0198792216485,9.52274461255295));
#42121=CARTESIAN_POINT('Ctrl Pts',(-2.82386804518254,14.017745249659,9.47760437142254));
#42122=CARTESIAN_POINT('Ctrl Pts',(-2.92799179665629,14.0168196929055,9.45802592557663));
#42123=CARTESIAN_POINT('Ctrl Pts',(-3.03212246239736,14.015819976852,9.43735210851414));
#42124=CARTESIAN_POINT('Ctrl Pts',(-3.13624016075678,14.0147416014962,9.41558544311034));
#42125=CARTESIAN_POINT('Ctrl Pts',(-3.39906091201799,14.0120194954027,9.36064059277251));
#42126=CARTESIAN_POINT('Ctrl Pts',(-3.66179324841398,14.0087772393006,9.29871252238622));
#42127=CARTESIAN_POINT('Ctrl Pts',(-3.92409365960145,14.0048094640642,9.22976650998086));
#42128=CARTESIAN_POINT('Ctrl Pts',(-4.19384459535778,14.0007289859664,9.15886211727017));
#42129=CARTESIAN_POINT('Ctrl Pts',(-4.46313872013994,13.9958811280336,9.08053601144839));
#42130=CARTESIAN_POINT('Ctrl Pts',(-4.7316024125131,13.9900514247656,8.99481051658923));
#42131=CARTESIAN_POINT('Ctrl Pts',(-5.02536872517533,13.9836722737607,8.90100542025272));
#42132=CARTESIAN_POINT('Ctrl Pts',(-5.31814069269643,13.9761172542124,8.79834071961033));
#42133=CARTESIAN_POINT('Ctrl Pts',(-5.60942878308013,13.967118242421,8.68691055918608));
#42134=CARTESIAN_POINT('Ctrl Pts',(-5.82848128650871,13.9603508663204,8.60311360213842));
#42135=CARTESIAN_POINT('Ctrl Pts',(-6.04669462191043,13.9527671398283,8.51436109383324));
#42136=CARTESIAN_POINT('Ctrl Pts',(-6.26386060039021,13.9442583526775,8.42071136781886));
#42137=CARTESIAN_POINT('Ctrl Pts',(6.38278051433227,13.9389660638327,8.36834463281926));
#42138=CARTESIAN_POINT('Ctrl Pts',(6.32403324549604,13.9421685246813,8.39503501693572));
#42139=CARTESIAN_POINT('Ctrl Pts',(5.68184080001437,13.9762293289878,8.68229415577496));
#42140=CARTESIAN_POINT('Ctrl Pts',(4.34156912266226,14.0269131243102,9.18193694262902));
#42141=CARTESIAN_POINT('Ctrl Pts',(2.26092021150987,14.0637866398188,9.66364676264392));
#42142=CARTESIAN_POINT('Ctrl Pts',(0.00240395732475112,14.0745321264826,
9.84161531252271));
#42143=CARTESIAN_POINT('Ctrl Pts',(-2.25657178139371,14.063833427226,9.66436170214786));
#42144=CARTESIAN_POINT('Ctrl Pts',(-4.338287360545,14.0270060790976,9.18297638358755));
#42145=CARTESIAN_POINT('Ctrl Pts',(-5.68009484646612,13.9763119235712,8.68302746369451));
#42146=CARTESIAN_POINT('Ctrl Pts',(-6.32334697022109,13.9422059231002,8.39534680690008));
#42147=CARTESIAN_POINT('Ctrl Pts',(-6.38277685455529,13.9389662535686,8.36834631006795));
#42148=CARTESIAN_POINT('Ctrl Pts',(6.17958116000266,13.4711650513731,7.96890660962997));
#42149=CARTESIAN_POINT('Ctrl Pts',(6.1226739972167,13.4744252864521,7.99459326956682));
#42150=CARTESIAN_POINT('Ctrl Pts',(5.50060489987548,13.5091207438235,8.27105239462829));
#42151=CARTESIAN_POINT('Ctrl Pts',(4.2025290500201,13.5611784708113,8.75195270223154));
#42152=CARTESIAN_POINT('Ctrl Pts',(2.1881646903414,13.5997630398516,9.21553749016288));
#42153=CARTESIAN_POINT('Ctrl Pts',(0.00232641633904755,13.61123690215,9.38677394813154));
#42154=CARTESIAN_POINT('Ctrl Pts',(-2.1839555556712,13.5998126299275,9.21622544229542));
#42155=CARTESIAN_POINT('Ctrl Pts',(-4.19935107275343,13.5612746813947,8.75295313615389));
#42156=CARTESIAN_POINT('Ctrl Pts',(-5.49891374142447,13.5092050955935,8.27175816634109));
#42157=CARTESIAN_POINT('Ctrl Pts',(-6.12200921769724,13.4744633603779,7.9948933334426));
#42158=CARTESIAN_POINT('Ctrl Pts',(-6.17957761500318,13.4711652453848,7.96890822259208));
#42159=CARTESIAN_POINT('Ctrl Pts',(6.17623978391479,12.827683761815,8.03328661654028));
#42160=CARTESIAN_POINT('Ctrl Pts',(6.11949336784761,12.8309117803229,8.05865899529169));
#42161=CARTESIAN_POINT('Ctrl Pts',(5.49914553135681,12.8652660029562,8.33176046636725));
#42162=CARTESIAN_POINT('Ctrl Pts',(4.20380863758019,12.9168465271217,8.80737082236057));
#42163=CARTESIAN_POINT('Ctrl Pts',(2.19033539306753,12.9551041637359,9.26687615010052));
#42164=CARTESIAN_POINT('Ctrl Pts',(0.00232951170839197,12.9664788697453,
9.43690573902765));
#42165=CARTESIAN_POINT('Ctrl Pts',(-2.1861248230667,12.9551533347932,9.26755884677766));
#42166=CARTESIAN_POINT('Ctrl Pts',(-4.20063536172209,12.9169418985469,8.80836121435707));
#42167=CARTESIAN_POINT('Ctrl Pts',(-5.49745868616426,12.8653495464233,8.33245792548714));
#42168=CARTESIAN_POINT('Ctrl Pts',(-6.11883046631787,12.8309494760218,8.05895538885718));
#42169=CARTESIAN_POINT('Ctrl Pts',(-6.17623624830767,12.8276839516259,8.03328821131818));
#42170=CARTESIAN_POINT('Ctrl Pts',(6.37340476901101,12.4448304032706,8.51423772060993));
#42171=CARTESIAN_POINT('Ctrl Pts',(6.3150446279235,12.4479587126635,8.54019211278279));
#42172=CARTESIAN_POINT('Ctrl Pts',(5.67700089063687,12.4812342950838,8.81958759200811));
#42173=CARTESIAN_POINT('Ctrl Pts',(4.34341280116177,12.5308239076974,9.30682734629494));
#42174=CARTESIAN_POINT('Ctrl Pts',(2.26536172811636,12.5669539973985,9.77894272739411));
#42175=CARTESIAN_POINT('Ctrl Pts',(0.00241050191523341,12.5774756952153,
9.95406181961986));
#42176=CARTESIAN_POINT('Ctrl Pts',(-2.26101109566215,12.5669998368927,9.77964527734846));
#42177=CARTESIAN_POINT('Ctrl Pts',(-4.34014276397128,12.5309149451459,9.30784321494086));
#42178=CARTESIAN_POINT('Ctrl Pts',(-5.6752653684065,12.481315031728,8.82030142532417));
#42179=CARTESIAN_POINT('Ctrl Pts',(-6.31436287541252,12.4479952405102,8.54049530748422));
#42180=CARTESIAN_POINT('Ctrl Pts',(-6.37340113191404,12.4448305832978,8.51423935521795));
#42181=CARTESIAN_POINT('',(-6.24994613508499,12.4626544380175,8.55169233715956));
#42182=CARTESIAN_POINT('Ctrl Pts',(-6.26386069634234,13.9442581018172,8.42071161317167));
#42183=CARTESIAN_POINT('Ctrl Pts',(-6.25435355654046,13.921854531114,8.40152900018476));
#42184=CARTESIAN_POINT('Ctrl Pts',(-6.24502268537409,13.897989865073,8.38292185729494));
#42185=CARTESIAN_POINT('Ctrl Pts',(-6.23597096179262,13.8726803662576,8.3651180362238));
#42186=CARTESIAN_POINT('Ctrl Pts',(-6.22714672203217,13.8480069343136,8.34776165272734));
#42187=CARTESIAN_POINT('Ctrl Pts',(-6.21858806970101,13.8219601170672,8.33116941791119));
#42188=CARTESIAN_POINT('Ctrl Pts',(-6.21039638859803,13.7946031445368,8.31556098565713));
#42189=CARTESIAN_POINT('Ctrl Pts',(-6.20233097480313,13.7676678548374,8.30019314317934));
#42190=CARTESIAN_POINT('Ctrl Pts',(-6.19462163292192,13.7394623695002,8.28577976268739));
#42191=CARTESIAN_POINT('Ctrl Pts',(-6.18736652633831,13.7100972516111,8.27252821600619));
#42192=CARTESIAN_POINT('Ctrl Pts',(-6.18023889772469,13.6812481021057,8.25950950949774));
#42193=CARTESIAN_POINT('Ctrl Pts',(-6.17355002094219,13.6512798568704,8.24761292078403));
#42194=CARTESIAN_POINT('Ctrl Pts',(-6.16738941348011,13.620345973838,8.23702171420378));
#42195=CARTESIAN_POINT('Ctrl Pts',(-6.16659032270645,13.6163335480056,8.23564793158376));
#42196=CARTESIAN_POINT('Ctrl Pts',(-6.1658001106991,13.6123049414575,8.23429608356915));
#42197=CARTESIAN_POINT('Ctrl Pts',(-6.16501896364319,13.6082605474023,8.23296654294361));
#42198=CARTESIAN_POINT('Ctrl Pts',(-6.15908815391333,13.5775537407484,8.22287208964124));
#42199=CARTESIAN_POINT('Ctrl Pts',(-6.15368082067904,13.5459334635958,8.21406594528197));
#42200=CARTESIAN_POINT('Ctrl Pts',(-6.14887156047967,13.5135955556427,8.20669591986198));
#42201=CARTESIAN_POINT('Ctrl Pts',(-6.14412391166845,13.4816719283307,8.19942031176982));
#42202=CARTESIAN_POINT('Ctrl Pts',(-6.13995938296957,13.449049524448,8.19354481691035));
#42203=CARTESIAN_POINT('Ctrl Pts',(-6.13643647742053,13.4159520378045,8.189177663298));
#42204=CARTESIAN_POINT('Ctrl Pts',(-6.13293425826425,13.3830488985821,8.18483615347701));
#42205=CARTESIAN_POINT('Ctrl Pts',(-6.13006636899709,13.3496769587491,8.18198574296722));
#42206=CARTESIAN_POINT('Ctrl Pts',(-6.12787339203533,13.316081408502,8.1806916287397));
#42207=CARTESIAN_POINT('Ctrl Pts',(-6.12568785535798,13.2825998405052,8.17940190515472));
#42208=CARTESIAN_POINT('Ctrl Pts',(-6.1241727979026,13.2488970071633,8.17965815933266));
#42209=CARTESIAN_POINT('Ctrl Pts',(-6.12334885433878,13.2152293057791,8.18147908566606));
#42210=CARTESIAN_POINT('Ctrl Pts',(-6.1225256521799,13.1815918994312,8.18329837348458));
#42211=CARTESIAN_POINT('Ctrl Pts',(-6.12239236539064,13.1479904376347,8.18667952416076));
#42212=CARTESIAN_POINT('Ctrl Pts',(-6.12294864311801,13.1146814724604,8.191593587105));
#42213=CARTESIAN_POINT('Ctrl Pts',(-6.12350763165346,13.0812101887036,8.19653159686738));
#42214=CARTESIAN_POINT('Ctrl Pts',(-6.12476287848253,13.0480351256725,8.20301730216947));
#42215=CARTESIAN_POINT('Ctrl Pts',(-6.1266928382439,13.0154042565278,8.21097459157634));
#42216=CARTESIAN_POINT('Ctrl Pts',(-6.12863026531057,12.9826471336302,8.21896266893571));
#42217=CARTESIAN_POINT('Ctrl Pts',(-6.13124748503553,12.9504391894584,8.22843331212406));
#42218=CARTESIAN_POINT('Ctrl Pts',(-6.13450288131641,12.9190064842205,8.23926726261598));
#42219=CARTESIAN_POINT('Ctrl Pts',(-6.13779568054161,12.8872126322519,8.25022569001086));
#42220=CARTESIAN_POINT('Ctrl Pts',(-6.14174118213299,12.8562125836447,8.26257835469243));
#42221=CARTESIAN_POINT('Ctrl Pts',(-6.14627889801488,12.826204107595,8.27616627166071));
#42222=CARTESIAN_POINT('Ctrl Pts',(-6.14958305285243,12.8043533232162,8.286060364361));
#42223=CARTESIAN_POINT('Ctrl Pts',(-6.15320081635984,12.7830275102378,8.29660860123681));
#42224=CARTESIAN_POINT('Ctrl Pts',(-6.15710430190698,12.7622886877713,8.30774088573614));
#42225=CARTESIAN_POINT('Ctrl Pts',(-6.16256073867545,12.733299193107,8.32330200559314));
#42226=CARTESIAN_POINT('Ctrl Pts',(-6.1685756007687,12.705458756018,8.34000451766156));
#42227=CARTESIAN_POINT('Ctrl Pts',(-6.17506225395425,12.6788942981287,8.35764310234325));
#42228=CARTESIAN_POINT('Ctrl Pts',(-6.18169729474581,12.651722156092,8.3756851843724));
#42229=CARTESIAN_POINT('Ctrl Pts',(-6.18882560675837,12.6258851317298,8.39470584497923));
#42230=CARTESIAN_POINT('Ctrl Pts',(-6.19634894750703,12.601465159828,8.41447879406655));
#42231=CARTESIAN_POINT('Ctrl Pts',(-6.20398372215225,12.5766834852314,8.43454461527502));
#42232=CARTESIAN_POINT('Ctrl Pts',(-6.2120249611779,12.5533609154971,8.45538439871226));
#42233=CARTESIAN_POINT('Ctrl Pts',(-6.22036981861811,12.5315294058142,8.47676724150478));
#42234=CARTESIAN_POINT('Ctrl Pts',(-6.22891479907769,12.5091743416349,8.49866287904461));
#42235=CARTESIAN_POINT('Ctrl Pts',(-6.23777780844621,12.4883823171592,8.5211272362734));
#42236=CARTESIAN_POINT('Ctrl Pts',(-6.24685350902485,12.4691365256179,8.54392966360548));
#42237=CARTESIAN_POINT('Ctrl Pts',(-6.24788171874652,12.4669561198417,8.54651300990006));
#42238=CARTESIAN_POINT('Ctrl Pts',(-6.24891266659523,12.4647955116567,8.54910071944511));
#42239=CARTESIAN_POINT('Ctrl Pts',(-6.24994620609389,12.4626546405112,8.55169247610414));
#42240=CARTESIAN_POINT('Ctrl Pts',(6.24994601334268,12.4626534654496,8.55169428461515));
#42241=CARTESIAN_POINT('Ctrl Pts',(6.23069497655085,12.4636500190818,8.56008041467674));
#42242=CARTESIAN_POINT('Ctrl Pts',(6.211425284112,12.4646384328761,8.56843158879158));
#42243=CARTESIAN_POINT('Ctrl Pts',(6.19213699687127,12.4656187797136,8.57674767820393));
#42244=CARTESIAN_POINT('Ctrl Pts',(5.88885444681381,12.4810334241091,8.70750707493049));
#42245=CARTESIAN_POINT('Ctrl Pts',(5.58097437610039,12.4944537936397,8.82959653937889));
#42246=CARTESIAN_POINT('Ctrl Pts',(5.26879164882413,12.5061905913634,8.94246194328229));
#42247=CARTESIAN_POINT('Ctrl Pts',(5.13451964215371,12.5112386713645,8.99100615454598));
#42248=CARTESIAN_POINT('Ctrl Pts',(4.99945172301877,12.5159752836543,9.03784334970954));
#42249=CARTESIAN_POINT('Ctrl Pts',(4.86361169851994,12.520425116014,9.08292645927752));
#42250=CARTESIAN_POINT('Ctrl Pts',(4.71266624403642,12.5253697703631,9.13302281702168));
#42251=CARTESIAN_POINT('Ctrl Pts',(4.56077038142756,12.5299567332287,9.1809571968488));
#42252=CARTESIAN_POINT('Ctrl Pts',(4.40795808112894,12.5342112095376,9.22667388688011));
#42253=CARTESIAN_POINT('Ctrl Pts',(4.32197583622981,12.5366050575669,9.25239710176902));
#42254=CARTESIAN_POINT('Ctrl Pts',(4.23570343975212,12.538893643089,9.27741816074338));
#42255=CARTESIAN_POINT('Ctrl Pts',(4.14914956176477,12.5410807812621,9.30172798252948));
#42256=CARTESIAN_POINT('Ctrl Pts',(4.02895850398687,12.5441179005297,9.33548525906989));
#42257=CARTESIAN_POINT('Ctrl Pts',(3.90822293847248,12.5469599285777,9.36787098065101));
#42258=CARTESIAN_POINT('Ctrl Pts',(3.78696267046352,12.5496164712603,9.39886142343057));
#42259=CARTESIAN_POINT('Ctrl Pts',(3.72633253645904,12.5509447426016,9.41435664482034));
#42260=CARTESIAN_POINT('Ctrl Pts',(3.66557122374829,12.5522266313763,9.42950303834137));
#42261=CARTESIAN_POINT('Ctrl Pts',(3.60468130682292,12.5534631219089,9.44429775672225));
#42262=CARTESIAN_POINT('Ctrl Pts',(3.57423634836023,12.5540813671752,9.45169511591269));
#42263=CARTESIAN_POINT('Ctrl Pts',(3.54375923868042,12.5546882621973,9.4590045558101));
#42264=CARTESIAN_POINT('Ctrl Pts',(3.51325030186749,12.5552839216038,9.46622572232529));
#42265=CARTESIAN_POINT('Ctrl Pts',(3.49799583346103,12.5555817513071,9.46983630558289));
#42266=CARTESIAN_POINT('Ctrl Pts',(3.48273340826245,12.5558767720639,9.47342482046282));
#42267=CARTESIAN_POINT('Ctrl Pts',(3.46746306711973,12.5561689974362,9.47699122308885));
#42268=CARTESIAN_POINT('Ctrl Pts',(3.45982789654837,12.5563151101224,9.47877442440187));
#42269=CARTESIAN_POINT('Ctrl Pts',(3.45219074699045,12.5564605239598,9.48055209764942));
#42270=CARTESIAN_POINT('Ctrl Pts',(3.44455162357435,12.5566052405941,9.48232423737314));
#42271=CARTESIAN_POINT('Ctrl Pts',(3.43691250015825,12.5567499572284,9.48409637709687));
#42272=CARTESIAN_POINT('Ctrl Pts',(3.43039508137458,12.5568729052858,9.4856040723575));
#42273=CARTESIAN_POINT('Ctrl Pts',(3.4216283368855,12.5570373005128,9.48762405051808));
#42274=CARTESIAN_POINT('Ctrl Pts',(3.12615752408291,12.5625780107953,9.55570457798095));
#42275=CARTESIAN_POINT('Ctrl Pts',(2.82904436899774,12.5671333706468,9.61510893169583));
#42276=CARTESIAN_POINT('Ctrl Pts',(2.5305765003445,12.5708912511799,9.66564787830496));
#42277=CARTESIAN_POINT('Ctrl Pts',(2.45380963084996,12.5718577898085,9.67864665347041));
#42278=CARTESIAN_POINT('Ctrl Pts',(2.37695303288142,12.5727715296055,9.69105871051769));
#42279=CARTESIAN_POINT('Ctrl Pts',(2.30001138902235,12.5736355847826,9.70288031846971));
#42280=CARTESIAN_POINT('Ctrl Pts',(2.00430329850994,12.5769563886242,9.74831403861067));
#42281=CARTESIAN_POINT('Ctrl Pts',(1.70734002773116,12.579543664529,9.78503027763991));
#42282=CARTESIAN_POINT('Ctrl Pts',(1.40947860217307,12.5814672979525,9.8129598758294));
#42283=CARTESIAN_POINT('Ctrl Pts',(1.11351805136661,12.583378655244,9.84071123453076));
#42284=CARTESIAN_POINT('Ctrl Pts',(0.816670228620736,12.5846347306945,9.85978783707557));
#42285=CARTESIAN_POINT('Ctrl Pts',(0.519277169781786,12.5853002264282,9.87007147871222));
#42286=CARTESIAN_POINT('Ctrl Pts',(0.34720187942253,12.5856852904646,9.87602172054868));
#42287=CARTESIAN_POINT('Ctrl Pts',(0.17494393792049,12.5858725678027,9.87902720484474));
#42288=CARTESIAN_POINT('Ctrl Pts',(0.00256942855689103,12.5858741620931,
9.87905705024713));
#42289=CARTESIAN_POINT('Ctrl Pts',(0.00208301752298114,12.5858741665919,
9.8790571344657));
#42290=CARTESIAN_POINT('Ctrl Pts',(0.00159660556107809,12.585874169612,
9.87905719498614));
#42291=CARTESIAN_POINT('Ctrl Pts',(0.00111019267267243,12.585874171153,
9.87905723180882));
#42292=CARTESIAN_POINT('Ctrl Pts',(-0.295689077035793,12.5858751114415,
9.87907970025826));
#42293=CARTESIAN_POINT('Ctrl Pts',(-0.59216539376131,12.5852965639793,9.87032024515954));
#42294=CARTESIAN_POINT('Ctrl Pts',(-0.887982512549591,12.5841115795841,
9.85287673127805));
#42295=CARTESIAN_POINT('Ctrl Pts',(-1.16622061432549,12.582997013226,9.83646980320515));
#42296=CARTESIAN_POINT('Ctrl Pts',(-1.44387582449546,12.5813459890709,9.81237963964323));
#42297=CARTESIAN_POINT('Ctrl Pts',(-1.72065714500414,12.5791334160587,9.78064720860151));
#42298=CARTESIAN_POINT('Ctrl Pts',(-1.91270535705508,12.5775981943529,9.75862926087877));
#42299=CARTESIAN_POINT('Ctrl Pts',(-2.10433775772286,12.5757815284213,9.73294467202123));
#42300=CARTESIAN_POINT('Ctrl Pts',(-2.29545568635781,12.5736541883739,9.70362171541517));
#42301=CARTESIAN_POINT('Ctrl Pts',(-2.38847948222357,12.5726187373949,9.6893492044635));
#42302=CARTESIAN_POINT('Ctrl Pts',(-2.48138138565884,12.5715096738354,9.67421459522921));
#42303=CARTESIAN_POINT('Ctrl Pts',(-2.57415306840246,12.5703203186287,9.65822585627093));
#42304=CARTESIAN_POINT('Ctrl Pts',(-2.71583889015522,12.5685038724371,9.63380700828738));
#42305=CARTESIAN_POINT('Ctrl Pts',(-2.85721797693568,12.5665035069359,9.6073921841135));
#42306=CARTESIAN_POINT('Ctrl Pts',(-2.99825373023941,12.5643006664828,9.5790023299836));
#42307=CARTESIAN_POINT('Ctrl Pts',(-3.06877160689128,12.5631992462562,9.56480740291865));
#42308=CARTESIAN_POINT('Ctrl Pts',(-3.13920364858881,12.5620471897453,9.55011870466143));
#42309=CARTESIAN_POINT('Ctrl Pts',(-3.20954536092081,12.5608417729686,9.53493913971815));
#42310=CARTESIAN_POINT('Ctrl Pts',(-3.24471621708681,12.5602390645802,9.52734935724652));
#42311=CARTESIAN_POINT('Ctrl Pts',(-3.27986449077428,12.5596230149951,9.51963685722513));
#42312=CARTESIAN_POINT('Ctrl Pts',(-3.31498962206888,12.5589932686438,9.51180200761284));
#42313=CARTESIAN_POINT('Ctrl Pts',(-3.33255218771618,12.5586783954681,9.50788458280669));
#42314=CARTESIAN_POINT('Ctrl Pts',(-3.35010896775377,12.5583600980292,9.50393657054786));
#42315=CARTESIAN_POINT('Ctrl Pts',(-3.36765989244758,12.5580383304446,9.49995801774782));
#42316=CARTESIAN_POINT('Ctrl Pts',(-3.37643535479449,12.5578774466524,9.4979687413478));
#42317=CARTESIAN_POINT('Ctrl Pts',(-3.38520935330468,12.5577156953191,9.49597182980904));
#42318=CARTESIAN_POINT('Ctrl Pts',(-3.39398187927851,12.5575530706168,9.49396728905644));
#42319=CARTESIAN_POINT('Ctrl Pts',(-3.40275440525234,12.5573904459144,9.49196274830384));
#42320=CARTESIAN_POINT('Ctrl Pts',(-3.41264857437856,12.5572058961111,9.48969190419738));
#42321=CARTESIAN_POINT('Ctrl Pts',(-3.42029503089472,12.5570625705361,9.48793078509275));
#42322=CARTESIAN_POINT('Ctrl Pts',(-3.73523036312535,12.5511594064357,9.41539540492774));
#42323=CARTESIAN_POINT('Ctrl Pts',(-4.04684827865571,12.5441153173257,9.33340063046015));
#42324=CARTESIAN_POINT('Ctrl Pts',(-4.35476458587455,12.5357286915261,9.24241813984974));
#42325=CARTESIAN_POINT('Ctrl Pts',(-4.37141519515592,12.5352751837836,9.23749825133756));
#42326=CARTESIAN_POINT('Ctrl Pts',(-4.38805498128561,12.5348177506726,9.23255206914417));
#42327=CARTESIAN_POINT('Ctrl Pts',(-4.40468388372678,12.5343563604153,9.22757966359974));
#42328=CARTESIAN_POINT('Ctrl Pts',(-4.72137612663838,12.5255693273601,9.13288175613993));
#42329=CARTESIAN_POINT('Ctrl Pts',(-5.03412129600066,12.5153470262873,9.02867719447994));
#42330=CARTESIAN_POINT('Ctrl Pts',(-5.34263369729778,12.5034361680417,8.91548494251033));
#42331=CARTESIAN_POINT('Ctrl Pts',(-5.62883951435732,12.4923865087679,8.81047690774881));
#42332=CARTESIAN_POINT('Ctrl Pts',(-5.91140270403815,12.4798837868993,8.69773306331674));
#42333=CARTESIAN_POINT('Ctrl Pts',(-6.19008882563368,12.4657244727602,8.5776282226717));
#42334=CARTESIAN_POINT('Ctrl Pts',(-6.21006122604612,12.4647097272467,8.56902075433024));
#42335=CARTESIAN_POINT('Ctrl Pts',(-6.23001371009115,12.4636864722795,8.5603754643636));
#42336=CARTESIAN_POINT('Ctrl Pts',(-6.24994620609389,12.4626546405112,8.55169247610414));
#42337=CARTESIAN_POINT('Ctrl Pts',(-6.25033451892106,13.9524682946008,8.43424269718798));
#42338=CARTESIAN_POINT('Ctrl Pts',(-6.28964915527219,13.9499438768096,8.41725253533479));
#42339=CARTESIAN_POINT('Ctrl Pts',(-6.41587003176774,13.9456274217175,8.35546025032207));
#42340=CARTESIAN_POINT('Ctrl Pts',(-6.61738868014126,13.9601645971529,8.21564074144287));
#42341=CARTESIAN_POINT('Ctrl Pts',(-6.82546143491885,14.0139067293176,7.99585604153587));
#42342=CARTESIAN_POINT('Ctrl Pts',(-6.97865008580523,14.0972105237428,7.74767876286032));
#42343=CARTESIAN_POINT('Ctrl Pts',(-7.07088219512303,14.1979515509549,7.49741012515146));
#42344=CARTESIAN_POINT('Ctrl Pts',(-7.10309704013408,14.2876054220639,7.30105159475886));
#42345=CARTESIAN_POINT('Ctrl Pts',(-7.10603159331704,14.3411724770656,7.19238285727497));
#42346=CARTESIAN_POINT('Ctrl Pts',(-7.10553695258355,14.3576106538258,7.15978428397002));
#42347=CARTESIAN_POINT('Ctrl Pts',(-6.05203636717249,13.4902976546902,8.02965348203525));
#42348=CARTESIAN_POINT('Ctrl Pts',(-6.08682726586427,13.4878645169164,8.01477622955758));
#42349=CARTESIAN_POINT('Ctrl Pts',(-6.19871067963014,13.4832750812962,7.96062311161307));
#42350=CARTESIAN_POINT('Ctrl Pts',(-6.37826045300425,13.4943571901332,7.83768099576627));
#42351=CARTESIAN_POINT('Ctrl Pts',(-6.56468542531687,13.5396514048005,7.64357855148817));
#42352=CARTESIAN_POINT('Ctrl Pts',(-6.70247684352513,13.611603280852,7.42378168844978));
#42353=CARTESIAN_POINT('Ctrl Pts',(-6.78559032245747,13.6996962165107,7.20196003959929));
#42354=CARTESIAN_POINT('Ctrl Pts',(-6.81459591395992,13.7785918003254,7.02819754060553));
#42355=CARTESIAN_POINT('Ctrl Pts',(-6.81722831460514,13.8258046273339,6.93233707607369));
#42356=CARTESIAN_POINT('Ctrl Pts',(-6.81678408764493,13.8402931100199,6.90361903188319));
#42357=CARTESIAN_POINT('Ctrl Pts',(-6.04019940720743,12.8475122295882,8.08818863513551));
#42358=CARTESIAN_POINT('Ctrl Pts',(-6.08811776273061,12.8443535265405,8.0679992039008));
#42359=CARTESIAN_POINT('Ctrl Pts',(-6.24139727010769,12.8387982128404,7.99491913859305));
#42360=CARTESIAN_POINT('Ctrl Pts',(-6.48332443625395,12.855390802314,7.83181228543884));
#42361=CARTESIAN_POINT('Ctrl Pts',(-6.72998275228084,12.9170968299401,7.57931248656608));
#42362=CARTESIAN_POINT('Ctrl Pts',(-6.90994194479098,13.0119770818171,7.29716053986814));
#42363=CARTESIAN_POINT('Ctrl Pts',(-7.01783236561899,13.1260881497257,7.01412193064447));
#42364=CARTESIAN_POINT('Ctrl Pts',(-7.05558995176488,13.2275881118917,6.79197606898948));
#42365=CARTESIAN_POINT('Ctrl Pts',(-7.05905913300314,13.2884728039491,6.66847100666564));
#42366=CARTESIAN_POINT('Ctrl Pts',(-7.05847594073483,13.3071939532727,6.631342309306));
#42367=CARTESIAN_POINT('Ctrl Pts',(-6.22296948742552,12.4591929883744,8.5705424543499));
#42368=CARTESIAN_POINT('Ctrl Pts',(-6.29279077977321,12.4549825546712,8.54120721875926));
#42369=CARTESIAN_POINT('Ctrl Pts',(-6.51521132942963,12.4484219402862,8.43543016078593));
#42370=CARTESIAN_POINT('Ctrl Pts',(-6.86168798984531,12.4757659175238,8.20227041545799));
#42371=CARTESIAN_POINT('Ctrl Pts',(-7.20973653489465,12.5676491290619,7.84677325666152));
#42372=CARTESIAN_POINT('Ctrl Pts',(-7.46091871314674,12.7042381878061,7.45368528454406));
#42373=CARTESIAN_POINT('Ctrl Pts',(-7.61072991218324,12.8654448707582,7.06115049381582));
#42374=CARTESIAN_POINT('Ctrl Pts',(-7.66328349318344,13.0076307346436,6.75235057956903));
#42375=CARTESIAN_POINT('Ctrl Pts',(-7.66816263515553,13.092970744036,6.57943675512195));
#42376=CARTESIAN_POINT('Ctrl Pts',(-7.667345053712,13.1192454833185,6.5272921268927));
#42377=CARTESIAN_POINT('',(-7.00000965177205,13.9487143132752,6.97711954466479));
#42378=CARTESIAN_POINT('',(-6.99999993499287,12.5220622648568,8.04448038251042));
#42379=CARTESIAN_POINT('Ctrl Pts',(-7.,13.9487143133546,6.97711954466507));
#42380=CARTESIAN_POINT('Ctrl Pts',(-7.,13.846910345019,7.02110369792794));
#42381=CARTESIAN_POINT('Ctrl Pts',(-7.,13.7565099975373,7.06259440190032));
#42382=CARTESIAN_POINT('Ctrl Pts',(-7.,13.6789127775256,7.10068312190857));
#42383=CARTESIAN_POINT('Ctrl Pts',(-7.,13.6401141675198,7.1197274819127));
#42384=CARTESIAN_POINT('Ctrl Pts',(-7.,13.604491505167,7.13788022505646));
#42385=CARTESIAN_POINT('Ctrl Pts',(-7.,13.5720954527481,7.15485418320256));
#42386=CARTESIAN_POINT('Ctrl Pts',(-7.,13.5558974265387,7.16334116227561));
#42387=CARTESIAN_POINT('Ctrl Pts',(-7.,13.540504937586,7.17153231301748));
#42388=CARTESIAN_POINT('Ctrl Pts',(-7.,13.5259184564153,7.17938775396613));
#42389=CARTESIAN_POINT('Ctrl Pts',(-7.,13.51862521583,7.18331547444047));
#42390=CARTESIAN_POINT('Ctrl Pts',(-7.,13.5115334771902,7.1871592674665));
#42391=CARTESIAN_POINT('Ctrl Pts',(-7.,13.5046429162458,7.19091413159631));
#42392=CARTESIAN_POINT('Ctrl Pts',(-7.,13.5011976357736,7.19279156366121));
#42393=CARTESIAN_POINT('Ctrl Pts',(-7.,13.4978026497252,7.19464676350206));
#42394=CARTESIAN_POINT('Ctrl Pts',(-7.,13.4944579155314,7.19647910844843));
#42395=CARTESIAN_POINT('Ctrl Pts',(-7.,13.4911131813377,7.19831145339479));
#42396=CARTESIAN_POINT('Ctrl Pts',(-7.,13.4892957406687,7.19930781525711));
#42397=CARTESIAN_POINT('Ctrl Pts',(-7.,13.4845744203103,7.20190695851936));
#42398=CARTESIAN_POINT('Ctrl Pts',(-7.,13.4090332945757,7.24349325071527));
#42399=CARTESIAN_POINT('Ctrl Pts',(-7.,13.3377847769944,7.28575717229597));
#42400=CARTESIAN_POINT('Ctrl Pts',(-7.,13.2713234786593,7.32831597848984));
#42401=CARTESIAN_POINT('Ctrl Pts',(-7.,13.2048621803243,7.3708747846837));
#42402=CARTESIAN_POINT('Ctrl Pts',(-7.,13.1444944017751,7.41273743687651));
#42403=CARTESIAN_POINT('Ctrl Pts',(-7.,13.0865047257911,7.45589780088873));
#42404=CARTESIAN_POINT('Ctrl Pts',(-7.,12.9705253738232,7.54221852891318));
#42405=CARTESIAN_POINT('Ctrl Pts',(-7.,12.862547855931,7.63579225294218));
#42406=CARTESIAN_POINT('Ctrl Pts',(-7.,12.7672508104679,7.73516747733596));
#42407=CARTESIAN_POINT('Ctrl Pts',(-7.,12.6719537650047,7.83454270172974));
#42408=CARTESIAN_POINT('Ctrl Pts',(-7.,12.5894810238525,7.93953389973554));
#42409=CARTESIAN_POINT('Ctrl Pts',(-7.,12.5220625166805,8.04448025538917));
#42410=CARTESIAN_POINT('Ctrl Pts',(-6.24994601297787,12.4626540898072,8.55169209823018));
#42411=CARTESIAN_POINT('Ctrl Pts',(-6.29982459974781,12.4600703735468,8.52996671717355));
#42412=CARTESIAN_POINT('Ctrl Pts',(-6.34869133122363,12.4586319660299,8.50671213387563));
#42413=CARTESIAN_POINT('Ctrl Pts',(-6.39656316448639,12.4582896059969,8.48199166741002));
#42414=CARTESIAN_POINT('Ctrl Pts',(-6.40601602277147,12.4582220029691,8.47711031964634));
#42415=CARTESIAN_POINT('Ctrl Pts',(-6.41543005269687,12.4581972219153,8.47217168167151));
#42416=CARTESIAN_POINT('Ctrl Pts',(-6.42480532433733,12.4582150091077,8.46717604859161));
#42417=CARTESIAN_POINT('Ctrl Pts',(-6.47308062566086,12.4583065992079,8.44145245342739));
#42418=CARTESIAN_POINT('Ctrl Pts',(-6.52033005210395,12.4595246094188,8.41422082064656));
#42419=CARTESIAN_POINT('Ctrl Pts',(-6.56658748121657,12.4618304449742,8.38551103548151));
#42420=CARTESIAN_POINT('Ctrl Pts',(-6.59417368647316,12.4632055592886,8.36838959052382));
#42421=CARTESIAN_POINT('Ctrl Pts',(-6.62140669136586,12.4649680995324,8.35074167140086));
#42422=CARTESIAN_POINT('Ctrl Pts',(-6.64828936293074,12.4671144548114,8.33256747406087));
#42423=CARTESIAN_POINT('Ctrl Pts',(-6.69395208409199,12.4707602391369,8.30169690736654));
#42424=CARTESIAN_POINT('Ctrl Pts',(-6.73859596814244,12.4755104312674,8.26931746786413));
#42425=CARTESIAN_POINT('Ctrl Pts',(-6.78220333696888,12.481366936842,8.23541025459223));
#42426=CARTESIAN_POINT('Ctrl Pts',(-6.80279898250507,12.4841329490125,8.21939596699677));
#42427=CARTESIAN_POINT('Ctrl Pts',(-6.8231629161368,12.4871460991754,8.20304046823201));
#42428=CARTESIAN_POINT('Ctrl Pts',(-6.84329031163055,12.4904084556441,8.18633971751031));
#42429=CARTESIAN_POINT('Ctrl Pts',(-6.88574258186573,12.4972893478318,8.15111485282334));
#42430=CARTESIAN_POINT('Ctrl Pts',(-6.92714539678634,12.5052775790726,8.11435523631283));
#42431=CARTESIAN_POINT('Ctrl Pts',(-6.96745644081089,12.5143953175279,8.07601416781882));
#42432=CARTESIAN_POINT('Ctrl Pts',(-6.97838520010813,12.5168672348728,8.06561949015891));
#42433=CARTESIAN_POINT('Ctrl Pts',(-6.98923346199965,12.5194222870681,8.05510847215563));
#42434=CARTESIAN_POINT('Ctrl Pts',(-6.99999980168616,12.522061165543,8.04447997453359));
#42435=CARTESIAN_POINT('Ctrl Pts',(-6.26385678721994,13.9442683198787,8.42070161672651));
#42436=CARTESIAN_POINT('Ctrl Pts',(-6.29456573149968,13.9363932840456,8.40064334074902));
#42437=CARTESIAN_POINT('Ctrl Pts',(-6.32505699633266,13.9291033776285,8.37895176101333));
#42438=CARTESIAN_POINT('Ctrl Pts',(-6.35516324043681,13.9224354844605,8.35562224165687));
#42439=CARTESIAN_POINT('Ctrl Pts',(-6.39907920397569,13.9127090319601,8.32159148319051));
#42440=CARTESIAN_POINT('Ctrl Pts',(-6.44217769161159,13.9043059353514,8.28407424509421));
#42441=CARTESIAN_POINT('Ctrl Pts',(-6.48397030176567,13.8972700933008,8.24317315549303));
#42442=CARTESIAN_POINT('Ctrl Pts',(-6.51466304337016,13.8921029290287,8.21313515188801));
#42443=CARTESIAN_POINT('Ctrl Pts',(-6.54465065466862,13.8876732740679,8.1812725167791));
#42444=CARTESIAN_POINT('Ctrl Pts',(-6.5737229708968,13.8840033212243,8.14763063810793));
#42445=CARTESIAN_POINT('Ctrl Pts',(-6.57468303811,13.8838821268423,8.14651966833004));
#42446=CARTESIAN_POINT('Ctrl Pts',(-6.57564210573341,13.883761761447,8.14540675847026));
#42447=CARTESIAN_POINT('Ctrl Pts',(-6.57660016725285,13.8836422247969,8.14429191158571));
#42448=CARTESIAN_POINT('Ctrl Pts',(-6.61458107806282,13.8789033737365,8.10009548032388));
#42449=CARTESIAN_POINT('Ctrl Pts',(-6.65098443579671,13.8754660854848,8.05285328625911));
#42450=CARTESIAN_POINT('Ctrl Pts',(-6.68538366622048,13.8733209517643,8.00276471114971));
#42451=CARTESIAN_POINT('Ctrl Pts',(-6.70990068011011,13.8717920724093,7.96706559007807));
#42452=CARTESIAN_POINT('Ctrl Pts',(-6.73339893888901,13.8709197261176,7.9299209974032));
#42453=CARTESIAN_POINT('Ctrl Pts',(-6.75570905449432,13.8707053657576,7.89140763570644));
#42454=CARTESIAN_POINT('Ctrl Pts',(-6.76177919350137,13.8706470425644,7.88092891550328));
#42455=CARTESIAN_POINT('Ctrl Pts',(-6.76776129395266,13.8706374583745,7.87034888571226));
#42456=CARTESIAN_POINT('Ctrl Pts',(-6.77365257560151,13.8706761862248,7.85966973489397));
#42457=CARTESIAN_POINT('Ctrl Pts',(-6.78330665419541,13.8707396497856,7.8421697463582));
#42458=CARTESIAN_POINT('Ctrl Pts',(-6.79271687941757,13.870932839958,7.82440357172246));
#42459=CARTESIAN_POINT('Ctrl Pts',(-6.80187061891861,13.8712539941027,7.80638101726204));
#42460=CARTESIAN_POINT('Ctrl Pts',(-6.80644748866912,13.8714145711751,7.79736974003183));
#42461=CARTESIAN_POINT('Ctrl Pts',(-6.81096023203815,13.8716071419432,7.78829436541889));
#42462=CARTESIAN_POINT('Ctrl Pts',(-6.81540721630231,13.8718315010089,7.77915614525578));
#42463=CARTESIAN_POINT('Ctrl Pts',(-6.81763070843439,13.8719436805418,7.77458703517423));
#42464=CARTESIAN_POINT('Ctrl Pts',(-6.81983776045167,13.8720638073409,7.77000221353246));
#42465=CARTESIAN_POINT('Ctrl Pts',(-6.82202816541374,13.8721918568295,7.7654018370919));
#42466=CARTESIAN_POINT('Ctrl Pts',(-6.82363152598122,13.8722855881278,7.76203439485721));
#42467=CARTESIAN_POINT('Ctrl Pts',(-6.82564555369224,13.8724098122046,7.75776604668181));
#42468=CARTESIAN_POINT('Ctrl Pts',(-6.82714766435398,13.8725074242894,7.75455631221724));
#42469=CARTESIAN_POINT('Ctrl Pts',(-6.82769763774233,13.8725431633667,7.75338112014642));
#42470=CARTESIAN_POINT('Ctrl Pts',(-6.82817948679385,13.8725750866858,7.75234811836397));
#42471=CARTESIAN_POINT('Ctrl Pts',(-6.8285492302672,13.8725997495507,7.75155420014755));
#42472=CARTESIAN_POINT('Ctrl Pts',(-6.8432998660531,13.8735836558616,7.71988143430211));
#42473=CARTESIAN_POINT('Ctrl Pts',(-6.85781064799793,13.8749528718461,7.6862938725749));
#42474=CARTESIAN_POINT('Ctrl Pts',(-6.87180028490507,13.8767952337077,7.65074685921025));
#42475=CARTESIAN_POINT('Ctrl Pts',(-6.87715735062103,13.8775007311863,7.63713480566915));
#42476=CARTESIAN_POINT('Ctrl Pts',(-6.88243753723721,13.8782756300721,7.6232356727681));
#42477=CARTESIAN_POINT('Ctrl Pts',(-6.88762322762864,13.8791249518407,7.60904793507498));
#42478=CARTESIAN_POINT('Ctrl Pts',(-6.90054947881501,13.881242036682,7.57368248759465));
#42479=CARTESIAN_POINT('Ctrl Pts',(-6.91289098172131,13.8838218102924,7.53652145582424));
#42480=CARTESIAN_POINT('Ctrl Pts',(-6.92437312452421,13.8869285469011,7.49757675561096));
#42481=CARTESIAN_POINT('Ctrl Pts',(-6.93225768998699,13.8890618828635,7.47083418294567));
#42482=CARTESIAN_POINT('Ctrl Pts',(-6.9397363802014,13.8914436322206,7.44325117588539));
#42483=CARTESIAN_POINT('Ctrl Pts',(-6.9467094345203,13.8940939133715,7.41484102592939));
#42484=CARTESIAN_POINT('Ctrl Pts',(-6.95354281588448,13.8966911083736,7.38699994218268));
#42485=CARTESIAN_POINT('Ctrl Pts',(-6.95989068062659,13.8995461624458,7.35836450547703));
#42486=CARTESIAN_POINT('Ctrl Pts',(-6.96564934887637,13.9026776268842,7.328955233001));
#42487=CARTESIAN_POINT('Ctrl Pts',(-6.97355724810228,13.9069778060463,7.28856992984403));
#42488=CARTESIAN_POINT('Ctrl Pts',(-6.98035516208629,13.9117996003484,7.24672344639869));
#42489=CARTESIAN_POINT('Ctrl Pts',(-6.98577699516258,13.9171733320292,7.20351888902676));
#42490=CARTESIAN_POINT('Ctrl Pts',(-6.99119882823886,13.9225470637101,7.16031433165482));
#42491=CARTESIAN_POINT('Ctrl Pts',(-6.99524529417623,13.9284726674529,7.11575137185419));
#42492=CARTESIAN_POINT('Ctrl Pts',(-6.99761122800613,13.9349758788666,7.0699751192112));
#42493=CARTESIAN_POINT('Ctrl Pts',(-6.99918436197109,13.9392999316473,7.03953801361207));
#42494=CARTESIAN_POINT('Ctrl Pts',(-7.00001350599334,13.9438793370277,7.00856523949188));
#42495=CARTESIAN_POINT('Ctrl Pts',(-7.00001296810904,13.9487143133882,6.97711954462543));
#42496=CARTESIAN_POINT('Ctrl Pts',(-6.23413001410206,24.3933910200767,11.8700319068232));
#42497=CARTESIAN_POINT('Ctrl Pts',(-6.23490531438389,23.8924703817557,11.9504777604879));
#42498=CARTESIAN_POINT('Ctrl Pts',(-6.23649310959702,22.7260279288224,12.0627647819659));
#42499=CARTESIAN_POINT('Ctrl Pts',(-6.23803996453712,20.8893409401919,11.9701373429924));
#42500=CARTESIAN_POINT('Ctrl Pts',(-6.23759277150523,18.9411611629796,11.5416381740992));
#42501=CARTESIAN_POINT('Ctrl Pts',(-6.23570360012082,17.0892587227143,10.7961451394149));
#42502=CARTESIAN_POINT('Ctrl Pts',(-6.23204977718706,15.3875854470211,9.75631584382835));
#42503=CARTESIAN_POINT('Ctrl Pts',(-6.22726122721249,14.0755190719303,8.61699454170999));
#42504=CARTESIAN_POINT('Ctrl Pts',(-6.22400168396393,13.3673833256599,7.8135002823412));
#42505=CARTESIAN_POINT('Ctrl Pts',(-6.22266615802228,13.1134096685017,7.49367917896873));
#42506=CARTESIAN_POINT('Ctrl Pts',(-6.72599000738659,24.374566153822,11.7530859083551));
#42507=CARTESIAN_POINT('Ctrl Pts',(-6.72668316439776,23.8785346950644,11.8323453484187));
#42508=CARTESIAN_POINT('Ctrl Pts',(-6.72805142643041,22.7235345615009,11.9427140669528));
#42509=CARTESIAN_POINT('Ctrl Pts',(-6.72941897542137,20.9054832736021,11.8502317181525));
#42510=CARTESIAN_POINT('Ctrl Pts',(-6.72902397759863,18.9767992612483,11.4262601894422));
#42511=CARTESIAN_POINT('Ctrl Pts',(-6.7273679204602,17.1431694184818,10.6891575760481));
#42512=CARTESIAN_POINT('Ctrl Pts',(-6.72416424438668,15.4573960102263,9.66125578100212));
#42513=CARTESIAN_POINT('Ctrl Pts',(-6.71993337962548,14.1564668032532,8.53485925833108));
#42514=CARTESIAN_POINT('Ctrl Pts',(-6.71707886547193,13.4537901856661,7.74006802512467));
#42515=CARTESIAN_POINT('Ctrl Pts',(-6.7158901469348,13.2016825422521,7.42368980520173));
#42516=CARTESIAN_POINT('Ctrl Pts',(-7.02718522254093,24.3100157396903,11.3520761820925));
#42517=CARTESIAN_POINT('Ctrl Pts',(-7.02756391671898,23.83092546813,11.4283598774116));
#42518=CARTESIAN_POINT('Ctrl Pts',(-7.02824882763447,22.7152040919926,11.5344319762806));
#42519=CARTESIAN_POINT('Ctrl Pts',(-7.02897714962795,20.9601377869518,11.4446324087422));
#42520=CARTESIAN_POINT('Ctrl Pts',(-7.02876722583613,19.0974452998546,11.0353399720625));
#42521=CARTESIAN_POINT('Ctrl Pts',(-7.02790268849586,17.3268264235393,10.3242145754422));
#42522=CARTESIAN_POINT('Ctrl Pts',(-7.02622933165022,15.6982356397987,9.33267256354404));
#42523=CARTESIAN_POINT('Ctrl Pts',(-7.0239793056009,14.4407048288934,8.24599539969497));
#42524=CARTESIAN_POINT('Ctrl Pts',(-7.02249262647073,13.7610260792249,7.47887533837767));
#42525=CARTESIAN_POINT('Ctrl Pts',(-7.02184966906143,13.5171517734752,7.17356121380424));
#42526=CARTESIAN_POINT('Ctrl Pts',(-6.99838062545647,24.2298260444632,10.8539091310108));
#42527=CARTESIAN_POINT('Ctrl Pts',(-6.99835912987599,23.7718327257578,10.9268138865563));
#42528=CARTESIAN_POINT('Ctrl Pts',(-6.99821532191765,22.70491909819,11.0282119310016));
#42529=CARTESIAN_POINT('Ctrl Pts',(-6.99814245128683,21.0278311164464,10.9423807653247));
#42530=CARTESIAN_POINT('Ctrl Pts',(-6.99816421467864,19.2468686121879,10.5510777432818));
#42531=CARTESIAN_POINT('Ctrl Pts',(-6.99828068958999,17.5546300565824,9.87141076730067));
#42532=CARTESIAN_POINT('Ctrl Pts',(-6.99850456871779,15.9978504212263,8.92371734687288));
#42533=CARTESIAN_POINT('Ctrl Pts',(-6.9987352349692,14.7957477561672,7.885044829661));
#42534=CARTESIAN_POINT('Ctrl Pts',(-6.99894167922838,14.1458833108553,7.15166848879572));
#42535=CARTESIAN_POINT('Ctrl Pts',(-6.99898903110029,13.9127708057857,6.8598833748166));
#42536=CARTESIAN_POINT('',(-7.0000030891987,24.1259430621517,10.927769589406));
#42537=CARTESIAN_POINT('Origin',(-5.99998370357417,24.1259473086569,10.9277595201361));
#42538=CARTESIAN_POINT('Ctrl Pts',(-7.00001101651647,24.1259401091757,10.9277661762092));
#42539=CARTESIAN_POINT('Ctrl Pts',(-7.00001786894362,23.9375950085174,10.9560764177985));
#42540=CARTESIAN_POINT('Ctrl Pts',(-7.00001802523644,23.7511663645914,10.9791078948017));
#42541=CARTESIAN_POINT('Ctrl Pts',(-7.0000155683334,23.5669992469552,10.9972403495527));
#42542=CARTESIAN_POINT('Ctrl Pts',(-7.00001306404721,23.3792803335476,11.0157225017793));
#42543=CARTESIAN_POINT('Ctrl Pts',(-7.00000784335981,23.1939109276873,11.0291149016377));
#42544=CARTESIAN_POINT('Ctrl Pts',(-7.00000354817182,23.0112027161862,11.0378133545419));
#42545=CARTESIAN_POINT('Ctrl Pts',(-7.00000225617267,22.9562438056513,11.0404298625303));
#42546=CARTESIAN_POINT('Ctrl Pts',(-7.00000104339791,22.901525326951,11.0426216090387));
#42547=CARTESIAN_POINT('Ctrl Pts',(-6.99999999754011,22.8470548580183,11.0443992462048));
#42548=CARTESIAN_POINT('Ctrl Pts',(-6.99999887667154,22.7886776712689,11.0463043786345));
#42549=CARTESIAN_POINT('Ctrl Pts',(-6.99999794691878,22.7305853409417,11.0477338782857));
#42550=CARTESIAN_POINT('Ctrl Pts',(-6.99999718088504,22.672784885931,11.0487021582321));
#42551=CARTESIAN_POINT('Ctrl Pts',(-6.99999462213136,22.4797162023915,11.0519364672786));
#42552=CARTESIAN_POINT('Ctrl Pts',(-6.99999387749987,22.2899077714107,11.0500263120017));
#42553=CARTESIAN_POINT('Ctrl Pts',(-6.99999403436582,22.1035888683532,11.0434957473627));
#42554=CARTESIAN_POINT('Ctrl Pts',(-6.99999406718812,22.0646038986033,11.0421293059511));
#42555=CARTESIAN_POINT('Ctrl Pts',(-6.99999414005244,22.025771533904,11.0405605106518));
#42556=CARTESIAN_POINT('Ctrl Pts',(-6.99999424550263,21.9870936117406,11.0387940509209));
#42557=CARTESIAN_POINT('Ctrl Pts',(-6.99999432423886,21.958214062736,11.0374750927786));
#42558=CARTESIAN_POINT('Ctrl Pts',(-6.99999441864918,21.9301065612872,11.0360814530954));
#42559=CARTESIAN_POINT('Ctrl Pts',(-6.99999453140906,21.901184348489,11.0345337171186));
#42560=CARTESIAN_POINT('Ctrl Pts',(-6.99999463684116,21.8741416641965,11.0330865617547));
#42561=CARTESIAN_POINT('Ctrl Pts',(-6.99999475849241,21.8463866742734,11.0315045689661));
#42562=CARTESIAN_POINT('Ctrl Pts',(-6.9999949035289,21.816624792391,11.0296819396473));
#42563=CARTESIAN_POINT('Ctrl Pts',(-6.99999520368225,21.7550325096593,11.025910004097));
#42564=CARTESIAN_POINT('Ctrl Pts',(-6.99999556267899,21.6935868205477,11.021626914985));
#42565=CARTESIAN_POINT('Ctrl Pts',(-6.99999595372439,21.6322954774274,11.0168388649797));
#42566=CARTESIAN_POINT('Ctrl Pts',(-6.99999673581519,21.5097127911868,11.0072627649692));
#42567=CARTESIAN_POINT('Ctrl Pts',(-6.99999764539657,21.3877474889111,10.9956668213854));
#42568=CARTESIAN_POINT('Ctrl Pts',(-6.99999847634418,21.2664589639591,10.9821001701665));
#42569=CARTESIAN_POINT('Ctrl Pts',(-6.99999902467301,21.1864226357584,10.9731477573148));
#42570=CARTESIAN_POINT('Ctrl Pts',(-6.99999953898571,21.1066809504165,10.9633371977035));
#42571=CARTESIAN_POINT('Ctrl Pts',(-6.99999996276695,21.0272503077224,10.9526825062929));
#42572=CARTESIAN_POINT('Ctrl Pts',(-7.00000126736565,20.7827252950085,10.9198823366822));
#42573=CARTESIAN_POINT('Ctrl Pts',(-7.00000171384875,20.5411518142187,10.8790835349701));
#42574=CARTESIAN_POINT('Ctrl Pts',(-7.0000017064317,20.3030234396079,10.8307721963177));
#42575=CARTESIAN_POINT('Ctrl Pts',(-7.00000169893534,20.0623489134957,10.7819442960097));
#42576=CARTESIAN_POINT('Ctrl Pts',(-7.00000122941436,19.8251935168243,10.7254423532093));
#42577=CARTESIAN_POINT('Ctrl Pts',(-7.00000072342785,19.5920157773719,10.6617527004579));
#42578=CARTESIAN_POINT('Ctrl Pts',(-7.00000046988916,19.4751755477949,10.6298392182077));
#42579=CARTESIAN_POINT('Ctrl Pts',(-7.00000020716688,19.3593332333778,10.5961208093747));
#42580=CARTESIAN_POINT('Ctrl Pts',(-6.99999998766512,19.2445418371312,10.5606572112207));
#42581=CARTESIAN_POINT('Ctrl Pts',(-6.99999993928862,19.2192426968463,10.5528413071195));
#42582=CARTESIAN_POINT('Ctrl Pts',(-6.99999989300543,19.1939945906656,10.5449406307592));
#42583=CARTESIAN_POINT('Ctrl Pts',(-6.99999984878294,19.1687979878635,10.5369559348259));
#42584=CARTESIAN_POINT('Ctrl Pts',(-6.9999996537447,19.0576712367164,10.5017403414804));
#42585=CARTESIAN_POINT('Ctrl Pts',(-6.99999949863667,18.9475464918459,10.4648905456778));
#42586=CARTESIAN_POINT('Ctrl Pts',(-6.99999938184581,18.8384625268113,10.4264702917995));
#42587=CARTESIAN_POINT('Ctrl Pts',(-6.99999932345038,18.7839205442939,10.4072601648604));
#42588=CARTESIAN_POINT('Ctrl Pts',(-6.99999927466556,18.7296387567356,10.3876574234024));
#42589=CARTESIAN_POINT('Ctrl Pts',(-6.9999992354737,18.6756217453312,10.3676698870215));
#42590=CARTESIAN_POINT('Ctrl Pts',(-6.99999921587777,18.648613239629,10.3576761188311));
#42591=CARTESIAN_POINT('Ctrl Pts',(-6.99999919868211,18.6216709279653,10.34758615191));
#42592=CARTESIAN_POINT('Ctrl Pts',(-6.99999918389647,18.5947953751795,10.3374009592937));
#42593=CARTESIAN_POINT('Ctrl Pts',(-6.99999917283135,18.5746825369799,10.3297786739865));
#42594=CARTESIAN_POINT('Ctrl Pts',(-6.9999991626883,18.5536617117961,10.3217399587041));
#42595=CARTESIAN_POINT('Ctrl Pts',(-6.99999915445983,18.5338560065227,10.3140993759427));
#42596=CARTESIAN_POINT('Ctrl Pts',(-6.9999991516931,18.5271965619125,10.3115303163214));
#42597=CARTESIAN_POINT('Ctrl Pts',(-6.99999914913279,18.5206743326982,10.3090066889746));
#42598=CARTESIAN_POINT('Ctrl Pts',(-6.99999914678741,18.5143695538256,10.3065606748832));
#42599=CARTESIAN_POINT('Ctrl Pts',(-6.99999907529418,18.3221833823898,10.231999759582));
#42600=CARTESIAN_POINT('Ctrl Pts',(-6.99999912491852,18.1296184436268,10.1510712626572));
#42601=CARTESIAN_POINT('Ctrl Pts',(-6.99999933315952,17.9371557774712,10.0634928028401));
#42602=CARTESIAN_POINT('Ctrl Pts',(-6.99999947285727,17.8080428721846,10.0047410999078));
#42603=CARTESIAN_POINT('Ctrl Pts',(-6.99999968443228,17.6789770014193,9.94299687733446));
#42604=CARTESIAN_POINT('Ctrl Pts',(-6.99999998816768,17.55011631383,9.87817756873086));
#42605=CARTESIAN_POINT('Ctrl Pts',(-7.00000042903666,17.3630762739412,9.78409297013374));
#42606=CARTESIAN_POINT('Ctrl Pts',(-7.00000106780699,17.1764663325097,9.68352877151032));
#42607=CARTESIAN_POINT('Ctrl Pts',(-7.0000015333121,16.9908081968233,9.57627840680166));
#42608=CARTESIAN_POINT('Ctrl Pts',(-7.00000199134818,16.8081289474422,9.47074887507177));
#42609=CARTESIAN_POINT('Ctrl Pts',(-7.0000022813204,16.6263711747535,9.35874596463026));
#42610=CARTESIAN_POINT('Ctrl Pts',(-7.00000202662872,16.4460793027373,9.24008888867506));
#42611=CARTESIAN_POINT('Ctrl Pts',(-7.00000181209412,16.2942139385447,9.14014040041301));
#42612=CARTESIAN_POINT('Ctrl Pts',(-7.00000121063197,16.1433894203617,9.03547088641571));
#42613=CARTESIAN_POINT('Ctrl Pts',(-6.99999998662461,15.9939582652679,8.92598176502494));
#42614=CARTESIAN_POINT('Ctrl Pts',(-6.99999852881509,15.8159837142825,8.79557872286767));
#42615=CARTESIAN_POINT('Ctrl Pts',(-6.99999617286935,15.6399850843186,8.65833774103931));
#42616=CARTESIAN_POINT('Ctrl Pts',(-6.99999449845862,15.4665283599749,8.51417822432004));
#42617=CARTESIAN_POINT('Ctrl Pts',(-6.99999284827035,15.2955809060811,8.37210415696424));
#42618=CARTESIAN_POINT('Ctrl Pts',(-6.99999186158984,15.127102326539,8.223310223894));
#42619=CARTESIAN_POINT('Ctrl Pts',(-6.99999320068044,14.9616764910547,8.06774693213457));
#42620=CARTESIAN_POINT('Ctrl Pts',(-6.99999413396005,14.8463829026477,7.95932704669855));
#42621=CARTESIAN_POINT('Ctrl Pts',(-6.99999620011851,14.732573021617,7.84761958458279));
#42622=CARTESIAN_POINT('Ctrl Pts',(-6.99999999965513,14.6204569866519,7.73261614629688));
#42623=CARTESIAN_POINT('Ctrl Pts',(-7.00000506883531,14.4708765406778,7.5791834496027));
#42624=CARTESIAN_POINT('Ctrl Pts',(-7.00001329848849,14.3243093935676,7.41988229083372));
#42625=CARTESIAN_POINT('Ctrl Pts',(-7.00001657716699,14.1813266553594,7.25479670165536));
#42626=CARTESIAN_POINT('Ctrl Pts',(-7.00001838080138,14.1026703972017,7.16398144043396));
#42627=CARTESIAN_POINT('Ctrl Pts',(-7.00001867122214,14.0250995430186,7.07141626669052));
#42628=CARTESIAN_POINT('Ctrl Pts',(-7.00001598720713,13.9487143130816,6.97711954471195));
#42629=CARTESIAN_POINT('Origin',(-5.999994980806,24.1259380084193,10.9277770011849));
#42630=CARTESIAN_POINT('Origin',(-6.,24.1259427055443,10.9277790621896));
#42631=CARTESIAN_POINT('Ctrl Pts',(-7.10781850275369,15.2163810752001,5.10138230547117));
#42632=CARTESIAN_POINT('Ctrl Pts',(-7.10965592212001,15.243638120146,5.01817377406916));
#42633=CARTESIAN_POINT('Ctrl Pts',(-7.09650767610584,15.3063332046137,4.83995160005142));
#42634=CARTESIAN_POINT('Ctrl Pts',(-7.01932069430837,15.4151469112539,4.57119042040278));
#42635=CARTESIAN_POINT('Ctrl Pts',(-6.87393092186964,15.5377052608318,4.31264986078896));
#42636=CARTESIAN_POINT('Ctrl Pts',(-6.66554646305825,15.6627867794142,4.09583198591426));
#42637=CARTESIAN_POINT('Ctrl Pts',(-6.44497302456871,15.7638564025997,3.96342727449913));
#42638=CARTESIAN_POINT('Ctrl Pts',(-6.29831085196003,15.8188935726671,3.91388110101737));
#42639=CARTESIAN_POINT('Ctrl Pts',(-6.24287183837156,15.8381896251399,3.89997079786695));
#42640=CARTESIAN_POINT('Ctrl Pts',(-6.8148660709738,14.6693917981612,4.91526501001416));
#42641=CARTESIAN_POINT('Ctrl Pts',(-6.81651061812386,14.6933027372077,4.84219421584678));
#42642=CARTESIAN_POINT('Ctrl Pts',(-6.80473712287996,14.7486587038382,4.68533569305599));
#42643=CARTESIAN_POINT('Ctrl Pts',(-6.73538317691255,14.8455315157831,4.44862592495412));
#42644=CARTESIAN_POINT('Ctrl Pts',(-6.60489820389822,14.9550819895903,4.221513592739));
#42645=CARTESIAN_POINT('Ctrl Pts',(-6.41858679306974,15.0669053982178,4.03209942015559));
#42646=CARTESIAN_POINT('Ctrl Pts',(-6.22251415808462,15.1569461567156,3.91737098109664));
#42647=CARTESIAN_POINT('Ctrl Pts',(-6.09292710476668,15.2057053040373,3.87479263718418));
#42648=CARTESIAN_POINT('Ctrl Pts',(-6.0440630425918,15.2227571048321,3.86287802597435));
#42649=CARTESIAN_POINT('Ctrl Pts',(-7.05538133470317,14.0958527991573,4.73239253440706));
#42650=CARTESIAN_POINT('Ctrl Pts',(-7.05754283669283,14.1268236090183,4.63786043739041));
#42651=CARTESIAN_POINT('Ctrl Pts',(-7.04209110197715,14.1976751412647,4.43640307164316));
#42652=CARTESIAN_POINT('Ctrl Pts',(-6.95206588367742,14.3202071651059,4.13340471860375));
#42653=CARTESIAN_POINT('Ctrl Pts',(-6.78206029032806,14.4587309981229,3.84080046654608));
#42654=CARTESIAN_POINT('Ctrl Pts',(-6.53634720729367,14.6016134734994,3.59312827978541));
#42655=CARTESIAN_POINT('Ctrl Pts',(-6.27298555123814,14.7190635414326,3.43984981302298));
#42656=CARTESIAN_POINT('Ctrl Pts',(-6.09561259560824,14.7842427841826,3.38184915974059));
#42657=CARTESIAN_POINT('Ctrl Pts',(-6.02821751691175,14.8072801448996,3.36552349019884));
#42658=CARTESIAN_POINT('Ctrl Pts',(-7.66703304724494,13.8868460483238,4.67749851121142));
#42659=CARTESIAN_POINT('Ctrl Pts',(-7.67007102559788,13.9305009829184,4.54444214041405));
#42660=CARTESIAN_POINT('Ctrl Pts',(-7.6483805489724,14.0291874424256,4.26262996939523));
#42661=CARTESIAN_POINT('Ctrl Pts',(-7.52318689543652,14.1975988325363,3.83989894765035));
#42662=CARTESIAN_POINT('Ctrl Pts',(-7.28601521757398,14.3874509907575,3.42923973707209));
#42663=CARTESIAN_POINT('Ctrl Pts',(-6.93967854664297,14.5846684088355,3.07710723531338));
#42664=CARTESIAN_POINT('Ctrl Pts',(-6.5628372219494,14.7493950807724,2.85516467155866));
#42665=CARTESIAN_POINT('Ctrl Pts',(-6.30520104433745,14.8425662279459,2.76979835072563));
#42666=CARTESIAN_POINT('Ctrl Pts',(-6.20672728843964,14.8757629841358,2.74564283123929));
#42667=CARTESIAN_POINT('',(-6.26386059984685,15.8144217559904,3.90573753014116));
#42668=CARTESIAN_POINT('',(-6.24994610153646,14.8593869932042,2.76546780225979));
#42669=CARTESIAN_POINT('Ctrl Pts',(-6.26385533697638,15.8144219674758,3.90575676779332));
#42670=CARTESIAN_POINT('Ctrl Pts',(-6.25431920294586,15.785024950916,3.90347124430492));
#42671=CARTESIAN_POINT('Ctrl Pts',(-6.2449664157803,15.7549995043499,3.89974752383157));
#42672=CARTESIAN_POINT('Ctrl Pts',(-6.23589798149847,15.724518813589,3.89443552233759));
#42673=CARTESIAN_POINT('Ctrl Pts',(-6.22705591741019,15.6947989950639,3.88925612133107));
#42674=CARTESIAN_POINT('Ctrl Pts',(-6.21848448219056,15.6646466824088,3.88256606616677));
#42675=CARTESIAN_POINT('Ctrl Pts',(-6.21028344947388,15.6342624944109,3.87425425030962));
#42676=CARTESIAN_POINT('Ctrl Pts',(-6.20220888165538,15.6043468490192,3.86607060769386));
#42677=CARTESIAN_POINT('Ctrl Pts',(-6.19449370857798,15.5742068731115,3.85631421861257));
#42678=CARTESIAN_POINT('Ctrl Pts',(-6.18723461420234,15.5440679323731,3.84491615956717));
#42679=CARTESIAN_POINT('Ctrl Pts',(-6.18010313606172,15.5144588398423,3.83371848052878));
#42680=CARTESIAN_POINT('Ctrl Pts',(-6.1734121821419,15.4848513800312,3.82093591445899));
#42681=CARTESIAN_POINT('Ctrl Pts',(-6.16724990086697,15.4554841750101,3.80654694090074));
#42682=CARTESIAN_POINT('Ctrl Pts',(-6.16645383918201,15.4516904327791,3.80468813082299));
#42683=CARTESIAN_POINT('Ctrl Pts',(-6.16566659105089,15.4479007265279,3.80280257837661));
#42684=CARTESIAN_POINT('Ctrl Pts',(-6.16488833747526,15.4441155924648,3.80089029683913));
#42685=CARTESIAN_POINT('Ctrl Pts',(-6.1589564514681,15.4152651194468,3.78631479542259));
#42686=CARTESIAN_POINT('Ctrl Pts',(-6.15354800793364,15.3866797106104,3.77018240242601));
#42687=CARTESIAN_POINT('Ctrl Pts',(-6.14873760388498,15.3586023645955,3.75252708013633));
#42688=CARTESIAN_POINT('Ctrl Pts',(-6.14398882657536,15.3308847212704,3.73509794257631));
#42689=CARTESIAN_POINT('Ctrl Pts',(-6.1398231365136,15.3036630123238,3.71618466794446));
#42690=CARTESIAN_POINT('Ctrl Pts',(-6.13629903821808,15.2771719432391,3.69586890326284));
#42691=CARTESIAN_POINT('Ctrl Pts',(-6.13279563454213,15.2508364380891,3.67567243917567));
#42692=CARTESIAN_POINT('Ctrl Pts',(-6.1299265293013,15.2252238223815,3.65409012001848));
#42693=CARTESIAN_POINT('Ctrl Pts',(-6.12773230732132,15.2005535737717,3.63124922072373));
#42694=CARTESIAN_POINT('Ctrl Pts',(-6.1255455309916,15.1759670386806,3.60848582741941));
#42695=CARTESIAN_POINT('Ctrl Pts',(-6.12402920434441,15.1523172315261,3.58447280976846));
#42696=CARTESIAN_POINT('Ctrl Pts',(-6.12320396530117,15.129798671608,3.5593782495565));
#42697=CARTESIAN_POINT('Ctrl Pts',(-6.12237946933404,15.107300388244,3.53430628542572));
#42698=CARTESIAN_POINT('Ctrl Pts',(-6.12224486166197,15.0859319388221,3.50815534111493));
#42699=CARTESIAN_POINT('Ctrl Pts',(-6.12279979543817,15.0658542612884,3.48112729768537));
#42700=CARTESIAN_POINT('Ctrl Pts',(-6.12335743311654,15.0456787557289,3.45396756073066));
#42701=CARTESIAN_POINT('Ctrl Pts',(-6.12461130491849,15.0268071072028,3.4259229058496));
#42702=CARTESIAN_POINT('Ctrl Pts',(-6.12653987018332,15.0093608390953,3.3972224952509));
#42703=CARTESIAN_POINT('Ctrl Pts',(-6.12847589670216,14.9918470746782,3.36841104819527));
#42704=CARTESIAN_POINT('Ctrl Pts',(-6.13109169581639,14.9757699798465,3.33893960549484));
#42705=CARTESIAN_POINT('Ctrl Pts',(-6.13434565659836,14.9612050732441,3.30905234390152));
#42706=CARTESIAN_POINT('Ctrl Pts',(-6.13763700560679,14.9464728148933,3.27882167567869));
#42707=CARTESIAN_POINT('Ctrl Pts',(-6.14158104247447,14.9332877444539,3.24816644452735));
#42708=CARTESIAN_POINT('Ctrl Pts',(-6.14611728449022,14.9216772847504,3.21733891367305));
#42709=CARTESIAN_POINT('Ctrl Pts',(-6.14942119404141,14.9132209659352,3.19488610509814));
#42710=CARTESIAN_POINT('Ctrl Pts',(-6.15303886477687,14.9055988304255,3.17234191617605));
#42711=CARTESIAN_POINT('Ctrl Pts',(-6.15694239071124,14.8988051599248,3.1497998363808));
#42712=CARTESIAN_POINT('Ctrl Pts',(-6.1623975114312,14.889311104208,3.11829760772158));
#42713=CARTESIAN_POINT('Ctrl Pts',(-6.16841114256548,14.8814366026319,3.08680088533039));
#42714=CARTESIAN_POINT('Ctrl Pts',(-6.17489884345628,14.8751254512654,3.05554519947911));
#42715=CARTESIAN_POINT('Ctrl Pts',(-6.18153496518978,14.8686699180261,3.02357446906709));
#42716=CARTESIAN_POINT('Ctrl Pts',(-6.1886667428536,14.8638495759053,2.99185656839097));
#42717=CARTESIAN_POINT('Ctrl Pts',(-6.19619836197334,14.8605615026144,2.96061010749823));
#42718=CARTESIAN_POINT('Ctrl Pts',(-6.20384154406425,14.8572247243612,2.92890080482331));
#42719=CARTESIAN_POINT('Ctrl Pts',(-6.21189614733935,14.8554652284595,2.89767739372793));
#42720=CARTESIAN_POINT('Ctrl Pts',(-6.22026195312469,14.8551414242366,2.86712645708341));
#42721=CARTESIAN_POINT('Ctrl Pts',(-6.2288284005593,14.8548098540417,2.83584280078556));
#42722=CARTESIAN_POINT('Ctrl Pts',(-6.23772083042933,14.8559828945091,2.80526447799116));
#42723=CARTESIAN_POINT('Ctrl Pts',(-6.24683682053218,14.8584845581957,2.77554348983372));
#42724=CARTESIAN_POINT('Ctrl Pts',(-6.24787035040546,14.8587681855498,2.77217385814505));
#42725=CARTESIAN_POINT('Ctrl Pts',(-6.24890676222108,14.8590688735896,2.76881519519068));
#42726=CARTESIAN_POINT('Ctrl Pts',(-6.24994591350264,14.8593863538791,2.76546768326257));
#42727=CARTESIAN_POINT('',(-7.00000135336451,14.5427413789166,3.16613017331584));
#42728=CARTESIAN_POINT('Ctrl Pts',(-7.00000153559549,14.542740500495,3.1661294352437));
#42729=CARTESIAN_POINT('Ctrl Pts',(-6.97364721274325,14.5565707108292,3.14316239933483));
#42730=CARTESIAN_POINT('Ctrl Pts',(-6.94679740601726,14.5702605952016,3.12104432197344));
#42731=CARTESIAN_POINT('Ctrl Pts',(-6.91946606855886,14.5838156764254,3.09975876986723));
#42732=CARTESIAN_POINT('Ctrl Pts',(-6.87663067475657,14.6050600536216,3.06639871172313));
#42733=CARTESIAN_POINT('Ctrl Pts',(-6.8326149259663,14.6259733629431,3.03508153386991));
#42734=CARTESIAN_POINT('Ctrl Pts',(-6.78747034343769,14.6465723854995,3.00575805068263));
#42735=CARTESIAN_POINT('Ctrl Pts',(-6.74232576090909,14.667171408056,2.97643456749534));
#42736=CARTESIAN_POINT('Ctrl Pts',(-6.6960516690935,14.6874563967845,2.94910431005622));
#42737=CARTESIAN_POINT('Ctrl Pts',(-6.6486547929194,14.7074421527635,2.9237597194014));
#42738=CARTESIAN_POINT('Ctrl Pts',(-6.6036789888132,14.7264070196151,2.89970975163018));
#42739=CARTESIAN_POINT('Ctrl Pts',(-6.55771201090129,14.7450958926099,2.87744892165356));
#42740=CARTESIAN_POINT('Ctrl Pts',(-6.51072378439587,14.7635200977768,2.85700612744214));
#42741=CARTESIAN_POINT('Ctrl Pts',(-6.5037844957592,14.7662410108025,2.85398710629316));
#42742=CARTESIAN_POINT('Ctrl Pts',(-6.4968228884971,14.7689561396818,2.8510078161327));
#42743=CARTESIAN_POINT('Ctrl Pts',(-6.48983882057931,14.7716655077748,2.84806843498458));
#42744=CARTESIAN_POINT('Ctrl Pts',(-6.44329065809342,14.7897231938838,2.82847773327587));
#42745=CARTESIAN_POINT('Ctrl Pts',(-6.39574608919368,14.8075257294178,2.81065598168833));
#42746=CARTESIAN_POINT('Ctrl Pts',(-6.34718915281274,14.8250699566923,2.79466001873052));
#42747=CARTESIAN_POINT('Ctrl Pts',(-6.31521652086591,14.8366220677448,2.78412737243107));
#42748=CARTESIAN_POINT('Ctrl Pts',(-6.28280457428078,14.8480620193034,2.77438725400823));
#42749=CARTESIAN_POINT('Ctrl Pts',(-6.24994591350294,14.859386353879,2.76546768326265));
#42750=CARTESIAN_POINT('',(-7.000010673752,14.7967990005536,4.92966193792747));
#42751=CARTESIAN_POINT('Ctrl Pts',(-7.000010673752,14.7967990005536,4.92966193792747));
#42752=CARTESIAN_POINT('Ctrl Pts',(-7.,14.7621679284434,4.84253808279512));
#42753=CARTESIAN_POINT('Ctrl Pts',(-7.,14.7150272228418,4.71628322423078));
#42754=CARTESIAN_POINT('Ctrl Pts',(-7.,14.675095371086,4.59667475186774));
#42755=CARTESIAN_POINT('Ctrl Pts',(-7.,14.6500761041033,4.51841274500377));
#42756=CARTESIAN_POINT('Ctrl Pts',(-7.,14.6389581414002,4.48205932201662));
#42757=CARTESIAN_POINT('Ctrl Pts',(-7.,14.5814663764124,4.28359371296804));
#42758=CARTESIAN_POINT('Ctrl Pts',(-7.,14.5473293834115,4.12815295854409));
#42759=CARTESIAN_POINT('Ctrl Pts',(-7.,14.4827650476056,3.68737356277082));
#42760=CARTESIAN_POINT('Ctrl Pts',(-7.,14.4884094371492,3.41567493764516));
#42761=CARTESIAN_POINT('Ctrl Pts',(-7.000002992025,14.5427411067738,3.16613061790934));
#42762=CARTESIAN_POINT('Ctrl Pts',(-7.00001531363849,14.7967990006772,4.92966193758492));
#42763=CARTESIAN_POINT('Ctrl Pts',(-7.00001196691825,14.8230711151817,4.89380607408238));
#42764=CARTESIAN_POINT('Ctrl Pts',(-6.99838322945502,14.8490064611586,4.85901685982402));
#42765=CARTESIAN_POINT('Ctrl Pts',(-6.99539548218125,14.8744859668073,4.82539406693647));
#42766=CARTESIAN_POINT('Ctrl Pts',(-6.99268063643135,14.8976381685438,4.79484238769247));
#42767=CARTESIAN_POINT('Ctrl Pts',(-6.98884285920536,14.9204144722212,4.76525326760272));
#42768=CARTESIAN_POINT('Ctrl Pts',(-6.98405836242474,14.9427429789628,4.73667880819996));
#42769=CARTESIAN_POINT('Ctrl Pts',(-6.97840508154729,14.9691259667611,4.70291570785058));
#42770=CARTESIAN_POINT('Ctrl Pts',(-6.97143143614919,14.9948834812303,4.6705691487042));
#42771=CARTESIAN_POINT('Ctrl Pts',(-6.96343343703202,15.0199262617575,4.63966369249073));
#42772=CARTESIAN_POINT('Ctrl Pts',(-6.95719888415003,15.0394474616503,4.61557245438453));
#42773=CARTESIAN_POINT('Ctrl Pts',(-6.95034087929794,15.0585349151722,4.5923562821223));
#42774=CARTESIAN_POINT('Ctrl Pts',(-6.94298351534871,15.0771558467909,4.57001569283416));
#42775=CARTESIAN_POINT('Ctrl Pts',(-6.93534008828234,15.0965007825202,4.5468064746927));
#42776=CARTESIAN_POINT('Ctrl Pts',(-6.9271576586673,15.1153422373258,4.52454227767355));
#42777=CARTESIAN_POINT('Ctrl Pts',(-6.91856206152671,15.1336516857214,4.50321362637874));
#42778=CARTESIAN_POINT('Ctrl Pts',(-6.9082791173002,15.1555553456522,4.47769808300178));
#42779=CARTESIAN_POINT('Ctrl Pts',(-6.89740589527407,15.1766974510516,4.4535212602693));
#42780=CARTESIAN_POINT('Ctrl Pts',(-6.88615352910444,15.1970443255629,4.43063595944498));
#42781=CARTESIAN_POINT('Ctrl Pts',(-6.87582437358577,15.215721822187,4.40962830401121));
#42782=CARTESIAN_POINT('Ctrl Pts',(-6.86517521076683,15.2337294687443,4.3897087262134));
#42783=CARTESIAN_POINT('Ctrl Pts',(-6.85434931457902,15.2510499793023,4.37083284180152));
#42784=CARTESIAN_POINT('Ctrl Pts',(-6.84893636648512,15.2597102345813,4.36139489959558));
#42785=CARTESIAN_POINT('Ctrl Pts',(-6.84347895561017,15.2681988269856,4.35221777101534));
#42786=CARTESIAN_POINT('Ctrl Pts',(-6.83799341138776,15.2765142688728,4.34329529706221));
#42787=CARTESIAN_POINT('Ctrl Pts',(-6.83525063927656,15.2806719898164,4.33883406008565));
#42788=CARTESIAN_POINT('Ctrl Pts',(-6.83250082545977,15.2847864234481,4.33443649226567));
#42789=CARTESIAN_POINT('Ctrl Pts',(-6.82974591181241,15.2888574285857,4.33010177679098));
#42790=CARTESIAN_POINT('Ctrl Pts',(-6.82836845498873,15.2908929311545,4.32793441905364));
#42791=CARTESIAN_POINT('Ctrl Pts',(-6.82698972268906,15.2929175766191,4.32578277473141));
#42792=CARTESIAN_POINT('Ctrl Pts',(-6.82560995332809,15.2949313485221,4.32364674161949));
#42793=CARTESIAN_POINT('Ctrl Pts',(-6.82452960127801,15.2965081211809,4.32197423908626));
#42794=CARTESIAN_POINT('Ctrl Pts',(-6.82391451566205,15.2974032632247,4.32102605564055));
#42795=CARTESIAN_POINT('Ctrl Pts',(-6.82267100370107,15.2992022745916,4.31912276492142));
#42796=CARTESIAN_POINT('Ctrl Pts',(-6.82232636696216,15.299700866829,4.31859527187976));
#42797=CARTESIAN_POINT('Ctrl Pts',(-6.82193326309863,15.3002688772549,4.3179945640952));
#42798=CARTESIAN_POINT('Ctrl Pts',(-6.82146776975955,15.3009400278368,4.31728537373772));
#42799=CARTESIAN_POINT('Ctrl Pts',(-6.81268226478646,15.3136070120445,4.30390044448221));
#42800=CARTESIAN_POINT('Ctrl Pts',(-6.80362640832164,15.3261903141844,4.29077930911651));
#42801=CARTESIAN_POINT('Ctrl Pts',(-6.79431173496066,15.338683927426,4.27793151564932));
#42802=CARTESIAN_POINT('Ctrl Pts',(-6.76482331619401,15.3782362428857,4.23725793544894));
#42803=CARTESIAN_POINT('Ctrl Pts',(-6.73274514991914,15.4168880037098,4.19932321819618));
#42804=CARTESIAN_POINT('Ctrl Pts',(-6.69853334234179,15.4544725960513,4.16431783527236));
#42805=CARTESIAN_POINT('Ctrl Pts',(-6.67146117751713,15.4842136810974,4.13661770589096));
#42806=CARTESIAN_POINT('Ctrl Pts',(-6.64305164022627,15.5132870161513,4.11075217063323));
#42807=CARTESIAN_POINT('Ctrl Pts',(-6.61350997411101,15.5416193773585,4.08681697858153));
#42808=CARTESIAN_POINT('Ctrl Pts',(-6.57430874914484,15.57921587788,4.05505543728706));
#42809=CARTESIAN_POINT('Ctrl Pts',(-6.533116155595,15.615507019943,4.02669216937345));
#42810=CARTESIAN_POINT('Ctrl Pts',(-6.49047955248457,15.6503524602336,4.00181647924621));
#42811=CARTESIAN_POINT('Ctrl Pts',(-6.45748266623747,15.6773196889905,3.98256493813914));
#42812=CARTESIAN_POINT('Ctrl Pts',(-6.42361968093473,15.7034214727792,3.96540262136043));
#42813=CARTESIAN_POINT('Ctrl Pts',(-6.38912480969674,15.7286009735068,3.95037176693883));
#42814=CARTESIAN_POINT('Ctrl Pts',(-6.34811700052793,15.7585345875121,3.93250295376041));
#42815=CARTESIAN_POINT('Ctrl Pts',(-6.30621724569481,15.7871646914559,3.91764573687081));
#42816=CARTESIAN_POINT('Ctrl Pts',(-6.26385533697638,15.8144219674758,3.90575676779332));
#42817=CARTESIAN_POINT('Ctrl Pts',(-6.22266866665511,14.5714076353156,3.97375061095509));
#42818=CARTESIAN_POINT('Ctrl Pts',(-6.22400419724087,14.9771431331047,3.92718914139647));
#42819=CARTESIAN_POINT('Ctrl Pts',(-6.22726378222481,16.0460292266971,3.85976019567651));
#42820=CARTESIAN_POINT('Ctrl Pts',(-6.23205231075792,17.7794228547352,3.98190952387196));
#42821=CARTESIAN_POINT('Ctrl Pts',(-6.23570613836487,19.7179580001375,4.44990387151557));
#42822=CARTESIAN_POINT('Ctrl Pts',(-6.23759530667989,21.5545938411779,5.23225344908634));
#42823=CARTESIAN_POINT('Ctrl Pts',(-6.23804249999508,23.235159518522,6.30682982345941));
#42824=CARTESIAN_POINT('Ctrl Pts',(-6.23649564902418,24.5993878927371,7.54006348689315));
#42825=CARTESIAN_POINT('Ctrl Pts',(-6.2349078630626,25.3447858427874,8.4442579151259));
#42826=CARTESIAN_POINT('Ctrl Pts',(-6.23413257076684,25.6421045126576,8.85534255591597));
#42827=CARTESIAN_POINT('Ctrl Pts',(-6.71589047216739,14.5843361710878,4.08565974143756));
#42828=CARTESIAN_POINT('Ctrl Pts',(-6.71707918947188,14.9863176706671,4.04021329281028));
#42829=CARTESIAN_POINT('Ctrl Pts',(-6.7199337157726,16.0451894970697,3.9750781528678));
#42830=CARTESIAN_POINT('Ctrl Pts',(-6.72416456955626,17.7615686381462,4.09849148251139));
#42831=CARTESIAN_POINT('Ctrl Pts',(-6.72736824236877,19.6804267269655,4.56367690614212));
#42832=CARTESIAN_POINT('Ctrl Pts',(-6.7290242968866,21.4982088429253,5.33903867080659));
#42833=CARTESIAN_POINT('Ctrl Pts',(-6.7294192912941,23.1617872950511,6.40303091018955));
#42834=CARTESIAN_POINT('Ctrl Pts',(-6.72805175754339,24.5127355742067,7.62318968102802));
#42835=CARTESIAN_POINT('Ctrl Pts',(-6.72668348409556,25.25139899912,8.51793670641239));
#42836=CARTESIAN_POINT('Ctrl Pts',(-6.72599033859008,25.546099410539,8.92472526281053));
#42837=CARTESIAN_POINT('Ctrl Pts',(-7.02184867857606,14.6305390034327,4.4855963187998));
#42838=CARTESIAN_POINT('Ctrl Pts',(-7.02249163139255,15.0188751615543,4.4421515223094));
#42839=CARTESIAN_POINT('Ctrl Pts',(-7.02397829285082,16.041918560353,4.38032091134352));
#42840=CARTESIAN_POINT('Ctrl Pts',(-7.02622833236719,17.6995247916472,4.5011327717638));
#42841=CARTESIAN_POINT('Ctrl Pts',(-7.02790168554062,19.5522386343259,4.95159427705417));
#42842=CARTESIAN_POINT('Ctrl Pts',(-7.0287662253155,21.3070968346045,5.70076931983152));
#42843=CARTESIAN_POINT('Ctrl Pts',(-7.02897614364903,22.9136327574069,6.72847832494041));
#42844=CARTESIAN_POINT('Ctrl Pts',(-7.02824784119134,24.2181471728286,7.90599723975289));
#42845=CARTESIAN_POINT('Ctrl Pts',(-7.0275628969235,24.9320746794641,8.76993207383052));
#42846=CARTESIAN_POINT('Ctrl Pts',(-7.02718421281456,25.216900126262,9.16263740321616));
#42847=CARTESIAN_POINT('Ctrl Pts',(-6.99898915447974,14.6884801945479,4.98714299553211));
#42848=CARTESIAN_POINT('Ctrl Pts',(-6.99894179717708,15.0596401640139,4.94565491848551));
#42849=CARTESIAN_POINT('Ctrl Pts',(-6.99873531515279,16.0377412527625,4.88660281634937));
#42850=CARTESIAN_POINT('Ctrl Pts',(-6.99850468378134,17.6222097431878,5.00216549828158));
#42851=CARTESIAN_POINT('Ctrl Pts',(-6.99828080391387,19.3931400914782,5.43285456754646));
#42852=CARTESIAN_POINT('Ctrl Pts',(-6.99816433649053,21.0703308732033,6.14885094481258));
#42853=CARTESIAN_POINT('Ctrl Pts',(-6.99814256766934,22.6063548077465,7.13148873843438));
#42854=CARTESIAN_POINT('Ctrl Pts',(-6.99821545499553,23.8529244713798,8.25667503834028));
#42855=CARTESIAN_POINT('Ctrl Pts',(-6.99835921852923,24.5356449909404,9.08279284373535));
#42856=CARTESIAN_POINT('Ctrl Pts',(-6.99838071935911,24.8079420348425,9.45819131628623));
#42857=CARTESIAN_POINT('',(-7.00000355772625,24.7867164860195,9.33251602987461));
#42858=CARTESIAN_POINT('Ctrl Pts',(-7.00001601631107,14.7967990005468,4.92966193771618));
#42859=CARTESIAN_POINT('Ctrl Pts',(-7.00002088955923,15.0161850300475,4.90663940958755));
#42860=CARTESIAN_POINT('Ctrl Pts',(-7.00001598262228,15.234292636829,4.89043247358986));
#42861=CARTESIAN_POINT('Ctrl Pts',(-7.00000988116101,15.4506299520445,4.88069443524321));
#42862=CARTESIAN_POINT('Ctrl Pts',(-7.00000652438984,15.5696497787099,4.87533697005084));
#42863=CARTESIAN_POINT('Ctrl Pts',(-7.0000027908345,15.6881347163888,4.87193754799028));
#42864=CARTESIAN_POINT('Ctrl Pts',(-6.99999999965563,15.8060095355692,4.87043898594988));
#42865=CARTESIAN_POINT('Ctrl Pts',(-6.99999455429069,16.0359738046019,4.86751541222465));
#42866=CARTESIAN_POINT('Ctrl Pts',(-6.99999266088648,16.2636130581478,4.87182596258862));
#42867=CARTESIAN_POINT('Ctrl Pts',(-6.99999257352081,16.4885162719136,4.88291846826979));
#42868=CARTESIAN_POINT('Ctrl Pts',(-6.99999248489009,16.7166760665194,4.89417159256048));
#42869=CARTESIAN_POINT('Ctrl Pts',(-6.99999425322404,16.9420200637692,4.91240447412795));
#42870=CARTESIAN_POINT('Ctrl Pts',(-6.99999619758454,17.1641720473477,4.9371555976089));
#42871=CARTESIAN_POINT('Ctrl Pts',(-6.99999754424877,17.3180345277597,4.95429822757969));
#42872=CARTESIAN_POINT('Ctrl Pts',(-6.99999897835572,17.4703669255095,4.97456784638868));
#42873=CARTESIAN_POINT('Ctrl Pts',(-6.99999998662298,17.6210585491081,4.99781411503021));
#42874=CARTESIAN_POINT('Ctrl Pts',(-7.00000143707717,17.8378376785165,5.03125529615071));
#42875=CARTESIAN_POINT('Ctrl Pts',(-7.00000201440455,18.0512192734557,5.07085505278939));
#42876=CARTESIAN_POINT('Ctrl Pts',(-7.00000210874309,18.2609089454417,5.11608568204281));
#42877=CARTESIAN_POINT('Ctrl Pts',(-7.00000220459579,18.4739641816515,5.1620422725999));
#42878=CARTESIAN_POINT('Ctrl Pts',(-7.00000180216121,18.6832080881582,5.21381192541017));
#42879=CARTESIAN_POINT('Ctrl Pts',(-7.00000129011671,18.8883807481865,5.27086478685517));
#42880=CARTESIAN_POINT('Ctrl Pts',(-7.00000086166942,19.06005658805,5.31860310590722));
#42881=CARTESIAN_POINT('Ctrl Pts',(-7.0000003561918,19.2288829378954,5.37004079520996));
#42882=CARTESIAN_POINT('Ctrl Pts',(-6.99999998816664,19.3947325989926,5.42487991583199));
#42883=CARTESIAN_POINT('Ctrl Pts',(-6.99999970373584,19.522910661253,5.46726271101465));
#42884=CARTESIAN_POINT('Ctrl Pts',(-6.99999950020159,19.6493112372598,5.51167738494756));
#42885=CARTESIAN_POINT('Ctrl Pts',(-6.99999936067768,19.77389027009,5.55798424211543));
#42886=CARTESIAN_POINT('Ctrl Pts',(-6.99999924479276,19.8773623632287,5.5964455090637));
#42887=CARTESIAN_POINT('Ctrl Pts',(-6.99999917321856,19.9795779919129,5.63621218780983));
#42888=CARTESIAN_POINT('Ctrl Pts',(-6.99999913936882,20.0805155479599,5.67720660818328));
#42889=CARTESIAN_POINT('Ctrl Pts',(-6.99999912244395,20.1309843259834,5.69770381837001));
#42890=CARTESIAN_POINT('Ctrl Pts',(-6.99999911499155,20.1811335858475,5.71850796396357));
#42891=CARTESIAN_POINT('Ctrl Pts',(-6.99999911640457,20.230960984313,5.7396095727455));
#42892=CARTESIAN_POINT('Ctrl Pts',(-6.99999911711109,20.2558746835458,5.75016037713646));
#42893=CARTESIAN_POINT('Ctrl Pts',(-6.99999912003616,20.2807079174289,5.76078554732452));
#42894=CARTESIAN_POINT('Ctrl Pts',(-6.99999912511612,20.3054604023376,5.77148390561387));
#42895=CARTESIAN_POINT('Ctrl Pts',(-6.9999991276561,20.3178366447919,5.77683308475855));
#42896=CARTESIAN_POINT('Ctrl Pts',(-6.99999913073492,20.3301927000026,5.78220056092855));
#42897=CARTESIAN_POINT('Ctrl Pts',(-6.99999913434533,20.3425285337603,5.78758618774242));
#42898=CARTESIAN_POINT('Ctrl Pts',(-6.99999913750155,20.3533125335665,5.792294308787));
#42899=CARTESIAN_POINT('Ctrl Pts',(-6.99999914057199,20.3627040147974,5.79641054922249));
#42900=CARTESIAN_POINT('Ctrl Pts',(-6.99999914483718,20.3743145448473,5.80152324163118));
#42901=CARTESIAN_POINT('Ctrl Pts',(-6.99999914545094,20.3759853177563,5.80225896583424));
#42902=CARTESIAN_POINT('Ctrl Pts',(-6.99999914609139,20.3777020071407,5.80301540343862));
#42903=CARTESIAN_POINT('Ctrl Pts',(-6.99999914676447,20.3794753368333,5.80379737398191));
#42904=CARTESIAN_POINT('Ctrl Pts',(-6.99999923697432,20.6171488623564,5.90860230487248));
#42905=CARTESIAN_POINT('Ctrl Pts',(-6.9999995214451,20.8492787949593,6.02101278100693));
#42906=CARTESIAN_POINT('Ctrl Pts',(-6.99999999018436,21.0754662943573,6.14041872107596));
#42907=CARTESIAN_POINT('Ctrl Pts',(-7.00000044364517,21.2942812687163,6.25593265435725));
#42908=CARTESIAN_POINT('Ctrl Pts',(-7.00000106797362,21.5075354204105,6.37799275859144));
#42909=CARTESIAN_POINT('Ctrl Pts',(-7.0000014259355,21.7149354690259,6.50595994064156));
#42910=CARTESIAN_POINT('Ctrl Pts',(-7.00000178766081,21.9245160164487,6.6352725046707));
#42911=CARTESIAN_POINT('Ctrl Pts',(-7.00000187627579,22.128118760899,6.7706170178974));
#42912=CARTESIAN_POINT('Ctrl Pts',(-7.00000131558895,22.3254829787871,6.91136700483684));
#42913=CARTESIAN_POINT('Ctrl Pts',(-7.00000103872953,22.4229387019167,6.98086740315849));
#42914=CARTESIAN_POINT('Ctrl Pts',(-7.00000060480684,22.5188739540238,7.0516862930617));
#42915=CARTESIAN_POINT('Ctrl Pts',(-6.99999997635786,22.6132610013232,7.12375115262203));
#42916=CARTESIAN_POINT('Ctrl Pts',(-6.99999887928546,22.7780308196262,7.24955351804758));
#42917=CARTESIAN_POINT('Ctrl Pts',(-6.99999719588015,22.9380818114236,7.37915178801838));
#42918=CARTESIAN_POINT('Ctrl Pts',(-6.99999590265512,23.0933374636584,7.51215857756211));
#42919=CARTESIAN_POINT('Ctrl Pts',(-6.99999568173278,23.11985987192,7.53488020040196));
#42920=CARTESIAN_POINT('Ctrl Pts',(-6.99999546003951,23.147696016291,7.55895210223158));
#42921=CARTESIAN_POINT('Ctrl Pts',(-6.99999525390297,23.1758122701074,7.58352676073225));
#42922=CARTESIAN_POINT('Ctrl Pts',(-6.9999951203152,23.194033142726,7.59945248558547));
#42923=CARTESIAN_POINT('Ctrl Pts',(-6.9999949932545,23.2123722852666,7.61558859099952));
#42924=CARTESIAN_POINT('Ctrl Pts',(-6.99999487632491,23.230556080559,7.63169544081873));
#42925=CARTESIAN_POINT('Ctrl Pts',(-6.99999457896369,23.2767989164085,7.67265643934869));
#42926=CARTESIAN_POINT('Ctrl Pts',(-6.99999434329156,23.3225495030913,7.71387570898918));
#42927=CARTESIAN_POINT('Ctrl Pts',(-6.99999419421933,23.3678080626012,7.75533994626581));
#42928=CARTESIAN_POINT('Ctrl Pts',(-6.99999365475981,23.5315888152958,7.9053898829985));
#42929=CARTESIAN_POINT('Ctrl Pts',(-6.99999426200986,23.6889267660997,8.05864857927771));
#42930=CARTESIAN_POINT('Ctrl Pts',(-6.99999708873464,23.8398716778354,8.21453805486139));
#42931=CARTESIAN_POINT('Ctrl Pts',(-6.99999738651599,23.8557729713616,8.23096023352509));
#42932=CARTESIAN_POINT('Ctrl Pts',(-6.99999770877531,23.8716033460782,8.24741164560196));
#42933=CARTESIAN_POINT('Ctrl Pts',(-6.99999805665875,23.8873628800275,8.26389164217577));
#42934=CARTESIAN_POINT('Ctrl Pts',(-6.99999863110266,23.9133858732566,8.29110430218429));
#42935=CARTESIAN_POINT('Ctrl Pts',(-6.99999927542236,23.939215707693,8.31839489993074));
#42936=CARTESIAN_POINT('Ctrl Pts',(-6.99999999465542,23.96485275711,8.34576054451061));
#42937=CARTESIAN_POINT('Ctrl Pts',(-7.0000039334845,24.1052522486671,8.49562656546484));
#42938=CARTESIAN_POINT('Ctrl Pts',(-7.00001006472447,24.2398678374837,8.64773959093446));
#42939=CARTESIAN_POINT('Ctrl Pts',(-7.00001375742669,24.3687624704118,8.80155051150861));
#42940=CARTESIAN_POINT('Ctrl Pts',(-7.00001750461739,24.4995590368591,8.95763102344457));
#42941=CARTESIAN_POINT('Ctrl Pts',(-7.0000187420762,24.624464636053,9.11545995264843));
#42942=CARTESIAN_POINT('Ctrl Pts',(-7.00001328590555,24.7435704048451,9.27451056188657));
#42943=CARTESIAN_POINT('Ctrl Pts',(-7.00001262320432,24.7580368766487,9.29382869548516));
#42944=CARTESIAN_POINT('Ctrl Pts',(-7.00001186252464,24.7724178171665,9.31316490733289));
#42945=CARTESIAN_POINT('Ctrl Pts',(-7.00001099700064,24.7867134139178,9.33251829944914));
#42946=CARTESIAN_POINT('',(-6.271594443024,25.5608538793675,8.76071211955143));
#42947=CARTESIAN_POINT('Origin',(-5.9999836234388,24.786713751936,9.3325281284206));
#42948=CARTESIAN_POINT('Ctrl Pts',(-6.26386059990525,15.8144217561051,3.90573753015588));
#42949=CARTESIAN_POINT('Ctrl Pts',(-6.26455152016216,16.0555038764713,3.90327937513647));
#42950=CARTESIAN_POINT('Ctrl Pts',(-6.26520985635303,16.2942788050406,3.90810430739374));
#42951=CARTESIAN_POINT('Ctrl Pts',(-6.26583560901963,16.530319704722,3.91978341537098));
#42952=CARTESIAN_POINT('Ctrl Pts',(-6.26647066279415,16.7698690862652,3.9316361201213));
#42953=CARTESIAN_POINT('Ctrl Pts',(-6.26707215721086,17.0066026034232,3.95054824892746));
#42954=CARTESIAN_POINT('Ctrl Pts',(-6.26764009283606,17.2401276173167,3.97607977054762));
#42955=CARTESIAN_POINT('Ctrl Pts',(-6.26812468264228,17.4393823148746,3.99786448445814));
#42956=CARTESIAN_POINT('Ctrl Pts',(-6.2685848405825,17.6363020702729,4.02446846271191));
#42957=CARTESIAN_POINT('Ctrl Pts',(-6.2690205670085,17.8306725455159,4.05562321069526));
#42958=CARTESIAN_POINT('Ctrl Pts',(-6.26953467303182,18.0600068849417,4.09238215538481));
#42959=CARTESIAN_POINT('Ctrl Pts',(-6.27001476738415,18.285791451733,4.13547485945373));
#42960=CARTESIAN_POINT('Ctrl Pts',(-6.27046085064331,18.5077359124598,4.1843574442804));
#42961=CARTESIAN_POINT('Ctrl Pts',(-6.27062083311881,18.5873336636003,4.20188860414532));
#42962=CARTESIAN_POINT('Ctrl Pts',(-6.27077644104249,18.6664379326915,4.22016468855067));
#42963=CARTESIAN_POINT('Ctrl Pts',(-6.27092767444099,18.7450367717596,4.23916134866817));
#42964=CARTESIAN_POINT('Ctrl Pts',(-6.27136815468887,18.9739626337642,4.29449075103807));
#42965=CARTESIAN_POINT('Ctrl Pts',(-6.27177152427923,19.1985970272609,4.35593090616152));
#42966=CARTESIAN_POINT('Ctrl Pts',(-6.27213778321205,19.4186800525206,4.42289861655494));
#42967=CARTESIAN_POINT('Ctrl Pts',(-6.27250404214487,19.6387630777802,4.48986632694836));
#42968=CARTESIAN_POINT('Ctrl Pts',(-6.27283319042016,19.8542949414132,4.56236165257248));
#42969=CARTESIAN_POINT('Ctrl Pts',(-6.27312522803792,20.0650658349331,4.63982809189077));
#42970=CARTESIAN_POINT('Ctrl Pts',(-6.27334042116275,20.2203761252606,4.69691061870571));
#42971=CARTESIAN_POINT('Ctrl Pts',(-6.27353526359634,20.3728239686049,4.75658573628156));
#42972=CARTESIAN_POINT('Ctrl Pts',(-6.27370997702005,20.5226551340267,4.81874475540076));
#42973=CARTESIAN_POINT('Ctrl Pts',(-6.27388469044377,20.6724862994485,4.88090377451995));
#42974=CARTESIAN_POINT('Ctrl Pts',(-6.27403927485761,20.819701119167,4.94554696496691));
#42975=CARTESIAN_POINT('Ctrl Pts',(-6.27417395194295,20.9645377628287,5.01262254882458));
#42976=CARTESIAN_POINT('Ctrl Pts',(-6.27427013710073,21.0679787853766,5.06052732490076));
#42977=CARTESIAN_POINT('Ctrl Pts',(-6.2743561681526,21.1702066478841,5.1096739270377));
#42978=CARTESIAN_POINT('Ctrl Pts',(-6.27443212585409,21.2713094630014,5.16004914532015));
#42979=CARTESIAN_POINT('Ctrl Pts',(-6.27457884491625,21.4665985505298,5.25735336381305));
#42980=CARTESIAN_POINT('Ctrl Pts',(-6.27469165472654,21.6616525046637,5.36122061383588));
#42981=CARTESIAN_POINT('Ctrl Pts',(-6.27477055528495,21.8559695030929,5.47186397511221));
#42982=CARTESIAN_POINT('Ctrl Pts',(-6.27484862841344,22.0482486997179,5.58134701977672));
#42983=CARTESIAN_POINT('Ctrl Pts',(-6.27489349977326,22.2398063968557,5.6974648751496));
#42984=CARTESIAN_POINT('Ctrl Pts',(-6.27490516936443,22.4301093886222,5.82040615118908));
#42985=CARTESIAN_POINT('Ctrl Pts',(-6.27491664536542,22.6172553899414,5.94130791943928));
#42986=CARTESIAN_POINT('Ctrl Pts',(-6.27489601204765,22.8031879940715,6.06880864561297));
#42987=CARTESIAN_POINT('Ctrl Pts',(-6.27484326941112,22.987353699931,6.20306946046052));
#42988=CARTESIAN_POINT('Ctrl Pts',(-6.27479056684953,23.171379472867,6.33722826115602));
#42989=CARTESIAN_POINT('Ctrl Pts',(-6.27470580374529,23.3536411785372,6.47813698009458));
#42990=CARTESIAN_POINT('Ctrl Pts',(-6.27458898009839,23.5335384062425,6.6259368247621));
#42991=CARTESIAN_POINT('Ctrl Pts',(-6.27454781389771,23.5969304126883,6.67801838724844));
#42992=CARTESIAN_POINT('Ctrl Pts',(-6.27450266675486,23.6600283703807,6.73095544150738));
#42993=CARTESIAN_POINT('Ctrl Pts',(-6.27445353865773,23.7228045290992,6.78475355170387));
#42994=CARTESIAN_POINT('Ctrl Pts',(-6.27431624105701,23.8982441751895,6.9351023721139));
#42995=CARTESIAN_POINT('Ctrl Pts',(-6.27414785113122,24.0711732188781,7.09217876505726));
#42996=CARTESIAN_POINT('Ctrl Pts',(-6.2739483686162,24.2410354064908,7.25599610010402));
#42997=CARTESIAN_POINT('Ctrl Pts',(-6.27375072715775,24.4093299083587,7.41830153833311));
#42998=CARTESIAN_POINT('Ctrl Pts',(-6.27352256437881,24.5746139498349,7.58722414933204));
#42999=CARTESIAN_POINT('Ctrl Pts',(-6.27326388002248,24.7363078687583,7.76274427820177));
#43000=CARTESIAN_POINT('Ctrl Pts',(-6.27300884363477,24.8957215788977,7.93578922097746));
#43001=CARTESIAN_POINT('Ctrl Pts',(-6.27272414043095,25.0516457201638,8.11524696640679));
#43002=CARTESIAN_POINT('Ctrl Pts',(-6.27240977016483,25.2034866584683,8.30106585433031));
#43003=CARTESIAN_POINT('Ctrl Pts',(-6.27215746702584,25.3253491546767,8.45019792488959));
#43004=CARTESIAN_POINT('Ctrl Pts',(-6.27188605493237,25.4445809018636,8.60342669609818));
#43005=CARTESIAN_POINT('Ctrl Pts',(-6.27159553375718,25.5608567073971,8.76070944735613));
#43006=CARTESIAN_POINT('Origin',(-5.999994993362,24.7867196013936,9.33250915082854));
#43007=CARTESIAN_POINT('',(-5.988522466616,25.7188096067786,9.69456809159626));
#43008=CARTESIAN_POINT('Origin',(-5.999994993362,24.7867196013936,9.33250915082854));
#43009=CARTESIAN_POINT('Origin',(-6.,24.7867243682982,9.33251101023601));
#43010=CARTESIAN_POINT('Ctrl Pts',(-5.9884183314302,25.7189877484754,9.69410640762213));
#43011=CARTESIAN_POINT('Ctrl Pts',(-5.98810627261414,25.6713270178884,9.81679904137616));
#43012=CARTESIAN_POINT('Ctrl Pts',(-5.98726405067268,25.5029619480015,10.2439466058636));
#43013=CARTESIAN_POINT('Ctrl Pts',(-5.98726405067174,25.2768814416824,10.7897532303017));
#43014=CARTESIAN_POINT('Ctrl Pts',(-5.98810627263415,25.093894583665,11.2108442548557));
#43015=CARTESIAN_POINT('Ctrl Pts',(-5.98841833146804,25.0408390141729,11.331302278264));
#43016=CARTESIAN_POINT('Ctrl Pts',(-6.58019637231563,25.7253769308084,9.69658812202776));
#43017=CARTESIAN_POINT('Ctrl Pts',(-6.57988216494696,25.6778801590244,9.81936871653832));
#43018=CARTESIAN_POINT('Ctrl Pts',(-6.57903377367882,25.5099484810601,10.2467760957568));
#43019=CARTESIAN_POINT('Ctrl Pts',(-6.57903377367798,25.283822418076,10.7926927037156));
#43020=CARTESIAN_POINT('Ctrl Pts',(-6.57988216496595,25.1003453889219,11.213660990656));
#43021=CARTESIAN_POINT('Ctrl Pts',(-6.58019637235286,25.047111685395,11.3340652753282));
#43022=CARTESIAN_POINT('Ctrl Pts',(-7.0007967699024,25.3372908820844,9.54584601718842));
#43023=CARTESIAN_POINT('Ctrl Pts',(-7.00061248525782,25.2904141391226,9.6673928911595));
#43024=CARTESIAN_POINT('Ctrl Pts',(-7.00011448478284,25.1245686183319,10.0904742410697));
#43025=CARTESIAN_POINT('Ctrl Pts',(-7.0001144847828,24.90079560249,10.6307100907232));
#43026=CARTESIAN_POINT('Ctrl Pts',(-7.00061248526902,24.7189024021122,11.0471442770885));
#43027=CARTESIAN_POINT('Ctrl Pts',(-7.00079676992375,24.6661026441675,11.1662377629661));
#43028=CARTESIAN_POINT('Ctrl Pts',(-6.99999917319424,24.7856430606076,9.33157252305582));
#43029=CARTESIAN_POINT('Ctrl Pts',(-6.99999957777252,24.7394735071848,9.45129807054518));
#43030=CARTESIAN_POINT('Ctrl Pts',(-7.00000004362271,24.576125663887,9.86804157212209));
#43031=CARTESIAN_POINT('Ctrl Pts',(-7.00000004362353,24.3557042217843,10.4001860069831));
#43032=CARTESIAN_POINT('Ctrl Pts',(-6.99999957777277,24.1765264322708,10.8103725330858));
#43033=CARTESIAN_POINT('Ctrl Pts',(-6.99999917319347,24.124514488149,10.9276780880777));
#43034=CARTESIAN_POINT('Origin',(-5.98852353411271,-11.4730434368695,-4.75229019548653));
#43035=CARTESIAN_POINT('Origin',(-7.00021006967891,-11.450461588713,-4.74293652086132));
#43036=CARTESIAN_POINT('Ctrl Pts',(-6.05501399426344,25.843213493296,9.37211836695523));
#43037=CARTESIAN_POINT('Ctrl Pts',(-4.03667599617529,26.0304542939164,8.81551147064258));
#43038=CARTESIAN_POINT('Ctrl Pts',(7.59696559070322E-7,26.2482747367075,
8.27054054754906));
#43039=CARTESIAN_POINT('Ctrl Pts',(4.03667751556894,26.030454211933,8.81551167576954));
#43040=CARTESIAN_POINT('Ctrl Pts',(6.05501627335339,25.8432132818694,9.37211899547316));
#43041=CARTESIAN_POINT('Ctrl Pts',(-6.05501399426344,25.5527964585656,10.139984230889));
#43042=CARTESIAN_POINT('Ctrl Pts',(-4.03667599617529,25.6069283663818,9.95057478849123));
#43043=CARTESIAN_POINT('Ctrl Pts',(7.59696559070322E-7,25.7965044905289,
9.81338314348819));
#43044=CARTESIAN_POINT('Ctrl Pts',(4.03667751556894,25.6069282950242,9.95057484012904));
#43045=CARTESIAN_POINT('Ctrl Pts',(6.05501627335339,25.5527963974361,10.1399844447668));
#43046=CARTESIAN_POINT('Ctrl Pts',(-6.05501399426344,25.238357418666,10.8990899687285));
#43047=CARTESIAN_POINT('Ctrl Pts',(-4.03667599617529,25.1425814619013,11.0715782717953));
#43048=CARTESIAN_POINT('Ctrl Pts',(7.59696559951561E-7,25.1794745731306,
11.3029082164588));
#43049=CARTESIAN_POINT('Ctrl Pts',(4.03667751556894,25.1425814480204,11.0715781847256));
#43050=CARTESIAN_POINT('Ctrl Pts',(6.05501627335339,25.2383575268156,10.8990897739563));
#43051=CARTESIAN_POINT('Ctrl Pts',(-6.05501399426344,24.9007381290703,11.6474034030455));
#43052=CARTESIAN_POINT('Ctrl Pts',(-4.03667599617529,24.639428484335,12.17365751233));
#43053=CARTESIAN_POINT('Ctrl Pts',(7.59696559951561E-7,24.4078900068987,
12.7132715562852));
#43054=CARTESIAN_POINT('Ctrl Pts',(4.03667751556894,24.6394285714926,12.1736573092234));
#43055=CARTESIAN_POINT('Ctrl Pts',(6.05501627335339,24.9007384241377,11.647402808804));
#43056=CARTESIAN_POINT('Ctrl Pts',(-5.98852262876833,25.7188097475182,9.69456765113316));
#43057=CARTESIAN_POINT('Ctrl Pts',(-5.94974655199935,25.7233178563395,9.68173306451428));
#43058=CARTESIAN_POINT('Ctrl Pts',(-5.90268839887375,25.7287701868352,9.66624531862473));
#43059=CARTESIAN_POINT('Ctrl Pts',(-5.84725019936459,25.7351158736154,9.64828911090958));
#43060=CARTESIAN_POINT('Ctrl Pts',(-5.7979319987961,25.7407610398751,9.63231514600116));
#43061=CARTESIAN_POINT('Ctrl Pts',(-5.74198182700145,25.7471137839668,9.61438660928848));
#43062=CARTESIAN_POINT('Ctrl Pts',(-5.67933070964221,25.7541280730545,9.59466621125991));
#43063=CARTESIAN_POINT('Ctrl Pts',(-5.62086563255419,25.7606737017603,9.57626343347167));
#43064=CARTESIAN_POINT('Ctrl Pts',(-5.55656514377058,25.7677957313199,9.55629965427607));
#43065=CARTESIAN_POINT('Ctrl Pts',(-5.48637319134976,25.7754414992881,9.53494806705986));
#43066=CARTESIAN_POINT('Ctrl Pts',(-5.42062866343296,25.782602824601,9.51494933539061));
#43067=CARTESIAN_POINT('Ctrl Pts',(-5.34971559674257,25.7902237362974,9.49373286447064));
#43068=CARTESIAN_POINT('Ctrl Pts',(-5.27358793301862,25.7982443243501,9.47148357427303));
#43069=CARTESIAN_POINT('Ctrl Pts',(-5.23094196658891,25.8027373786763,9.45901974133193));
#43070=CARTESIAN_POINT('Ctrl Pts',(-5.18665959187008,25.8073555411599,9.44623259643214));
#43071=CARTESIAN_POINT('Ctrl Pts',(-5.14073271205297,25.8120856159465,9.43316140505069));
#43072=CARTESIAN_POINT('Ctrl Pts',(-5.08889805695584,25.8174241409263,9.41840880919258));
#43073=CARTESIAN_POINT('Ctrl Pts',(-5.03496462672037,25.8229086383713,9.40328537750376));
#43074=CARTESIAN_POINT('Ctrl Pts',(-4.97891809315243,25.8285213367152,9.38784391926512));
#43075=CARTESIAN_POINT('Ctrl Pts',(-4.97191227645643,25.8292229240082,9.38591373698529));
#43076=CARTESIAN_POINT('Ctrl Pts',(-4.9648734425235,25.8299265142188,9.38397858545359));
#43077=CARTESIAN_POINT('Ctrl Pts',(-4.95780155881135,25.8306320663123,9.38203858387997));
#43078=CARTESIAN_POINT('Ctrl Pts',(-4.9507296750992,25.8313376184058,9.38009858230635));
#43079=CARTESIAN_POINT('Ctrl Pts',(-4.9496889160187,25.8314409551873,9.37981464399015));
#43080=CARTESIAN_POINT('Ctrl Pts',(-4.94641136834185,25.8317672566037,9.37891770500492));
#43081=CARTESIAN_POINT('Ctrl Pts',(-4.93985627298814,25.8324198594365,9.37712382703444));
#43082=CARTESIAN_POINT('Ctrl Pts',(-4.93317299793578,25.8330840043494,9.37529867940669));
#43083=CARTESIAN_POINT('Ctrl Pts',(-4.9263614142535,25.8337595501923,9.37344269718707));
#43084=CARTESIAN_POINT('Ctrl Pts',(-4.91273824688894,25.8351106418783,9.36973073274782));
#43085=CARTESIAN_POINT('Ctrl Pts',(-4.8986018450049,25.8365073369903,9.36589542983153));
#43086=CARTESIAN_POINT('Ctrl Pts',(-4.88395128477203,25.837948712664,9.36193973840303));
#43087=CARTESIAN_POINT('Ctrl Pts',(-4.82888918203459,25.8433659236218,9.34707281970699));
#43088=CARTESIAN_POINT('Ctrl Pts',(-4.76656444809351,25.8494139952152,9.33050591088874));
#43089=CARTESIAN_POINT('Ctrl Pts',(-4.69691511772529,25.8560232547324,9.3124519712463));
#43090=CARTESIAN_POINT('Ctrl Pts',(-4.6924371148455,25.8564481875063,9.31129121932976));
#43091=CARTESIAN_POINT('Ctrl Pts',(-4.68792883456788,25.8568754337939,9.31012433765358));
#43092=CARTESIAN_POINT('Ctrl Pts',(-4.68339026042408,25.8573049723977,9.30895139010649));
#43093=CARTESIAN_POINT('Ctrl Pts',(-4.61719980893437,25.8635693526232,9.29184515249631));
#43094=CARTESIAN_POINT('Ctrl Pts',(-4.54456608448041,25.8703224212848,9.27344578850706));
#43095=CARTESIAN_POINT('Ctrl Pts',(-4.46543031231668,25.8774900621148,9.2539735216352));
#43096=CARTESIAN_POINT('Ctrl Pts',(-4.45474238385238,25.8784581101966,9.25134363391598));
#43097=CARTESIAN_POINT('Ctrl Pts',(-4.44393585351717,25.8794336924479,9.24869424872019));
#43098=CARTESIAN_POINT('Ctrl Pts',(-4.4330105765163,25.8804165993201,9.24602597882123));
#43099=CARTESIAN_POINT('Ctrl Pts',(-4.38710136156029,25.8845468820467,9.23481361538715));
#43100=CARTESIAN_POINT('Ctrl Pts',(-4.33909519627864,25.8888067385631,9.22326717421519));
#43101=CARTESIAN_POINT('Ctrl Pts',(-4.28898061558176,25.8931797976848,9.21143417068796));
#43102=CARTESIAN_POINT('Ctrl Pts',(-4.26392332523332,25.8953663272456,9.20551766892434));
#43103=CARTESIAN_POINT('Ctrl Pts',(-4.23833893103118,25.8975811559212,9.19952952600431));
#43104=CARTESIAN_POINT('Ctrl Pts',(-4.2122259637705,25.8998220365003,9.19347619099659));
#43105=CARTESIAN_POINT('Ctrl Pts',(-4.19916948014016,25.9009424767899,9.19044952349273));
#43106=CARTESIAN_POINT('Ctrl Pts',(-4.18598085324542,25.9020694299378,9.18740655792294));
#43107=CARTESIAN_POINT('Ctrl Pts',(-4.17265989938065,25.9032026087186,9.18434811514538));
#43108=CARTESIAN_POINT('Ctrl Pts',(-4.16599942244827,25.903769198109,9.1828188937566));
#43109=CARTESIAN_POINT('Ctrl Pts',(-4.15930586377339,25.9043373438988,9.18128580306261));
#43110=CARTESIAN_POINT('Ctrl Pts',(-4.15257920030619,25.9049070094453,9.17974894750905));
#43111=CARTESIAN_POINT('Ctrl Pts',(-4.14585253683899,25.9054766749918,9.17821209195549));
#43112=CARTESIAN_POINT('Ctrl Pts',(-4.13787834766994,25.906150240868,9.17639538792558));
#43113=CARTESIAN_POINT('Ctrl Pts',(-4.13229987245998,25.9066205284662,9.1751271912668));
#43114=CARTESIAN_POINT('Ctrl Pts',(-4.01426668864598,25.9165711942729,9.14829382126812));
#43115=CARTESIAN_POINT('Ctrl Pts',(-3.89866246388149,25.9259487436324,9.12310703016633));
#43116=CARTESIAN_POINT('Ctrl Pts',(-3.78553933773529,25.9347866014893,9.09944311733136));
#43117=CARTESIAN_POINT('Ctrl Pts',(-3.72757713767392,25.9393149565894,9.08731816554915));
#43118=CARTESIAN_POINT('Ctrl Pts',(-3.67026631241337,25.9437019885214,9.07559218649405));
#43119=CARTESIAN_POINT('Ctrl Pts',(-3.61361387566397,25.9479542173353,9.06424377037705));
#43120=CARTESIAN_POINT('Ctrl Pts',(-3.53000420754008,25.954229806883,9.04749537684419));
#43121=CARTESIAN_POINT('Ctrl Pts',(-3.4478280117861,25.9602100184249,9.03157413172856));
#43122=CARTESIAN_POINT('Ctrl Pts',(-3.36710459947149,25.9659121181529,9.01642319069318));
#43123=CARTESIAN_POINT('Ctrl Pts',(-3.32674289331419,25.9687631680169,9.00884772017549));
#43124=CARTESIAN_POINT('Ctrl Pts',(-3.28674438304887,25.9715446997034,9.00146482919276));
#43125=CARTESIAN_POINT('Ctrl Pts',(-3.24711124803021,25.974258874849,8.99426757532993));
#43126=CARTESIAN_POINT('Ctrl Pts',(-3.21205403583497,25.976659679478,8.98790129479791));
#43127=CARTESIAN_POINT('Ctrl Pts',(-3.17869659599589,25.9789135456954,8.98192974330363));
#43128=CARTESIAN_POINT('Ctrl Pts',(-3.1432884761785,25.9812721261275,8.97568591217661));
#43129=CARTESIAN_POINT('Ctrl Pts',(-3.13866675033491,25.9815799852342,8.97487092183452));
#43130=CARTESIAN_POINT('Ctrl Pts',(-3.13401008629195,25.9818896040878,8.97405136081079));
#43131=CARTESIAN_POINT('Ctrl Pts',(-3.12931014363594,25.9822015197303,8.97322580890466));
#43132=CARTESIAN_POINT('Ctrl Pts',(-2.96648094475864,25.9930078162983,8.94462461834892));
#43133=CARTESIAN_POINT('Ctrl Pts',(-2.80321460460901,26.0030636630445,8.91812930485928));
#43134=CARTESIAN_POINT('Ctrl Pts',(-2.63956869903528,26.0123437147697,8.89376779891749));
#43135=CARTESIAN_POINT('Ctrl Pts',(-2.55774574624841,26.0169837406323,8.8815870459466));
#43136=CARTESIAN_POINT('Ctrl Pts',(-2.47582807006182,26.0214299518029,8.86993939926748));
#43137=CARTESIAN_POINT('Ctrl Pts',(-2.39382320408785,26.0256794517738,8.85882768855804));
#43138=CARTESIAN_POINT('Ctrl Pts',(-2.35282077110086,26.0278042017593,8.85327183320332));
#43139=CARTESIAN_POINT('Ctrl Pts',(-2.3117965406663,26.0298797740671,8.84784996190035));
#43140=CARTESIAN_POINT('Ctrl Pts',(-2.27075145561285,26.0319058064775,8.8425624289481));
#43141=CARTESIAN_POINT('Ctrl Pts',(-2.23483700619109,26.0336785848366,8.83793583761487));
#43142=CARTESIAN_POINT('Ctrl Pts',(-2.19890658995167,26.0354134342236,8.83341209908647));
#43143=CARTESIAN_POINT('Ctrl Pts',(-2.16296083870261,26.0371101115458,8.82899145069237));
#43144=CARTESIAN_POINT('Ctrl Pts',(-2.15782573138132,26.0373524940204,8.82835992949322));
#43145=CARTESIAN_POINT('Ctrl Pts',(-2.15064935712902,26.0376898014891,8.82748121634172));
#43146=CARTESIAN_POINT('Ctrl Pts',(-2.14755457971219,26.0378349211905,8.82710319943079));
#43147=CARTESIAN_POINT('Ctrl Pts',(-2.07171079200998,26.0413913733493,8.81783912952246));
#43148=CARTESIAN_POINT('Ctrl Pts',(-1.98853406425259,26.0450892765804,8.80823185855688));
#43149=CARTESIAN_POINT('Ctrl Pts',(-1.8979985584707,26.0488171805511,8.79857761323498));
#43150=CARTESIAN_POINT('Ctrl Pts',(-1.80788627983242,26.0525276576555,8.78896849870057));
#43151=CARTESIAN_POINT('Ctrl Pts',(-1.71048386265067,26.0562679429853,8.77931284001457));
#43152=CARTESIAN_POINT('Ctrl Pts',(-1.60576582961983,26.0599077783493,8.76995031000074));
#43153=CARTESIAN_POINT('Ctrl Pts',(-1.54093858753986,26.0621610720891,8.76415429777514));
#43154=CARTESIAN_POINT('Ctrl Pts',(-1.47330770039573,26.064375462622,8.7584715702553));
#43155=CARTESIAN_POINT('Ctrl Pts',(-1.40286712366898,26.066515890114,8.75299183003445));
#43156=CARTESIAN_POINT('Ctrl Pts',(-1.2874083954114,26.0700242520217,8.74401002059333));
#43157=CARTESIAN_POINT('Ctrl Pts',(-1.16440227620838,26.0733352030884,8.73557112794578));
#43158=CARTESIAN_POINT('Ctrl Pts',(-1.03383834675618,26.0762729138799,8.72811511444));
#43159=CARTESIAN_POINT('Ctrl Pts',(-0.99560026387569,26.0771332772988,8.72593148176605));
#43160=CARTESIAN_POINT('Ctrl Pts',(-0.956713932107611,26.0779614672454,
8.72383245646009));
#43161=CARTESIAN_POINT('Ctrl Pts',(-0.917179089719602,26.0787526642074,
8.72182982586604));
#43162=CARTESIAN_POINT('Ctrl Pts',(-0.829915811207326,26.0804990336547,
8.71740951960627));
#43163=CARTESIAN_POINT('Ctrl Pts',(-0.739493573310718,26.0820653851727,
8.71345864444578));
#43164=CARTESIAN_POINT('Ctrl Pts',(-0.645913650094968,26.0833957874964,
8.71011175662346));
#43165=CARTESIAN_POINT('Ctrl Pts',(-0.599123688487095,26.0840609886583,
8.70843831271229));
#43166=CARTESIAN_POINT('Ctrl Pts',(-0.551544305404433,26.0846671724655,
8.70691585554372));
#43167=CARTESIAN_POINT('Ctrl Pts',(-0.503176822052515,26.0852068326966,
8.70556207661074));
#43168=CARTESIAN_POINT('Ctrl Pts',(-0.478993080376557,26.0854766628122,
8.70488518714424));
#43169=CARTESIAN_POINT('Ctrl Pts',(-0.454612313630426,26.0857298598239,
8.70425046650503));
#43170=CARTESIAN_POINT('Ctrl Pts',(-0.430034769117113,26.0859654658729,
8.70366013802557));
#43171=CARTESIAN_POINT('Ctrl Pts',(-0.417745996860458,26.0860832688974,
8.70336497378585));
#43172=CARTESIAN_POINT('Ctrl Pts',(-0.405408030162496,26.0861966740309,
8.70308090753664));
#43173=CARTESIAN_POINT('Ctrl Pts',(-0.393020899242947,26.0863055592071,
8.70280822111152));
#43174=CARTESIAN_POINT('Ctrl Pts',(-0.386827333783172,26.0863600017952,
8.70267187789895));
#43175=CARTESIAN_POINT('Ctrl Pts',(-0.38062147726803,26.0864133143842,8.70253837963916));
#43176=CARTESIAN_POINT('Ctrl Pts',(-0.374403333723082,26.0864654815839,
8.70240776175677));
#43177=CARTESIAN_POINT('Ctrl Pts',(-0.368185190178134,26.0865176487837,
8.70227714387437));
#43178=CARTESIAN_POINT('Ctrl Pts',(-0.359951179343043,26.086584673328,8.70210934521882));
#43179=CARTESIAN_POINT('Ctrl Pts',(-0.355712046080956,26.0866185315618,
8.70202458472192));
#43180=CARTESIAN_POINT('Ctrl Pts',(-0.236619695465579,26.087569729932,8.69964336049719));
#43181=CARTESIAN_POINT('Ctrl Pts',(-0.118036481380672,26.0880468078157,
8.69845862330752));
#43182=CARTESIAN_POINT('Ctrl Pts',(8.84627652694544E-13,26.0880528188531,
8.69844059746301));
#43183=CARTESIAN_POINT('Ctrl Pts',(0.150862669520566,26.0880605015723,8.69841755859408));
#43184=CARTESIAN_POINT('Ctrl Pts',(0.300832226640068,26.0872987295697,8.70030104109582));
#43185=CARTESIAN_POINT('Ctrl Pts',(0.449830176676706,26.0858123671823,8.70402388189702));
#43186=CARTESIAN_POINT('Ctrl Pts',(0.582617904676077,26.0844877134917,8.70734169648153));
#43187=CARTESIAN_POINT('Ctrl Pts',(0.714638268422484,26.0825864011306,8.71212360418822));
#43188=CARTESIAN_POINT('Ctrl Pts',(0.845857312319287,26.0801350899488,8.71832934841613));
#43189=CARTESIAN_POINT('Ctrl Pts',(0.911466834267689,26.0789094343579,8.72143222053008));
#43190=CARTESIAN_POINT('Ctrl Pts',(0.976876025877581,26.0775462469279,8.72489104102562));
#43191=CARTESIAN_POINT('Ctrl Pts',(1.04208087423999,26.0760486783595,8.72870073181513));
#43192=CARTESIAN_POINT('Ctrl Pts',(1.0746832984212,26.0752998940752,8.73060557720988));
#43193=CARTESIAN_POINT('Ctrl Pts',(1.10723463677122,26.0745175128011,8.73259813958272));
#43194=CARTESIAN_POINT('Ctrl Pts',(1.13973439403713,26.0737019184225,8.73467778118198));
#43195=CARTESIAN_POINT('Ctrl Pts',(1.15598427267008,26.0732941212332,8.73571760198161));
#43196=CARTESIAN_POINT('Ctrl Pts',(1.17222125603092,26.0728780206698,8.73677919255257));
#43197=CARTESIAN_POINT('Ctrl Pts',(1.18844528299769,26.0724536641226,8.73786247301944));
#43198=CARTESIAN_POINT('Ctrl Pts',(1.19655729648108,26.072241485849,8.73840411325288));
#43199=CARTESIAN_POINT('Ctrl Pts',(1.20466607086589,26.0720272435736,8.73895117595814));
#43200=CARTESIAN_POINT('Ctrl Pts',(1.21277159856042,26.0718109431763,8.73950365116429));
#43201=CARTESIAN_POINT('Ctrl Pts',(1.21682436240769,26.0717027929776,8.73977988876737));
#43202=CARTESIAN_POINT('Ctrl Pts',(1.22087631458238,26.0715941282481,8.74005747949553));
#43203=CARTESIAN_POINT('Ctrl Pts',(1.22492745414149,26.0714849497653,8.74033642196936));
#43204=CARTESIAN_POINT('Ctrl Pts',(1.22695302392105,26.0714303605238,8.74047589320627));
#43205=CARTESIAN_POINT('Ctrl Pts',(1.2289783905467,26.071375642844,8.7406157023796));
#43206=CARTESIAN_POINT('Ctrl Pts',(1.23100355390154,26.0713207968345,8.74075584928271));
#43207=CARTESIAN_POINT('Ctrl Pts',(1.23302871725637,26.0712659508249,8.74089599618582));
#43208=CARTESIAN_POINT('Ctrl Pts',(1.2364307874484,26.071173499238,8.74113225907129));
#43209=CARTESIAN_POINT('Ctrl Pts',(1.23707843403604,26.071155873915,8.74117730300421));
#43210=CARTESIAN_POINT('Ctrl Pts',(1.27880640238213,26.070020271669,8.74407949046734));
#43211=CARTESIAN_POINT('Ctrl Pts',(1.32947418621204,26.0685956982891,8.74772049868581));
#43212=CARTESIAN_POINT('Ctrl Pts',(1.38903588177794,26.0667850967465,8.75236099222838));
#43213=CARTESIAN_POINT('Ctrl Pts',(1.4502568344543,26.0649240558492,8.75713075965802));
#43214=CARTESIAN_POINT('Ctrl Pts',(1.52087413046551,26.0626550531865,8.76295665858922));
#43215=CARTESIAN_POINT('Ctrl Pts',(1.600837921869,26.0598523531197,8.77017538872663));
#43216=CARTESIAN_POINT('Ctrl Pts',(1.68763018423549,26.0568103177776,8.7780105589836));
#43217=CARTESIAN_POINT('Ctrl Pts',(1.78543337805792,26.0531393882259,8.78748663714181));
#43218=CARTESIAN_POINT('Ctrl Pts',(1.89418376361909,26.0486569411145,8.79909572979417));
#43219=CARTESIAN_POINT('Ctrl Pts',(1.97507224561918,26.0453228992109,8.80773056706121));
#43220=CARTESIAN_POINT('Ctrl Pts',(2.06201712669602,26.041539334321,8.81754695154596));
#43221=CARTESIAN_POINT('Ctrl Pts',(2.1549921780888,26.0372258146777,8.82876497934841));
#43222=CARTESIAN_POINT('Ctrl Pts',(2.28380967502505,26.0312494070811,8.84430762482615));
#43223=CARTESIAN_POINT('Ctrl Pts',(2.42418374813402,26.0242460016502,8.86256856411004));
#43224=CARTESIAN_POINT('Ctrl Pts',(2.57592901329186,26.0159217123473,8.88437768472368));
#43225=CARTESIAN_POINT('Ctrl Pts',(2.68639479746009,26.0098618913404,8.90025403913974));
#43226=CARTESIAN_POINT('Ctrl Pts',(2.80288661117011,26.0031018901479,8.9180112218424));
#43227=CARTESIAN_POINT('Ctrl Pts',(2.92533293723364,25.9955370736535,8.93795304949481));
#43228=CARTESIAN_POINT('Ctrl Pts',(3.04038694421305,25.9884289596111,8.95669095084035));
#43229=CARTESIAN_POINT('Ctrl Pts',(3.16069314161519,25.9806061163848,8.97736950665797));
#43230=CARTESIAN_POINT('Ctrl Pts',(3.28616263495456,25.9719648496818,9.00029786548505));
#43231=CARTESIAN_POINT('Ctrl Pts',(3.31917347192997,25.969691345272,9.00633028257074));
#43232=CARTESIAN_POINT('Ctrl Pts',(3.35254171651977,25.9673612973124,9.01251818453037));
#43233=CARTESIAN_POINT('Ctrl Pts',(3.38626574978679,25.9649730755069,9.01886661871804));
#43234=CARTESIAN_POINT('Ctrl Pts',(3.46721789189222,25.9592403190049,9.03410558324042));
#43235=CARTESIAN_POINT('Ctrl Pts',(3.55021941013772,25.9531711026084,9.05027288491658));
#43236=CARTESIAN_POINT('Ctrl Pts',(3.63524343812244,25.9467396041628,9.06744908937538));
#43237=CARTESIAN_POINT('Ctrl Pts',(3.6777554521148,25.94352385494,9.07603719160478));
#43238=CARTESIAN_POINT('Ctrl Pts',(3.72077309357543,25.9402175474073,9.08487752393684));
#43239=CARTESIAN_POINT('Ctrl Pts',(3.76429262432316,25.936817427614,9.09398048718069));
#43240=CARTESIAN_POINT('Ctrl Pts',(3.78605238969703,25.9351173677173,9.09853196880261));
#43241=CARTESIAN_POINT('Ctrl Pts',(3.80793762739503,25.9333938556752,9.10314910848554));
#43242=CARTESIAN_POINT('Ctrl Pts',(3.82994785785757,25.9316464880811,9.10783321552209));
#43243=CARTESIAN_POINT('Ctrl Pts',(3.84095297308885,25.930772804284,9.11017526904036));
#43244=CARTESIAN_POINT('Ctrl Pts',(3.85198933651134,25.9298931566631,9.11253406442057));
#43245=CARTESIAN_POINT('Ctrl Pts',(3.86305688682359,25.9290074948405,9.11490976643313));
#43246=CARTESIAN_POINT('Ctrl Pts',(3.86859066197971,25.9285646639292,9.11609761743942));
#43247=CARTESIAN_POINT('Ctrl Pts',(3.87413223385828,25.9281203294717,9.11728969510533));
#43248=CARTESIAN_POINT('Ctrl Pts',(3.87968159470531,25.9276744851742,9.11848602009804));
#43249=CARTESIAN_POINT('Ctrl Pts',(3.88523095555234,25.9272286408767,9.11968234509074));
#43250=CARTESIAN_POINT('Ctrl Pts',(3.8929759297363,25.9266048156772,9.12135659426671));
#43251=CARTESIAN_POINT('Ctrl Pts',(3.8963530363699,25.9263324164788,9.12208775774814));
#43252=CARTESIAN_POINT('Ctrl Pts',(4.05455254536718,25.9135719608254,9.15633888343296));
#43253=CARTESIAN_POINT('Ctrl Pts',(4.20702422262898,25.9005572533943,9.19143330092842));
#43254=CARTESIAN_POINT('Ctrl Pts',(4.35383997724603,25.8874577523657,9.22692824483611));
#43255=CARTESIAN_POINT('Ctrl Pts',(4.49776644086422,25.8746160456759,9.26172465865618));
#43256=CARTESIAN_POINT('Ctrl Pts',(4.63625740514875,25.861692914023,9.29690585548952));
#43257=CARTESIAN_POINT('Ctrl Pts',(4.76938061674201,25.8488288553367,9.33210103938896));
#43258=CARTESIAN_POINT('Ctrl Pts',(4.90003547357203,25.8362033204973,9.36664363837266));
#43259=CARTESIAN_POINT('Ctrl Pts',(5.02551978873465,25.823634734847,9.40119967260459));
#43260=CARTESIAN_POINT('Ctrl Pts',(5.14589760986401,25.8112364690961,9.43546490646807));
#43261=CARTESIAN_POINT('Ctrl Pts',(5.26549547828554,25.7989185342637,9.46950812882075));
#43262=CARTESIAN_POINT('Ctrl Pts',(5.38005281035675,25.7867687802875,9.5032642479009));
#43263=CARTESIAN_POINT('Ctrl Pts',(5.48963241682708,25.7748781427592,9.53648188896845));
#43264=CARTESIAN_POINT('Ctrl Pts',(5.59870644662265,25.7630423660685,9.56954627100308));
#43265=CARTESIAN_POINT('Ctrl Pts',(5.70284857716153,25.7514633579738,9.60207711615654));
#43266=CARTESIAN_POINT('Ctrl Pts',(5.80212075381237,25.740209928981,9.63387378843652));
#43267=CARTESIAN_POINT('Ctrl Pts',(5.86628467072857,25.7329363493409,9.65442535794184));
#43268=CARTESIAN_POINT('Ctrl Pts',(5.92841411668111,25.7257983564541,9.67467118186661));
#43269=CARTESIAN_POINT('Ctrl Pts',(5.98852581792878,25.7188097818106,9.69456766392382));
#43270=CARTESIAN_POINT('Ctrl Pts',(-6.39567215327757,25.5334667771464,8.78352120081293));
#43271=CARTESIAN_POINT('Ctrl Pts',(-6.35564925405008,25.5378748203104,8.77012420775373));
#43272=CARTESIAN_POINT('Ctrl Pts',(-5.98524856644197,25.5783538673712,8.64740144178755));
#43273=CARTESIAN_POINT('Ctrl Pts',(-5.25616414720834,25.6522250604739,8.42856302669376));
#43274=CARTESIAN_POINT('Ctrl Pts',(-4.17575802099697,25.7436220847966,8.16491184754273));
#43275=CARTESIAN_POINT('Ctrl Pts',(-3.01936659774181,25.8195373983552,7.95089063936762));
#43276=CARTESIAN_POINT('Ctrl Pts',(-1.83578627573155,25.872533317112,7.80508001376507));
#43277=CARTESIAN_POINT('Ctrl Pts',(-0.697926096812265,25.8989853856378,
7.73463115189508));
#43278=CARTESIAN_POINT('Ctrl Pts',(0.331404301561069,25.9017876014486,7.72744126775874));
#43279=CARTESIAN_POINT('Ctrl Pts',(1.24580220706962,25.8874720952612,7.76509235812669));
#43280=CARTESIAN_POINT('Ctrl Pts',(2.07029186482381,25.8615915973225,7.83520238948189));
#43281=CARTESIAN_POINT('Ctrl Pts',(2.81705936567024,25.8276643504536,7.92875394935922));
#43282=CARTESIAN_POINT('Ctrl Pts',(3.49017608565394,25.7886689674746,8.03787750825027));
#43283=CARTESIAN_POINT('Ctrl Pts',(4.0949642222784,25.747012346068,8.15592090125258));
#43284=CARTESIAN_POINT('Ctrl Pts',(4.65004649453019,25.7034080434421,8.28092688614671));
#43285=CARTESIAN_POINT('Ctrl Pts',(5.18049690519974,25.6570345557263,8.4154495605664));
#43286=CARTESIAN_POINT('Ctrl Pts',(5.70541816431205,25.6067236205178,8.56333260888681));
#43287=CARTESIAN_POINT('Ctrl Pts',(6.10978031431405,25.5646825181694,8.6889091565671));
#43288=CARTESIAN_POINT('Ctrl Pts',(6.34031508653319,25.5395632352113,8.76499188397675));
#43289=CARTESIAN_POINT('Ctrl Pts',(6.39541676950722,25.5334956939384,8.78343681303983));
#43290=CARTESIAN_POINT('Ctrl Pts',(-6.33011139739059,25.7770025828591,9.06768825330065));
#43291=CARTESIAN_POINT('Ctrl Pts',(-6.29056321231621,25.7814432939444,9.05437271194277));
#43292=CARTESIAN_POINT('Ctrl Pts',(-5.92452857218488,25.8222252643026,8.93238597022711));
#43293=CARTESIAN_POINT('Ctrl Pts',(-5.203572845008,25.8966944951544,8.71469357563352));
#43294=CARTESIAN_POINT('Ctrl Pts',(-4.13461175586402,25.9888994695799,8.45222824130109));
#43295=CARTESIAN_POINT('Ctrl Pts',(-2.99009397812991,26.065525690553,8.23905800812465));
#43296=CARTESIAN_POINT('Ctrl Pts',(-1.81832922019448,26.1190305753704,8.09376643352996));
#43297=CARTESIAN_POINT('Ctrl Pts',(-0.69152146876971,26.1457315728714,8.0235405665061));
#43298=CARTESIAN_POINT('Ctrl Pts',(0.328402059247375,26.1485587633991,8.01637067248625));
#43299=CARTESIAN_POINT('Ctrl Pts',(1.23408499126555,26.1341108596132,8.05390746812353));
#43300=CARTESIAN_POINT('Ctrl Pts',(2.05049313694551,26.1079833265253,8.12378170806464));
#43301=CARTESIAN_POINT('Ctrl Pts',(2.78979399169512,26.0737316581453,8.21699609755371));
#43302=CARTESIAN_POINT('Ctrl Pts',(3.45606870546097,26.0343678285272,8.32569987339932));
#43303=CARTESIAN_POINT('Ctrl Pts',(4.05461471067682,25.992326080533,8.44325998325948));
#43304=CARTESIAN_POINT('Ctrl Pts',(4.60387478654295,25.9483298974354,8.56772132367673));
#43305=CARTESIAN_POINT('Ctrl Pts',(5.12865373396191,25.9015538253764,8.70161770703905));
#43306=CARTESIAN_POINT('Ctrl Pts',(5.64781964556615,25.8508244104092,8.84875802217962));
#43307=CARTESIAN_POINT('Ctrl Pts',(6.04758703599702,25.8084521556453,8.9736427631715));
#43308=CARTESIAN_POINT('Ctrl Pts',(6.27541106185641,25.783144228056,9.04927164235629));
#43309=CARTESIAN_POINT('Ctrl Pts',(6.32985871986087,25.7770316774931,9.06760427361747));
#43310=CARTESIAN_POINT('Ctrl Pts',(-6.21909462086777,25.836782154238,9.42601905314513));
#43311=CARTESIAN_POINT('Ctrl Pts',(-6.18025121921535,25.8412519032068,9.41291697690927));
#43312=CARTESIAN_POINT('Ctrl Pts',(-5.82072605323139,25.8823021492172,9.29288098658681));
#43313=CARTESIAN_POINT('Ctrl Pts',(-5.11236921245908,25.9572845750022,9.07859409021145));
#43314=CARTESIAN_POINT('Ctrl Pts',(-4.06204085296457,26.0501633515562,8.82020853397432));
#43315=CARTESIAN_POINT('Ctrl Pts',(-2.93762065843339,26.1273686052668,8.61036402280483));
#43316=CARTESIAN_POINT('Ctrl Pts',(-1.78654232977251,26.1812753445501,8.46734625508623));
#43317=CARTESIAN_POINT('Ctrl Pts',(-0.679604906611716,26.2081619982703,
8.39820999068061));
#43318=CARTESIAN_POINT('Ctrl Pts',(0.322775234770271,26.2110063243669,8.39114887629604));
#43319=CARTESIAN_POINT('Ctrl Pts',(1.21259995864587,26.1964622439816,8.42810733714285));
#43320=CARTESIAN_POINT('Ctrl Pts',(2.01460907267051,26.1701446088356,8.49689116067258));
#43321=CARTESIAN_POINT('Ctrl Pts',(2.74086259740854,26.1356362294652,8.58864802757013));
#43322=CARTESIAN_POINT('Ctrl Pts',(3.39541033252112,26.0959750883794,8.6956538995844));
#43323=CARTESIAN_POINT('Ctrl Pts',(3.98346188127814,26.0536180912027,8.81138170964562));
#43324=CARTESIAN_POINT('Ctrl Pts',(4.52312475530119,26.0092972283702,8.93390626645097));
#43325=CARTESIAN_POINT('Ctrl Pts',(5.0387516314274,25.9621835641126,9.06571874387191));
#43326=CARTESIAN_POINT('Ctrl Pts',(5.54885320623593,25.9110981985056,9.21056117041002));
#43327=CARTESIAN_POINT('Ctrl Pts',(5.94159337987235,25.8684387281626,9.33347708049541));
#43328=CARTESIAN_POINT('Ctrl Pts',(6.16536922502574,25.8429639688667,9.40789773397969));
#43329=CARTESIAN_POINT('Ctrl Pts',(6.21884615353447,25.8368113937589,9.42593631502812));
#43330=CARTESIAN_POINT('Ctrl Pts',(-6.09442352525463,25.6959141203215,9.75594787349936));
#43331=CARTESIAN_POINT('Ctrl Pts',(-6.05631315053983,25.7004009763365,9.74313007698199));
#43332=CARTESIAN_POINT('Ctrl Pts',(-5.70357677499405,25.7416081622015,9.62570029038551));
#43333=CARTESIAN_POINT('Ctrl Pts',(-5.00868072692758,25.8168722610937,9.41610186799907));
#43334=CARTESIAN_POINT('Ctrl Pts',(-3.97883577951549,25.9100981342311,9.16351996697486));
#43335=CARTESIAN_POINT('Ctrl Pts',(-2.87697998757772,25.9875850899881,8.95852199803055));
#43336=CARTESIAN_POINT('Ctrl Pts',(-1.74953270103721,26.0416717614473,8.81888051999469));
#43337=CARTESIAN_POINT('Ctrl Pts',(-0.665590719017744,26.0686277716833,
8.75138786955641));
#43338=CARTESIAN_POINT('Ctrl Pts',(0.316136038747394,26.071476502194,8.74449311396111));
#43339=CARTESIAN_POINT('Ctrl Pts',(1.18750276603807,26.0568999322397,8.78057512315524));
#43340=CARTESIAN_POINT('Ctrl Pts',(1.97292052610175,26.0305034336769,8.84772672103612));
#43341=CARTESIAN_POINT('Ctrl Pts',(2.68428382255083,25.9958793975116,8.93732381873537));
#43342=CARTESIAN_POINT('Ctrl Pts',(3.32557899277926,25.9560770317247,9.04184069738195));
#43343=CARTESIAN_POINT('Ctrl Pts',(3.90188993653773,25.913564745964,9.15491273886181));
#43344=CARTESIAN_POINT('Ctrl Pts',(4.43092963053144,25.8690791874711,9.27466385145588));
#43345=CARTESIAN_POINT('Ctrl Pts',(4.93654521767831,25.8217894019311,9.40353243689169));
#43346=CARTESIAN_POINT('Ctrl Pts',(5.43686957263409,25.7705123468464,9.54518075650168));
#43347=CARTESIAN_POINT('Ctrl Pts',(5.82216258062757,25.727691692376,9.665415326738));
#43348=CARTESIAN_POINT('Ctrl Pts',(6.04171208841764,25.7021196038088,9.73821977413358));
#43349=CARTESIAN_POINT('Ctrl Pts',(6.09417956627165,25.6959434303745,9.75586685440467));
#43350=CARTESIAN_POINT('',(6.27159454904157,25.5608537658352,8.76071457497584));
#43351=CARTESIAN_POINT('Origin',(5.999999949017,24.7867247244415,9.33250966431025));
#43352=CARTESIAN_POINT('Ctrl Pts',(-6.27159387327992,25.5608571664729,8.76070928018854));
#43353=CARTESIAN_POINT('Ctrl Pts',(-6.13239664953756,25.575965649089,8.71504798308059));
#43354=CARTESIAN_POINT('Ctrl Pts',(-5.98564492700752,25.5914802261018,8.66855402651474));
#43355=CARTESIAN_POINT('Ctrl Pts',(-5.83132864915275,25.607227821856,8.62173960560949));
#43356=CARTESIAN_POINT('Ctrl Pts',(-5.67907411117793,25.6227650221378,8.57555064794039));
#43357=CARTESIAN_POINT('Ctrl Pts',(-5.51945550480999,25.638529241025,8.52904987089545));
#43358=CARTESIAN_POINT('Ctrl Pts',(-5.35247247516796,25.6543232268546,8.48276842591158));
#43359=CARTESIAN_POINT('Ctrl Pts',(-5.3256661092757,25.6568586902724,8.47533870475417));
#43360=CARTESIAN_POINT('Ctrl Pts',(-5.2986699799632,25.6593948516824,8.46791471659402));
#43361=CARTESIAN_POINT('Ctrl Pts',(-5.27148411637426,25.6619308142419,8.46049875106702));
#43362=CARTESIAN_POINT('Ctrl Pts',(-5.14595239295794,25.6736407144837,8.42625525792378));
#43363=CARTESIAN_POINT('Ctrl Pts',(-5.01637482827605,25.6853470111082,8.39218170988391));
#43364=CARTESIAN_POINT('Ctrl Pts',(-4.88275739379448,25.6969639517451,8.35851824340345));
#43365=CARTESIAN_POINT('Ctrl Pts',(-4.71106409288832,25.7118912768514,8.31526197447118));
#43366=CARTESIAN_POINT('Ctrl Pts',(-4.53269553687205,25.7266725079885,8.27268032221235));
#43367=CARTESIAN_POINT('Ctrl Pts',(-4.34764553912031,25.7411115944755,8.23131618958215));
#43368=CARTESIAN_POINT('Ctrl Pts',(-4.2958392354979,25.7451539382077,8.21973595267237));
#43369=CARTESIAN_POINT('Ctrl Pts',(-4.24350936371134,25.7491693140107,8.20825139413575));
#43370=CARTESIAN_POINT('Ctrl Pts',(-4.19065603668935,25.7531530590042,8.19687502119264));
#43371=CARTESIAN_POINT('Ctrl Pts',(-4.14338231791793,25.7567162488938,8.18669962665356));
#43372=CARTESIAN_POINT('Ctrl Pts',(-4.0956898294982,25.7602541303974,8.17661078502605));
#43373=CARTESIAN_POINT('Ctrl Pts',(-4.04757899994192,25.7637634416522,8.16661761900435));
#43374=CARTESIAN_POINT('Ctrl Pts',(-3.90056248231458,25.7744871544776,8.13608061762375));
#43375=CARTESIAN_POINT('Ctrl Pts',(-3.74963598155595,25.7849451003172,8.10643537283319));
#43376=CARTESIAN_POINT('Ctrl Pts',(-3.59479967329023,25.7950405852558,8.07795017762525));
#43377=CARTESIAN_POINT('Ctrl Pts',(-3.51738151915737,25.8000883277252,8.06370758002128));
#43378=CARTESIAN_POINT('Ctrl Pts',(-3.43898590453603,25.8050453456782,8.04975523934115));
#43379=CARTESIAN_POINT('Ctrl Pts',(-3.35961280206576,25.8098988457103,8.03612821259867));
#43380=CARTESIAN_POINT('Ctrl Pts',(-3.31992625083063,25.8123255957263,8.02931469922742));
#43381=CARTESIAN_POINT('Ctrl Pts',(-3.27999532524208,25.8147264537992,8.02258252424152));
#43382=CARTESIAN_POINT('Ctrl Pts',(-3.23982002132918,25.8170997774362,8.01593617638247));
#43383=CARTESIAN_POINT('Ctrl Pts',(-3.21973236937273,25.8182864392547,8.01261300245294));
#43384=CARTESIAN_POINT('Ctrl Pts',(-3.1995836226854,25.8194662166494,8.00931128595365));
#43385=CARTESIAN_POINT('Ctrl Pts',(-3.17937378027931,25.8206389002878,8.00603159320849));
#43386=CARTESIAN_POINT('Ctrl Pts',(-3.16169016817398,25.8216649984714,8.00316186205647));
#43387=CARTESIAN_POINT('Ctrl Pts',(-3.14395977965026,25.8226856654494,8.00030899287969));
#43388=CARTESIAN_POINT('Ctrl Pts',(-3.12618261395312,25.8237007595066,7.99747336763182));
#43389=CARTESIAN_POINT('Ctrl Pts',(-3.12364301885352,25.8238457729434,7.9970682783107));
#43390=CARTESIAN_POINT('Ctrl Pts',(-3.11986204430108,25.8240613377268,7.99646617419699));
#43391=CARTESIAN_POINT('Ctrl Pts',(-3.11856096474827,25.824135458209,7.99625915656741));
#43392=CARTESIAN_POINT('Ctrl Pts',(-3.09161192020686,25.8256707034384,7.99197123481171));
#43393=CARTESIAN_POINT('Ctrl Pts',(-3.06343761503096,25.8272573707004,7.98754567947991));
#43394=CARTESIAN_POINT('Ctrl Pts',(-3.03403807605523,25.8288897798103,7.98299838251482));
#43395=CARTESIAN_POINT('Ctrl Pts',(-2.96197169591088,25.8328912648526,7.97185170324256));
#43396=CARTESIAN_POINT('Ctrl Pts',(-2.88254322638795,25.8371688494462,7.95997012655567));
#43397=CARTESIAN_POINT('Ctrl Pts',(-2.79575230181482,25.8416266619309,7.9476214331184));
#43398=CARTESIAN_POINT('Ctrl Pts',(-2.70929163338439,25.8460675115826,7.93531972883216));
#43399=CARTESIAN_POINT('Ctrl Pts',(-2.61552418771846,25.8506872657355,7.92255446105429));
#43400=CARTESIAN_POINT('Ctrl Pts',(-2.51445069720308,25.855372905854,7.90963877170834));
#43401=CARTESIAN_POINT('Ctrl Pts',(-2.50259151428056,25.8559226826846,7.90812334445098));
#43402=CARTESIAN_POINT('Ctrl Pts',(-2.4906317538322,25.8564733453643,7.90660590131109));
#43403=CARTESIAN_POINT('Ctrl Pts',(-2.47857142058778,25.8570246943066,7.90508699199917));
#43404=CARTESIAN_POINT('Ctrl Pts',(-2.37688555907985,25.8616733545927,7.89228041370609));
#43405=CARTESIAN_POINT('Ctrl Pts',(-2.26804970880952,25.8663725677609,7.8793659892952));
#43406=CARTESIAN_POINT('Ctrl Pts',(-2.15206266310375,25.8709939097392,7.86670049242327));
#43407=CARTESIAN_POINT('Ctrl Pts',(-2.11969726318713,25.8722834639335,7.86316627126169));
#43408=CARTESIAN_POINT('Ctrl Pts',(-2.08677508025734,25.8735668397906,7.85965171818127));
#43409=CARTESIAN_POINT('Ctrl Pts',(-2.05329620826432,25.8748409764783,7.85616525032574));
#43410=CARTESIAN_POINT('Ctrl Pts',(-1.97656808888935,25.8777610901518,7.84817483410527));
#43411=CARTESIAN_POINT('Ctrl Pts',(-1.89691549423532,25.8806329596912,7.84033139016118));
#43412=CARTESIAN_POINT('Ctrl Pts',(-1.81433837908348,25.8834176187708,7.83274216046773));
#43413=CARTESIAN_POINT('Ctrl Pts',(-1.81240130548538,25.8834829406166,7.8325641341896));
#43414=CARTESIAN_POINT('Ctrl Pts',(-1.81046262264534,25.8835482142048,7.8323862480318));
#43415=CARTESIAN_POINT('Ctrl Pts',(-1.80852233054424,25.8836134390365,7.83220850346248));
#43416=CARTESIAN_POINT('Ctrl Pts',(-1.76910546295402,25.8849384758959,7.82859763778417));
#43417=CARTESIAN_POINT('Ctrl Pts',(-1.72902444752696,25.8862434067418,7.82504517372945));
#43418=CARTESIAN_POINT('Ctrl Pts',(-1.6882793075523,25.8875239410946,7.82156332312573));
#43419=CARTESIAN_POINT('Ctrl Pts',(-1.66690389946438,25.8881957253707,7.81973670091749));
#43420=CARTESIAN_POINT('Ctrl Pts',(-1.64534571114051,25.8888607903948,7.81792951642983));
#43421=CARTESIAN_POINT('Ctrl Pts',(-1.62360474343983,25.889518493133,7.81614356880621));
#43422=CARTESIAN_POINT('Ctrl Pts',(-1.6127342595895,25.8898473445022,7.81525059499439));
#43423=CARTESIAN_POINT('Ctrl Pts',(-1.60181808086,25.8901743549559,7.8143629306771));
#43424=CARTESIAN_POINT('Ctrl Pts',(-1.59085620735388,25.8904994430688,7.81348080371653));
#43425=CARTESIAN_POINT('Ctrl Pts',(-1.58537527060083,25.8906619871253,7.81303974023625));
#43426=CARTESIAN_POINT('Ctrl Pts',(-1.57988291015145,25.8908240505749,7.81260006111269));
#43427=CARTESIAN_POINT('Ctrl Pts',(-1.57437912601871,25.8909856231766,7.81216179501871));
#43428=CARTESIAN_POINT('Ctrl Pts',(-1.56887534188597,25.8911471957783,7.81172352892473));
#43429=CARTESIAN_POINT('Ctrl Pts',(-1.56205961599394,25.8913460650961,7.81118421557168));
#43430=CARTESIAN_POINT('Ctrl Pts',(-1.55783350257863,25.89146885813,7.81085126459434));
#43431=CARTESIAN_POINT('Ctrl Pts',(-1.33210010952135,25.8980277185939,7.79306703912503));
#43432=CARTESIAN_POINT('Ctrl Pts',(-1.11005333250434,25.9030589041166,7.7794380791357));
#43433=CARTESIAN_POINT('Ctrl Pts',(-0.89169622994583,25.906695435275,7.76958900504006));
#43434=CARTESIAN_POINT('Ctrl Pts',(-0.848420263737139,25.907416155589,7.7676370273267));
#43435=CARTESIAN_POINT('Ctrl Pts',(-0.805289118208011,25.9080820825321,
7.76583364434555));
#43436=CARTESIAN_POINT('Ctrl Pts',(-0.762302665091636,25.9086942316615,
7.76417611739813));
#43437=CARTESIAN_POINT('Ctrl Pts',(-0.724717141794447,25.9092294687816,
7.76272684644923));
#43438=CARTESIAN_POINT('Ctrl Pts',(-0.68724222102171,25.9097235717933,7.76138905797346));
#43439=CARTESIAN_POINT('Ctrl Pts',(-0.649878100577331,25.9101771201779,
7.76016085477969));
#43440=CARTESIAN_POINT('Ctrl Pts',(-0.558066277942419,25.911291587837,7.75714289068888));
#43441=CARTESIAN_POINT('Ctrl Pts',(-0.466923505753704,25.9121612114512,
7.75478652107046));
#43442=CARTESIAN_POINT('Ctrl Pts',(-0.376449018564199,25.9127967453162,
7.7530636364847));
#43443=CARTESIAN_POINT('Ctrl Pts',(-0.312801838539285,25.9132438319986,
7.75185161806052));
#43444=CARTESIAN_POINT('Ctrl Pts',(-0.249485544181297,25.913575012163,7.75095306737938));
#43445=CARTESIAN_POINT('Ctrl Pts',(-0.186500135809807,25.9137938238034,
7.75035834235737));
#43446=CARTESIAN_POINT('Ctrl Pts',(-0.155007431624062,25.9139032296236,
7.75006097984637));
#43447=CARTESIAN_POINT('Ctrl Pts',(-0.123597448811888,25.9139845409445,
7.74983957568175));
#43448=CARTESIAN_POINT('Ctrl Pts',(-0.0922701869944179,25.9140381879309,
7.74969293815496));
#43449=CARTESIAN_POINT('Ctrl Pts',(-0.0647192837063548,25.9140853680178,
7.74956397711321));
#43450=CARTESIAN_POINT('Ctrl Pts',(-0.0383381534770102,25.9141107435395,
7.74949397605362));
#43451=CARTESIAN_POINT('Ctrl Pts',(-0.0102093113128477,25.9141157540723,
7.74947894090337));
#43452=CARTESIAN_POINT('Ctrl Pts',(-0.00635373562016292,25.9141164408581,
7.74947688005921));
#43453=CARTESIAN_POINT('Ctrl Pts',(-0.00246532424755673,25.9141167168094,
7.74947592639803));
#43454=CARTESIAN_POINT('Ctrl Pts',(0.00146343592704603,25.9141165580605,
7.74947614237112));
#43455=CARTESIAN_POINT('Ctrl Pts',(0.123996040186545,25.9141116069004,7.74948287827353));
#43456=CARTESIAN_POINT('Ctrl Pts',(0.246525247851146,25.9136952230428,7.75063924297031));
#43457=CARTESIAN_POINT('Ctrl Pts',(0.369056161634649,25.9128591689236,7.75293700917956));
#43458=CARTESIAN_POINT('Ctrl Pts',(0.64487089222353,25.9109772271792,7.75810923672925));
#43459=CARTESIAN_POINT('Ctrl Pts',(0.920694080572269,25.9069699675977,7.76906155340267));
#43460=CARTESIAN_POINT('Ctrl Pts',(1.19651513952632,25.9008591996694,7.78581189746439));
#43461=CARTESIAN_POINT('Ctrl Pts',(1.22211216209444,25.9002921020549,7.78736637969499));
#43462=CARTESIAN_POINT('Ctrl Pts',(1.24770916810565,25.8997068763829,7.7889708319627));
#43463=CARTESIAN_POINT('Ctrl Pts',(1.27330614986382,25.8991035329777,7.79062529025566));
#43464=CARTESIAN_POINT('Ctrl Pts',(1.37082342231014,25.8968049649756,7.7969283091674));
#43465=CARTESIAN_POINT('Ctrl Pts',(1.46834034405745,25.8942434560884,7.80395705460546));
#43466=CARTESIAN_POINT('Ctrl Pts',(1.56585686824688,25.89141831084,7.81170938455013));
#43467=CARTESIAN_POINT('Ctrl Pts',(1.74017752234041,25.8863680778491,7.82556745873741));
#43468=CARTESIAN_POINT('Ctrl Pts',(1.91449856142016,25.880476413635,7.84173859307239));
#43469=CARTESIAN_POINT('Ctrl Pts',(2.08881914766684,25.8737425938397,7.86022312559126));
#43470=CARTESIAN_POINT('Ctrl Pts',(2.17523066091776,25.8704046085162,7.86938599304761));
#43471=CARTESIAN_POINT('Ctrl Pts',(2.26164204568451,25.8668596485272,7.87911743613203));
#43472=CARTESIAN_POINT('Ctrl Pts',(2.34805359304106,25.863107937854,7.88941699556841));
#43473=CARTESIAN_POINT('Ctrl Pts',(2.47841969424383,25.8574478622245,7.90495558327923));
#43474=CARTESIAN_POINT('Ctrl Pts',(2.60878583457507,25.8513174294346,7.92178731779572));
#43475=CARTESIAN_POINT('Ctrl Pts',(2.73915198671474,25.8447165662376,7.93991205144734));
#43476=CARTESIAN_POINT('Ctrl Pts',(2.77254322425417,25.8430258590459,7.94455441663774));
#43477=CARTESIAN_POINT('Ctrl Pts',(2.80593446849372,25.8413042753965,7.94928160882464));
#43478=CARTESIAN_POINT('Ctrl Pts',(2.83932570100359,25.8395518100846,7.95409365064916));
#43479=CARTESIAN_POINT('Ctrl Pts',(2.87111753474536,25.8378832856951,7.95867520161762));
#43480=CARTESIAN_POINT('Ctrl Pts',(2.90290935782796,25.836186767153,7.96333366859984));
#43481=CARTESIAN_POINT('Ctrl Pts',(2.93470118626495,25.8344622609784,7.96806902210271));
#43482=CARTESIAN_POINT('Ctrl Pts',(2.98358847779635,25.8318104337559,7.97535072367763));
#43483=CARTESIAN_POINT('Ctrl Pts',(3.03247576585934,25.829092441693,7.98281424533809));
#43484=CARTESIAN_POINT('Ctrl Pts',(3.08136305634897,25.8263083276583,7.9904595402296));
#43485=CARTESIAN_POINT('Ctrl Pts',(3.09765881984551,25.8253802896468,7.99300797186011));
#43486=CARTESIAN_POINT('Ctrl Pts',(3.11203761009798,25.8245558039489,7.99527206090195));
#43487=CARTESIAN_POINT('Ctrl Pts',(3.13025034766616,25.8235021731655,7.99816542552789));
#43488=CARTESIAN_POINT('Ctrl Pts',(3.25876974095643,25.8160671575057,8.0185826453391));
#43489=CARTESIAN_POINT('Ctrl Pts',(3.38586955214421,25.8083003352541,8.04008423985018));
#43490=CARTESIAN_POINT('Ctrl Pts',(3.51153601864061,25.8002315699843,8.06258511763896));
#43491=CARTESIAN_POINT('Ctrl Pts',(3.71379593233212,25.7872449092419,8.09880023314611));
#43492=CARTESIAN_POINT('Ctrl Pts',(3.9123420147794,25.7734766580682,8.13760300891054));
#43493=CARTESIAN_POINT('Ctrl Pts',(4.1071405034411,25.75904847144,8.17864699109328));
#43494=CARTESIAN_POINT('Ctrl Pts',(4.29249186418904,25.7453200075127,8.21770046630425));
#43495=CARTESIAN_POINT('Ctrl Pts',(4.47445059164769,25.7309940292942,8.25878319076582));
#43496=CARTESIAN_POINT('Ctrl Pts',(4.65300686532189,25.7161712833696,8.30161093596719));
#43497=CARTESIAN_POINT('Ctrl Pts',(4.83064737870333,25.7014245587568,8.34421903081588));
#43498=CARTESIAN_POINT('Ctrl Pts',(5.00492039797542,25.6861862006155,8.3885543902908));
#43499=CARTESIAN_POINT('Ctrl Pts',(5.17583188151053,25.6705523550977,8.43435430849758));
#43500=CARTESIAN_POINT('Ctrl Pts',(5.35320454352684,25.6543274839557,8.48188565773427));
#43501=CARTESIAN_POINT('Ctrl Pts',(5.52695678568221,25.6376768256315,8.53099447907734));
#43502=CARTESIAN_POINT('Ctrl Pts',(5.69711015110884,25.6207054195578,8.58141011157052));
#43503=CARTESIAN_POINT('Ctrl Pts',(5.87744252567627,25.6027187406029,8.63484173603484));
#43504=CARTESIAN_POINT('Ctrl Pts',(6.05373257749037,25.5843721248016,8.68974139055599));
#43505=CARTESIAN_POINT('Ctrl Pts',(6.2260191449712,25.5657894695239,8.74581872722904));
#43506=CARTESIAN_POINT('Ctrl Pts',(6.24124268425681,25.5641474739418,8.75077381775268));
#43507=CARTESIAN_POINT('Ctrl Pts',(6.25643497131818,25.5625036240469,8.75573811142633));
#43508=CARTESIAN_POINT('Ctrl Pts',(6.27159604048006,25.5608580129971,8.7607114336902));
#43509=CARTESIAN_POINT('Origin',(5.999999999061,24.7867247845918,9.33250979146072));
#43510=CARTESIAN_POINT('Origin',(5.99996968669486,24.786693647859,9.33251391748345));
#43511=CARTESIAN_POINT('Ctrl Pts',(6.2417693835149,15.8394371419482,3.89966763071918));
#43512=CARTESIAN_POINT('Ctrl Pts',(6.29480660013804,15.8210003804235,3.91290159518924));
#43513=CARTESIAN_POINT('Ctrl Pts',(6.43873775859606,15.7672282165569,3.96076091853584));
#43514=CARTESIAN_POINT('Ctrl Pts',(6.6574605393883,15.6678516583381,4.08940826000748));
#43515=CARTESIAN_POINT('Ctrl Pts',(6.86734070593742,15.5432497310862,4.30355889900136));
#43516=CARTESIAN_POINT('Ctrl Pts',(7.01531432749514,15.4204361246427,4.56089237217717));
#43517=CARTESIAN_POINT('Ctrl Pts',(7.09527320778199,15.3106118534239,4.83061809734207));
#43518=CARTESIAN_POINT('Ctrl Pts',(7.10994677008608,15.2460735777555,5.0132274309249));
#43519=CARTESIAN_POINT('Ctrl Pts',(7.10820127775525,15.2174916046755,5.10034196570805));
#43520=CARTESIAN_POINT('Ctrl Pts',(7.10813648779779,15.2165799927952,5.10312736513287));
#43521=CARTESIAN_POINT('Ctrl Pts',(6.04288609483464,15.2236247505278,3.8631163616068));
#43522=CARTESIAN_POINT('Ctrl Pts',(6.08960513438832,15.2073416533561,3.87444417175601));
#43523=CARTESIAN_POINT('Ctrl Pts',(6.21669065164213,15.1597345425427,3.91554209118234));
#43524=CARTESIAN_POINT('Ctrl Pts',(6.41097421036258,15.0712598304035,4.02691979479796));
#43525=CARTESIAN_POINT('Ctrl Pts',(6.59849709551467,14.9599216454064,4.21386278649374));
#43526=CARTESIAN_POINT('Ctrl Pts',(6.73122625671432,14.8501808036311,4.43977189790894));
#43527=CARTESIAN_POINT('Ctrl Pts',(6.80304009224872,14.7524265349867,4.67721487713722));
#43528=CARTESIAN_POINT('Ctrl Pts',(6.81617737917041,14.6954476818957,4.83787645047658));
#43529=CARTESIAN_POINT('Ctrl Pts',(6.81461541449534,14.6703824924246,4.91434573780175));
#43530=CARTESIAN_POINT('Ctrl Pts',(6.81455743808829,14.6695832352687,4.91679057943266));
#43531=CARTESIAN_POINT('Ctrl Pts',(6.02645463242452,14.8077937469123,3.36555058259603));
#43532=CARTESIAN_POINT('Ctrl Pts',(6.0909048021779,14.7857891518488,3.38107551335727));
#43533=CARTESIAN_POINT('Ctrl Pts',(6.26494841949978,14.7221064653423,3.43708239772331));
#43534=CARTESIAN_POINT('Ctrl Pts',(6.52611209862578,14.6065921781731,3.58601226673634));
#43535=CARTESIAN_POINT('Ctrl Pts',(6.77358742595278,14.4642384951137,3.83063358124898));
#43536=CARTESIAN_POINT('Ctrl Pts',(6.94658414411926,14.3254403906868,4.12182395730633));
#43537=CARTESIAN_POINT('Ctrl Pts',(7.03979999596078,14.2018202245916,4.4257862610867));
#43538=CARTESIAN_POINT('Ctrl Pts',(7.05702527180377,14.1289362505915,4.63206598706388));
#43539=CARTESIAN_POINT('Ctrl Pts',(7.05497400841223,14.0964786467982,4.73097960482542));
#43540=CARTESIAN_POINT('Ctrl Pts',(7.05489786501909,14.0954432215508,4.73414280665572));
#43541=CARTESIAN_POINT('Ctrl Pts',(6.20434274665245,14.8765684418783,2.74504865258545));
#43542=CARTESIAN_POINT('Ctrl Pts',(6.29855278522411,14.84484558641,2.76803006088607));
#43543=CARTESIAN_POINT('Ctrl Pts',(6.55152406662262,14.7537433506342,2.85051411109445));
#43544=CARTESIAN_POINT('Ctrl Pts',(6.92554893952471,14.5915746583482,3.06637382200757));
#43545=CARTESIAN_POINT('Ctrl Pts',(7.27464606008605,14.3949448866597,3.41448089961097));
#43546=CARTESIAN_POINT('Ctrl Pts',(7.51612671900243,14.2046487813112,3.82343069258363));
#43547=CARTESIAN_POINT('Ctrl Pts',(7.64578429976314,14.0347520877583,4.24764907618302));
#43548=CARTESIAN_POINT('Ctrl Pts',(7.66995071774345,13.9332743711703,4.53620693589844));
#43549=CARTESIAN_POINT('Ctrl Pts',(7.66706900976556,13.8875235981543,4.67544806374864));
#43550=CARTESIAN_POINT('Ctrl Pts',(7.66696203369115,13.8860634885015,4.67990184251473));
#43551=CARTESIAN_POINT('',(6.9999997358383,14.7967908123979,4.92966736370966));
#43552=CARTESIAN_POINT('',(7.00000022915846,14.5427406233569,3.16613333521326));
#43553=CARTESIAN_POINT('Ctrl Pts',(7.,14.7967908124046,4.92966736369987));
#43554=CARTESIAN_POINT('Ctrl Pts',(7.,14.7551697581394,4.82500542408383));
#43555=CARTESIAN_POINT('Ctrl Pts',(7.,14.7202719475865,4.7308289607362));
#43556=CARTESIAN_POINT('Ctrl Pts',(7.,14.6923688673053,4.64894777974916));
#43557=CARTESIAN_POINT('Ctrl Pts',(7.,14.6784173271647,4.60800718925564));
#43558=CARTESIAN_POINT('Ctrl Pts',(7.,14.666162916251,4.57015546746193));
#43559=CARTESIAN_POINT('Ctrl Pts',(7.,14.655417087011,4.53564364192123));
#43560=CARTESIAN_POINT('Ctrl Pts',(7.,14.650044172391,4.51838772915088));
#43561=CARTESIAN_POINT('Ctrl Pts',(7.,14.6450467875392,4.50196675534175));
#43562=CARTESIAN_POINT('Ctrl Pts',(7.,14.6403945300219,4.48641068966369));
#43563=CARTESIAN_POINT('Ctrl Pts',(7.,14.6380684012632,4.47863265682467));
#43564=CARTESIAN_POINT('Ctrl Pts',(7.,14.6358285543382,4.47107085101841));
#43565=CARTESIAN_POINT('Ctrl Pts',(7.,14.6336709343289,4.46372880000887));
#43566=CARTESIAN_POINT('Ctrl Pts',(7.,14.6325921243242,4.46005777450411));
#43567=CARTESIAN_POINT('Ctrl Pts',(7.,14.6315338710485,4.45644168769852));
#43568=CARTESIAN_POINT('Ctrl Pts',(7.,14.6304956715052,4.45288096933233));
#43569=CARTESIAN_POINT('Ctrl Pts',(7.,14.6294574719619,4.44932025096614));
#43570=CARTESIAN_POINT('Ctrl Pts',(7.,14.6289382246372,4.4475382963016));
#43571=CARTESIAN_POINT('Ctrl Pts',(7.,14.6274407295948,4.44236534461973));
#43572=CARTESIAN_POINT('Ctrl Pts',(7.,14.603480808917,4.35959811770983));
#43573=CARTESIAN_POINT('Ctrl Pts',(7.,14.5830120743208,4.27935669050358));
#43574=CARTESIAN_POINT('Ctrl Pts',(7.,14.5661204867627,4.20226777656473));
#43575=CARTESIAN_POINT('Ctrl Pts',(7.,14.5492288992046,4.12517886262588));
#43576=CARTESIAN_POINT('Ctrl Pts',(7.,14.5361235670877,4.05275636196388));
#43577=CARTESIAN_POINT('Ctrl Pts',(7.,14.5256463779026,3.98125693906969));
#43578=CARTESIAN_POINT('Ctrl Pts',(7.,14.5046919995326,3.8382580932813));
#43579=CARTESIAN_POINT('Ctrl Pts',(7.,14.4945143427946,3.69578853863727));
#43580=CARTESIAN_POINT('Ctrl Pts',(7.,14.4974004966839,3.55817078061321));
#43581=CARTESIAN_POINT('Ctrl Pts',(7.,14.5002866505733,3.42055302258915));
#43582=CARTESIAN_POINT('Ctrl Pts',(7.,14.5162046706628,3.28801013281503));
#43583=CARTESIAN_POINT('Ctrl Pts',(7.,14.5427403138302,3.1661340810964));
#43584=CARTESIAN_POINT('',(6.2499447585205,14.859388404893,2.76546247674145));
#43585=CARTESIAN_POINT('Ctrl Pts',(6.24994458389757,14.8593878111664,2.76546236623351));
#43586=CARTESIAN_POINT('Ctrl Pts',(6.29980716926801,14.8422034238441,2.77899714130872));
#43587=CARTESIAN_POINT('Ctrl Pts',(6.34865165736493,14.8247500216694,2.79442084961687));
#43588=CARTESIAN_POINT('Ctrl Pts',(6.39650063437509,14.8070371392973,2.81164832003518));
#43589=CARTESIAN_POINT('Ctrl Pts',(6.42315488865876,14.7971701849684,2.82124487582145));
#43590=CARTESIAN_POINT('Ctrl Pts',(6.44950007514397,14.787222497999,2.83140207154089));
#43591=CARTESIAN_POINT('Ctrl Pts',(6.4755382818578,14.7771943490334,2.8421117724326));
#43592=CARTESIAN_POINT('Ctrl Pts',(6.52301982831677,14.7589076818199,2.86164127252605));
#43593=CARTESIAN_POINT('Ctrl Pts',(6.56948212852928,14.740353824833,2.88300539426928));
#43594=CARTESIAN_POINT('Ctrl Pts',(6.61495863330414,14.7215228869671,2.90616780645185));
#43595=CARTESIAN_POINT('Ctrl Pts',(6.62617146692926,14.7168798702195,2.91187880547091));
#43596=CARTESIAN_POINT('Ctrl Pts',(6.63732425001315,14.7122199768811,2.9176993436247));
#43597=CARTESIAN_POINT('Ctrl Pts',(6.6484172330222,14.7075430018446,2.92362928654739));
#43598=CARTESIAN_POINT('Ctrl Pts',(6.69398623825065,14.6883303969287,2.94798897409292));
#43599=CARTESIAN_POINT('Ctrl Pts',(6.73852982859227,14.6688362321768,2.9741895171999));
#43600=CARTESIAN_POINT('Ctrl Pts',(6.78203884617526,14.6490475988644,3.00223984763589));
#43601=CARTESIAN_POINT('Ctrl Pts',(6.82408097367041,14.629926131847,3.0293444717801));
#43602=CARTESIAN_POINT('Ctrl Pts',(6.86515740984907,14.6105295250194,3.05817677588614));
#43603=CARTESIAN_POINT('Ctrl Pts',(6.90522597828194,14.5908446770955,3.08877620005188));
#43604=CARTESIAN_POINT('Ctrl Pts',(6.93747899216091,14.5749994473275,3.11340706885768));
#43605=CARTESIAN_POINT('Ctrl Pts',(6.96907832380679,14.5589674064224,3.13918361820505));
#43606=CARTESIAN_POINT('Ctrl Pts',(7.00000068579859,14.5427398601927,3.16613235169124));
#43607=CARTESIAN_POINT('',(6.26385811009516,15.8144409652449,3.90573611874549));
#43608=CARTESIAN_POINT('Origin',(6.52771826980506,15.8038104576537,2.94124750390268));
#43609=CARTESIAN_POINT('Ctrl Pts',(6.26385556519314,15.8144410677384,3.90574542181138));
#43610=CARTESIAN_POINT('Ctrl Pts',(6.30364984979714,15.7888354137076,3.91691345720727));
#43611=CARTESIAN_POINT('Ctrl Pts',(6.34303406289391,15.7620196111154,3.9307005085015));
#43612=CARTESIAN_POINT('Ctrl Pts',(6.3816518889474,15.7340505126519,3.94714461691159));
#43613=CARTESIAN_POINT('Ctrl Pts',(6.4267935123979,15.7013565306203,3.96636666604505));
#43614=CARTESIAN_POINT('Ctrl Pts',(6.47088863867637,15.667085953782,3.98922019532522));
#43615=CARTESIAN_POINT('Ctrl Pts',(6.51341066571092,15.6313661843138,4.01561497269632));
#43616=CARTESIAN_POINT('Ctrl Pts',(6.53319158177353,15.6147496255347,4.02789361772057));
#43617=CARTESIAN_POINT('Ctrl Pts',(6.55263143917655,15.5978197383494,4.040938560204));
#43618=CARTESIAN_POINT('Ctrl Pts',(6.57167361680582,15.5805908621124,4.05474088366913));
#43619=CARTESIAN_POINT('Ctrl Pts',(6.58329053398495,15.570080171989,4.06316116267796));
#43620=CARTESIAN_POINT('Ctrl Pts',(6.59475941100498,15.5594582226939,4.0718633354495));
#43621=CARTESIAN_POINT('Ctrl Pts',(6.60606691947575,15.5487284531784,4.08084546649594));
#43622=CARTESIAN_POINT('Ctrl Pts',(6.64408869308806,15.5126493409245,4.11104810168181));
#43623=CARTESIAN_POINT('Ctrl Pts',(6.68028910165754,15.4753495562228,4.14441625586059));
#43624=CARTESIAN_POINT('Ctrl Pts',(6.71423321238755,15.4369829533116,4.18075365161009));
#43625=CARTESIAN_POINT('Ctrl Pts',(6.73210524393638,15.4167824200556,4.1998857799608));
#43626=CARTESIAN_POINT('Ctrl Pts',(6.74935110305278,15.3962864909449,4.21984101266869));
#43627=CARTESIAN_POINT('Ctrl Pts',(6.76590188515017,15.3755200500137,4.24059109905349));
#43628=CARTESIAN_POINT('Ctrl Pts',(6.77350227475515,15.3659837609818,4.2501198778105));
#43629=CARTESIAN_POINT('Ctrl Pts',(6.78095602918618,15.3563904507545,4.25981628327801));
#43630=CARTESIAN_POINT('Ctrl Pts',(6.78825615479716,15.3467426609164,4.26967762130588));
#43631=CARTESIAN_POINT('Ctrl Pts',(6.790134185423,15.3442606700914,4.27221454954726));
#43632=CARTESIAN_POINT('Ctrl Pts',(6.79200204735593,15.3417750740821,4.27476239367609));
#43633=CARTESIAN_POINT('Ctrl Pts',(6.79385965046825,15.3392859192095,4.27732107911455));
#43634=CARTESIAN_POINT('Ctrl Pts',(6.79839881275779,15.333203523107,4.2835733772379));
#43635=CARTESIAN_POINT('Ctrl Pts',(6.80287673363183,15.3270998599874,4.28989042541093));
#43636=CARTESIAN_POINT('Ctrl Pts',(6.80729206658171,15.3209756341991,4.2962711170141));
#43637=CARTESIAN_POINT('Ctrl Pts',(6.80949973305664,15.317913521305,4.29946146281569));
#43638=CARTESIAN_POINT('Ctrl Pts',(6.81169175208366,15.3148462677536,4.30266771930985));
#43639=CARTESIAN_POINT('Ctrl Pts',(6.81386795551184,15.3117739591357,4.30588975184288));
#43640=CARTESIAN_POINT('Ctrl Pts',(6.81548498418286,15.3094910792096,4.30828388417325));
#43641=CARTESIAN_POINT('Ctrl Pts',(6.81751779611187,15.3065994703175,4.31132427339662));
#43642=CARTESIAN_POINT('Ctrl Pts',(6.81901903291707,15.3044498470018,4.3135904229623));
#43643=CARTESIAN_POINT('Ctrl Pts',(6.8195381664,15.3037064989604,4.31437406623084));
#43644=CARTESIAN_POINT('Ctrl Pts',(6.81999417601719,15.303051900134,4.31506478744318));
#43645=CARTESIAN_POINT('Ctrl Pts',(6.82034894851834,15.3025419553618,4.31560304213719));
#43646=CARTESIAN_POINT('Ctrl Pts',(6.83460303192456,15.2820533456421,4.33722909059689));
#43647=CARTESIAN_POINT('Ctrl Pts',(6.84880149062183,15.2603765087782,4.36053116336644));
#43648=CARTESIAN_POINT('Ctrl Pts',(6.86266115088873,15.2375350020463,4.38562159480448));
#43649=CARTESIAN_POINT('Ctrl Pts',(6.87577607619647,15.2159208607949,4.409363817046));
#43650=CARTESIAN_POINT('Ctrl Pts',(6.88858775800522,15.1932637307109,4.43470749378823));
#43651=CARTESIAN_POINT('Ctrl Pts',(6.90081536935772,15.1696006099861,4.46173298293594));
#43652=CARTESIAN_POINT('Ctrl Pts',(6.90556277146064,15.1604133414468,4.47222569981362));
#43653=CARTESIAN_POINT('Ctrl Pts',(6.91022166644203,15.1510746283178,4.48297175954424));
#43654=CARTESIAN_POINT('Ctrl Pts',(6.91477373620808,15.1415874471195,4.49397515925285));
#43655=CARTESIAN_POINT('Ctrl Pts',(6.92451241417757,15.1212906135304,4.51751578403212));
#43656=CARTESIAN_POINT('Ctrl Pts',(6.93376334490682,15.1003134238407,4.54223534254804));
#43657=CARTESIAN_POINT('Ctrl Pts',(6.94234872663041,15.0786949537686,4.56814999140341));
#43658=CARTESIAN_POINT('Ctrl Pts',(6.95179572114869,15.0549068946186,4.59666538577509));
#43659=CARTESIAN_POINT('Ctrl Pts',(6.96043775178613,15.0303418978765,4.62662830347885));
#43660=CARTESIAN_POINT('Ctrl Pts',(6.96800702070548,15.0050707208775,4.65803766375443));
#43661=CARTESIAN_POINT('Ctrl Pts',(6.97344665173649,14.9869096699149,4.68060990060317));
#43662=CARTESIAN_POINT('Ctrl Pts',(6.97833162733887,14.9683843006087,4.70392867568163));
#43663=CARTESIAN_POINT('Ctrl Pts',(6.98254997944005,14.9495281509576,4.72798518062679));
#43664=CARTESIAN_POINT('Ctrl Pts',(6.98802445617009,14.9250570897451,4.75920513888767));
#43665=CARTESIAN_POINT('Ctrl Pts',(6.99237688658608,14.9000279909683,4.79166907499824));
#43666=CARTESIAN_POINT('Ctrl Pts',(6.99536960101161,14.8745360686185,4.82531024797829));
#43667=CARTESIAN_POINT('Ctrl Pts',(6.99836231543714,14.8490441462688,4.85895142095833));
#43668=CARTESIAN_POINT('Ctrl Pts',(6.99999594670264,14.8230891465946,4.89377001753077));
#43669=CARTESIAN_POINT('Ctrl Pts',(6.99999920776373,14.7967908123851,4.92966736373478));
#43670=CARTESIAN_POINT('Ctrl Pts',(6.99990231846403,14.6847031578439,4.95610625002928));
#43671=CARTESIAN_POINT('Ctrl Pts',(6.99990231846403,15.0109940548522,4.91841598752362));
#43672=CARTESIAN_POINT('Ctrl Pts',(6.99990231846403,15.8988757041253,4.85614479764408));
#43673=CARTESIAN_POINT('Ctrl Pts',(6.99990231846403,17.351727469812,4.9299863360756));
#43674=CARTESIAN_POINT('Ctrl Pts',(6.99990231846403,19.0057080032784,5.27368461013775));
#43675=CARTESIAN_POINT('Ctrl Pts',(6.99990231846403,20.590268079334,5.86659846405635));
#43676=CARTESIAN_POINT('Ctrl Pts',(6.99990231846403,22.0651422307797,6.69608016041579));
#43677=CARTESIAN_POINT('Ctrl Pts',(6.99990231846403,23.3944809544711,7.73956615459866));
#43678=CARTESIAN_POINT('Ctrl Pts',(6.99990231846403,24.2870583744167,8.6952955923328));
#43679=CARTESIAN_POINT('Ctrl Pts',(6.99990231846403,24.7366539504827,9.28611088916545));
#43680=CARTESIAN_POINT('Ctrl Pts',(6.99990231846403,24.8428619070666,9.43307698115495));
#43681=CARTESIAN_POINT('Ctrl Pts',(7.00658755380489,14.6298084473363,4.48100446307126));
#43682=CARTESIAN_POINT('Ctrl Pts',(7.00658755380489,14.9703697746716,4.44166427685036));
#43683=CARTESIAN_POINT('Ctrl Pts',(7.00658755380489,15.8968450849154,4.37670040150181));
#43684=CARTESIAN_POINT('Ctrl Pts',(7.00658755380489,17.4127705149432,4.45373854384782));
#43685=CARTESIAN_POINT('Ctrl Pts',(7.00658755380489,19.1391934374833,4.81245484156605));
#43686=CARTESIAN_POINT('Ctrl Pts',(7.00658755380489,20.7926967961888,5.43122447964866));
#43687=CARTESIAN_POINT('Ctrl Pts',(7.00658755380489,22.3317396202352,6.29673482166948));
#43688=CARTESIAN_POINT('Ctrl Pts',(7.00658755380489,23.7192732848802,7.38594521460744));
#43689=CARTESIAN_POINT('Ctrl Pts',(7.00658755380489,24.6505400754064,8.38311665741879));
#43690=CARTESIAN_POINT('Ctrl Pts',(7.00658755380489,25.1196657073454,8.99958310836095));
#43691=CARTESIAN_POINT('Ctrl Pts',(7.00658755380489,25.2304959439334,9.15294401871312));
#43692=CARTESIAN_POINT('Ctrl Pts',(6.71725767899343,14.5860721993496,4.10247674370146));
#43693=CARTESIAN_POINT('Ctrl Pts',(6.71725767899343,14.9380032028224,4.06182201420451));
#43694=CARTESIAN_POINT('Ctrl Pts',(6.71725767899343,15.8952272302191,3.99471279628271));
#43695=CARTESIAN_POINT('Ctrl Pts',(6.71725767899343,17.4614053239266,4.07429776800594));
#43696=CARTESIAN_POINT('Ctrl Pts',(6.71725767899343,19.2455452516906,4.44497937168528));
#43697=CARTESIAN_POINT('Ctrl Pts',(6.71725767899343,20.953977773508,5.08434908175678));
#43698=CARTESIAN_POINT('Ctrl Pts',(6.71725767899343,22.5441456868779,5.97856451697804));
#43699=CARTESIAN_POINT('Ctrl Pts',(6.71725767899343,23.9780449912323,7.10420489788168));
#43700=CARTESIAN_POINT('Ctrl Pts',(6.71725767899343,24.9401367536043,8.13439441828645));
#43701=CARTESIAN_POINT('Ctrl Pts',(6.71725767899343,25.4248225617206,8.77129790636529));
#43702=CARTESIAN_POINT('Ctrl Pts',(6.71725767899343,25.5393355062252,8.92975375864079));
#43703=CARTESIAN_POINT('Ctrl Pts',(6.25443113011109,14.5720960327223,3.98151605950182));
#43704=CARTESIAN_POINT('Ctrl Pts',(6.25443113011109,14.9276602808206,3.94044126022634));
#43705=CARTESIAN_POINT('Ctrl Pts',(6.25443113011109,15.8947102355587,3.87264648589394));
#43706=CARTESIAN_POINT('Ctrl Pts',(6.25443113011109,17.4769468535728,3.95304531142131));
#43707=CARTESIAN_POINT('Ctrl Pts',(6.25443113011109,19.2795305784078,4.32755049662825));
#43708=CARTESIAN_POINT('Ctrl Pts',(6.25443113011109,21.0055160264994,4.97350307678813));
#43709=CARTESIAN_POINT('Ctrl Pts',(6.25443113011109,22.6120212527427,5.8768913876941));
#43710=CARTESIAN_POINT('Ctrl Pts',(6.25443113011109,24.0607369607973,7.01417317831217));
#43711=CARTESIAN_POINT('Ctrl Pts',(6.25443113011109,25.0326790181266,8.05491381308084));
#43712=CARTESIAN_POINT('Ctrl Pts',(6.25443113011109,25.5223371689888,8.69834807253971));
#43713=CARTESIAN_POINT('Ctrl Pts',(6.25443113011109,25.6380269437365,8.85843204246403));
#43714=CARTESIAN_POINT('Ctrl Pts',(6.99999999975116,14.796790812404,4.92966736369432));
#43715=CARTESIAN_POINT('Ctrl Pts',(6.99999999975279,14.9628120942143,4.9122434544952));
#43716=CARTESIAN_POINT('Ctrl Pts',(6.99999999939315,15.1287094965253,4.89864382129396));
#43717=CARTESIAN_POINT('Ctrl Pts',(6.99999999870943,15.294561887614,4.88880665018259));
#43718=CARTESIAN_POINT('Ctrl Pts',(6.99999999819716,15.4188238238608,4.88143632575454));
#43719=CARTESIAN_POINT('Ctrl Pts',(6.99999999754782,15.5430607645851,4.87617913713079));
#43720=CARTESIAN_POINT('Ctrl Pts',(6.99999999746715,15.667307619498,4.87302815224969));
#43721=CARTESIAN_POINT('Ctrl Pts',(6.99999999735909,15.8337151132274,4.86880794484717));
#43722=CARTESIAN_POINT('Ctrl Pts',(6.99999999919074,16.0001407341898,4.86836394895551));
#43723=CARTESIAN_POINT('Ctrl Pts',(6.99999999987887,16.166701195129,4.87172626796587));
#43724=CARTESIAN_POINT('Ctrl Pts',(6.99999999995352,16.1847696360791,4.87209101156799));
#43725=CARTESIAN_POINT('Ctrl Pts',(6.99999999999963,16.2028396593029,4.8725005976837));
#43726=CARTESIAN_POINT('Ctrl Pts',(6.99999999999963,16.2209114099307,4.87295510148193));
#43727=CARTESIAN_POINT('Ctrl Pts',(6.99999999999963,16.4297965262892,4.8782085537198));
#43728=CARTESIAN_POINT('Ctrl Pts',(6.9999999954667,16.6388913988277,4.88938135116946));
#43729=CARTESIAN_POINT('Ctrl Pts',(6.99999999503575,16.8476333268867,4.90651885872368));
#43730=CARTESIAN_POINT('Ctrl Pts',(6.99999999469175,17.0142564616812,4.92019845466208));
#43731=CARTESIAN_POINT('Ctrl Pts',(6.9999999963588,17.1806544793605,4.93767756116664));
#43732=CARTESIAN_POINT('Ctrl Pts',(6.99999999805313,17.3465410238682,4.95895540149735));
#43733=CARTESIAN_POINT('Ctrl Pts',(6.99999999906359,17.4454726952585,4.97164511249072));
#43734=CARTESIAN_POINT('Ctrl Pts',(6.99999999999963,17.544222462615,4.98568551449838));
#43735=CARTESIAN_POINT('Ctrl Pts',(6.99999999999963,17.6427305436046,5.00106284970836));
#43736=CARTESIAN_POINT('Ctrl Pts',(6.99999999999963,17.9064996520793,5.04223780670992));
#43737=CARTESIAN_POINT('Ctrl Pts',(6.99999999769782,18.1685324379956,5.09308743825919));
#43738=CARTESIAN_POINT('Ctrl Pts',(6.99999999858912,18.4283218652711,5.15338940372302));
#43739=CARTESIAN_POINT('Ctrl Pts',(6.9999999992438,18.619142849646,5.19768250883596));
#43740=CARTESIAN_POINT('Ctrl Pts',(6.99999999995071,18.808753796749,5.24707643234085));
#43741=CARTESIAN_POINT('Ctrl Pts',(6.99999999999527,18.9969552178462,5.30150090629035));
#43742=CARTESIAN_POINT('Ctrl Pts',(6.99999999999829,19.0096808723613,5.30518093723065));
#43743=CARTESIAN_POINT('Ctrl Pts',(6.99999999999963,19.0224000823289,5.30888397401697));
#43744=CARTESIAN_POINT('Ctrl Pts',(6.99999999999963,19.0351127865529,5.3126099921686));
#43745=CARTESIAN_POINT('Ctrl Pts',(6.99999999999963,19.3842397982826,5.41493704705863));
#43746=CARTESIAN_POINT('Ctrl Pts',(6.99999999999433,19.7284570030457,5.53457218802795));
#43747=CARTESIAN_POINT('Ctrl Pts',(6.99999999997183,20.0659266389262,5.67102983958899));
#43748=CARTESIAN_POINT('Ctrl Pts',(6.9999999999649,20.169893191372,5.71306927093113));
#43749=CARTESIAN_POINT('Ctrl Pts',(6.99999999999963,20.2732191475457,5.75670501823988));
#43750=CARTESIAN_POINT('Ctrl Pts',(6.99999999999963,20.3758503571618,5.80192197800648));
#43751=CARTESIAN_POINT('Ctrl Pts',(6.99999999999963,20.4434628840057,5.83171050839074));
#43752=CARTESIAN_POINT('Ctrl Pts',(6.99999999997007,20.5107752122269,5.86218302328723));
#43753=CARTESIAN_POINT('Ctrl Pts',(6.99999999992877,20.5777722436876,5.89333439996507));
#43754=CARTESIAN_POINT('Ctrl Pts',(6.99999999970392,20.9425747082302,6.06295533298561));
#43755=CARTESIAN_POINT('Ctrl Pts',(6.99999999999963,21.2980259815938,6.25270726283353));
#43756=CARTESIAN_POINT('Ctrl Pts',(6.99999999999963,21.6419501727056,6.4612030800231));
#43757=CARTESIAN_POINT('Ctrl Pts',(6.99999999999963,21.7796572872,6.5446847254302));
#43758=CARTESIAN_POINT('Ctrl Pts',(6.9999999996197,21.9155159097578,6.63117290946998));
#43759=CARTESIAN_POINT('Ctrl Pts',(6.99999999912184,22.0494139576794,6.72060682878888));
#43760=CARTESIAN_POINT('Ctrl Pts',(6.99999999824605,22.2849549618095,6.8779306694769));
#43761=CARTESIAN_POINT('Ctrl Pts',(6.99999999886115,22.5144315343706,7.04436836788122));
#43762=CARTESIAN_POINT('Ctrl Pts',(6.99999999981795,22.7372440058527,7.21957770321878));
#43763=CARTESIAN_POINT('Ctrl Pts',(6.99999999992514,22.7622055678981,7.23920631137463));
#43764=CARTESIAN_POINT('Ctrl Pts',(6.99999999999963,22.7870834467616,7.25894503891287));
#43765=CARTESIAN_POINT('Ctrl Pts',(6.99999999999963,22.8118767647635,7.27879342661068));
#43766=CARTESIAN_POINT('Ctrl Pts',(6.99999999999963,22.9845622066237,7.41703743249722));
#43767=CARTESIAN_POINT('Ctrl Pts',(6.99999999634261,23.1531796781679,7.56056973529903));
#43768=CARTESIAN_POINT('Ctrl Pts',(6.99999999541923,23.3172464672391,7.70901269845457));
#43769=CARTESIAN_POINT('Ctrl Pts',(6.99999999530942,23.3367573752257,7.72666561292783));
#43770=CARTESIAN_POINT('Ctrl Pts',(6.99999999523431,23.3562039693901,7.7443879310535));
#43771=CARTESIAN_POINT('Ctrl Pts',(6.99999999519885,23.3755854729976,7.76217898327269));
#43772=CARTESIAN_POINT('Ctrl Pts',(6.99999999489031,23.5442323268772,7.91698663105599));
#43773=CARTESIAN_POINT('Ctrl Pts',(6.99999999999963,23.7079469955236,8.07700145659367));
#43774=CARTESIAN_POINT('Ctrl Pts',(6.99999999999963,23.8663282356994,8.24167851093918));
#43775=CARTESIAN_POINT('Ctrl Pts',(6.99999999999963,23.9843305537447,8.36437154024027));
#43776=CARTESIAN_POINT('Ctrl Pts',(6.9999999974146,24.0993266000013,8.48968650811308));
#43777=CARTESIAN_POINT('Ctrl Pts',(6.99999999745781,24.2114124198125,8.61766946000518));
#43778=CARTESIAN_POINT('Ctrl Pts',(6.99999999749905,24.318376059481,8.73980375293336));
#43779=CARTESIAN_POINT('Ctrl Pts',(6.99999999865126,24.4226893685616,8.86436824503144));
#43780=CARTESIAN_POINT('Ctrl Pts',(6.99999999924035,24.5244042559699,8.99143397814575));
#43781=CARTESIAN_POINT('Ctrl Pts',(6.99999999975839,24.6138515921833,9.10317466469306));
#43782=CARTESIAN_POINT('Ctrl Pts',(6.99999999990826,24.7012891768634,9.21685021183985));
#43783=CARTESIAN_POINT('Ctrl Pts',(6.9999999998936,24.7867157008319,9.33251047980519));
#43784=CARTESIAN_POINT('Ctrl Pts',(6.26386081936141,15.8144408559214,3.90572621533164));
#43785=CARTESIAN_POINT('Ctrl Pts',(6.2646071571378,16.0736401969478,3.90306654962963));
#43786=CARTESIAN_POINT('Ctrl Pts',(6.26531568508263,16.3306804620868,3.90881650033525));
#43787=CARTESIAN_POINT('Ctrl Pts',(6.26598638626061,16.5850686264647,3.92256316414692));
#43788=CARTESIAN_POINT('Ctrl Pts',(6.2666647366093,16.8423580210206,3.93646660504761));
#43789=CARTESIAN_POINT('Ctrl Pts',(6.26730439248674,17.0969345331479,3.95855018426228));
#43790=CARTESIAN_POINT('Ctrl Pts',(6.2679053397188,17.3483408478098,3.98839324939858));
#43791=CARTESIAN_POINT('Ctrl Pts',(6.26800176544167,17.3886805554093,3.99318175490248));
#43792=CARTESIAN_POINT('Ctrl Pts',(6.26809719457051,17.4289387505187,3.99817005148869));
#43793=CARTESIAN_POINT('Ctrl Pts',(6.26819162705404,17.4691136669068,4.00335641724054));
#43794=CARTESIAN_POINT('Ctrl Pts',(6.26876871455366,17.7146270875046,4.03505088012148));
#43795=CARTESIAN_POINT('Ctrl Pts',(6.26930858144218,17.9570264035881,4.07414071626594));
#43796=CARTESIAN_POINT('Ctrl Pts',(6.26981121749717,18.1959031194725,4.12010910859023));
#43797=CARTESIAN_POINT('Ctrl Pts',(6.27017912394857,18.37074987786,4.15375585543381));
#43798=CARTESIAN_POINT('Ctrl Pts',(6.27052708379087,18.5437104294303,4.19108825682538));
#43799=CARTESIAN_POINT('Ctrl Pts',(6.27085509380364,18.7146409206978,4.2319103480927));
#43800=CARTESIAN_POINT('Ctrl Pts',(6.27121137830344,18.9003056327786,4.27625130660444));
#43801=CARTESIAN_POINT('Ctrl Pts',(6.27154412415377,19.0835749911811,4.3247094130082));
#43802=CARTESIAN_POINT('Ctrl Pts',(6.27185332727448,19.2642823708993,4.37704091251744));
#43803=CARTESIAN_POINT('Ctrl Pts',(6.27227096880013,19.5083643374345,4.44772521623471));
#43804=CARTESIAN_POINT('Ctrl Pts',(6.27264565893848,19.7477705540641,4.5254749182099));
#43805=CARTESIAN_POINT('Ctrl Pts',(6.27297738975663,19.9821808854897,4.60968099294868));
#43806=CARTESIAN_POINT('Ctrl Pts',(6.27330912057479,20.2165912169153,4.69388706768746));
#43807=CARTESIAN_POINT('Ctrl Pts',(6.27359789209192,20.4460058483219,4.78454958019296));
#43808=CARTESIAN_POINT('Ctrl Pts',(6.27384369851774,20.6701561188015,4.88108731632356));
#43809=CARTESIAN_POINT('Ctrl Pts',(6.27395596467506,20.7725313494162,4.92517859927516));
#43810=CARTESIAN_POINT('Ctrl Pts',(6.274059268442,20.8738091329866,4.97049582165233));
#43811=CARTESIAN_POINT('Ctrl Pts',(6.27415361644308,20.9739672996456,5.01698549278479));
#43812=CARTESIAN_POINT('Ctrl Pts',(6.27415652008545,20.9770497549524,5.01841625313386));
#43813=CARTESIAN_POINT('Ctrl Pts',(6.27415941518457,20.9801311498554,5.01984812399059));
#43814=CARTESIAN_POINT('Ctrl Pts',(6.27416230174624,20.9832114837509,5.02128110381964));
#43815=CARTESIAN_POINT('Ctrl Pts',(6.27420631168368,21.0301757676948,5.04312901831916));
#43816=CARTESIAN_POINT('Ctrl Pts',(6.27424833704542,21.0768934073318,5.0652347129111));
#43817=CARTESIAN_POINT('Ctrl Pts',(6.27428839844132,21.1233627191961,5.08759195320009));
#43818=CARTESIAN_POINT('Ctrl Pts',(6.27431785052249,21.1575257310999,5.10402840632335));
#43819=CARTESIAN_POINT('Ctrl Pts',(6.2743467018383,21.1921534486782,5.12089383929234));
#43820=CARTESIAN_POINT('Ctrl Pts',(6.27437398824107,21.2260047646262,5.13758092935802));
#43821=CARTESIAN_POINT('Ctrl Pts',(6.27438625179811,21.2412188456975,5.14508074831611));
#43822=CARTESIAN_POINT('Ctrl Pts',(6.27439819925053,21.2562764111607,5.15254389876329));
#43823=CARTESIAN_POINT('Ctrl Pts',(6.27440974306803,21.2710663093239,5.15991218758797));
#43824=CARTESIAN_POINT('Ctrl Pts',(6.27456064722751,21.4644041849283,5.25623261471226));
#43825=CARTESIAN_POINT('Ctrl Pts',(6.27467736526253,21.6577059358034,5.35907904466896));
#43826=CARTESIAN_POINT('Ctrl Pts',(6.27475989543337,21.8504727943955,5.46870199605282));
#43827=CARTESIAN_POINT('Ctrl Pts',(6.27484107212138,22.0400783044643,5.57652714693292));
#43828=CARTESIAN_POINT('Ctrl Pts',(6.27488917310781,22.2291663735341,5.69090844126615));
#43829=CARTESIAN_POINT('Ctrl Pts',(6.27490419770935,22.4172141919104,5.81206904072998));
#43830=CARTESIAN_POINT('Ctrl Pts',(6.27490863155076,22.4727081231324,5.84782419083762));
#43831=CARTESIAN_POINT('Ctrl Pts',(6.2749101848683,22.5281111352571,5.88416962570433));
#43832=CARTESIAN_POINT('Ctrl Pts',(6.27490885766006,22.5834089609015,5.92111080776558));
#43833=CARTESIAN_POINT('Ctrl Pts',(6.27490450925621,22.7645842052217,6.04214319208507));
#43834=CARTESIAN_POINT('Ctrl Pts',(6.27486923980178,22.9446338346503,6.16957223798428));
#43835=CARTESIAN_POINT('Ctrl Pts',(6.2748030497645,23.1230233225777,6.30354224822262));
#43836=CARTESIAN_POINT('Ctrl Pts',(6.27475277111024,23.258529869426,6.40530728875025));
#43837=CARTESIAN_POINT('Ctrl Pts',(6.27468465104014,23.3930775980555,6.51084612431001));
#43838=CARTESIAN_POINT('Ctrl Pts',(6.27459869008054,23.5264138891986,6.62021363206385));
#43839=CARTESIAN_POINT('Ctrl Pts',(6.27448994557249,23.6950903378017,6.7585684838625));
#43840=CARTESIAN_POINT('Ctrl Pts',(6.27435264847565,23.8618295446342,6.90305124022513));
#43841=CARTESIAN_POINT('Ctrl Pts',(6.27418680127018,24.026082061508,7.05375519723077));
#43842=CARTESIAN_POINT('Ctrl Pts',(6.27401315139378,24.1980622234404,7.21154937550556));
#43843=CARTESIAN_POINT('Ctrl Pts',(6.27380820178873,24.3673155362908,7.37616474895342));
#43844=CARTESIAN_POINT('Ctrl Pts',(6.2735719562331,24.5332726200832,7.54763344678315));
#43845=CARTESIAN_POINT('Ctrl Pts',(6.27333930371878,24.6967056747693,7.71649428977333));
#43846=CARTESIAN_POINT('Ctrl Pts',(6.27307629996608,24.8569420194823,7.89200164036484));
#43847=CARTESIAN_POINT('Ctrl Pts',(6.2727829495743,25.0133992150722,8.07415384833901));
#43848=CARTESIAN_POINT('Ctrl Pts',(6.27261681774183,25.1020049280167,8.17731130422409));
#43849=CARTESIAN_POINT('Ctrl Pts',(6.27244095301194,25.1893978688721,8.28259933546736));
#43850=CARTESIAN_POINT('Ctrl Pts',(6.27225535637375,25.2754665765764,8.39001281171685));
#43851=CARTESIAN_POINT('Ctrl Pts',(6.27204648360049,25.3723293745519,8.51089727864247));
#43852=CARTESIAN_POINT('Ctrl Pts',(6.27182528484287,25.46751518399,8.63447390404182));
#43853=CARTESIAN_POINT('Ctrl Pts',(6.27159176169396,25.5608443101225,8.76072155999657));
#43854=CARTESIAN_POINT('Ctrl Pts',(-6.390310997207,15.4599632088997,3.94962478603215));
#43855=CARTESIAN_POINT('Ctrl Pts',(-4.260207331471,16.2180720984124,3.32898409023249));
#43856=CARTESIAN_POINT('Ctrl Pts',(0.0001535202166307,16.9761997022964,
2.70679304528151));
#43857=CARTESIAN_POINT('Ctrl Pts',(4.260514371904,16.2180174588604,3.32902893260671));
#43858=CARTESIAN_POINT('Ctrl Pts',(6.390771557857,15.4597992883758,3.9497589827666));
#43859=CARTESIAN_POINT('Ctrl Pts',(-6.390310997207,16.2401119443479,3.91822480441049));
#43860=CARTESIAN_POINT('Ctrl Pts',(-4.260207331471,16.9588864514405,3.34432399295645));
#43861=CARTESIAN_POINT('Ctrl Pts',(0.0001535202166307,17.6776685616714,
2.76847544297843));
#43862=CARTESIAN_POINT('Ctrl Pts',(4.260514371904,16.9588346475797,3.34436549534545));
#43863=CARTESIAN_POINT('Ctrl Pts',(6.390771557857,16.2399565288181,3.91834889490668));
#43864=CARTESIAN_POINT('Ctrl Pts',(-6.390310997207,18.1257229797427,4.02649557071453));
#43865=CARTESIAN_POINT('Ctrl Pts',(-4.260207331471,18.7393790303087,3.53810403696184));
#43866=CARTESIAN_POINT('Ctrl Pts',(0.0001535202166307,19.3530131910523,
3.05102600446442));
#43867=CARTESIAN_POINT('Ctrl Pts',(4.260514371904,18.7393348046511,3.53813914151219));
#43868=CARTESIAN_POINT('Ctrl Pts',(6.390771557857,18.125590293236,4.02660117217093));
#43869=CARTESIAN_POINT('Ctrl Pts',(-6.390310997207,21.0044951210711,4.89945800148705));
#43870=CARTESIAN_POINT('Ctrl Pts',(-4.260207331471,21.442483951078,4.44478850538388));
#43871=CARTESIAN_POINT('Ctrl Pts',(0.0001535202166307,21.8807678511965,
3.98943347064864));
#43872=CARTESIAN_POINT('Ctrl Pts',(4.260514371904,21.4424523632066,4.44482132360082));
#43873=CARTESIAN_POINT('Ctrl Pts',(6.390771557857,21.0044004178526,4.89955631145292));
#43874=CARTESIAN_POINT('Ctrl Pts',(-6.390310997207,23.7052293934154,6.63374483550749));
#43875=CARTESIAN_POINT('Ctrl Pts',(-4.260207331471,23.9981328584314,6.09525951521535));
#43876=CARTESIAN_POINT('Ctrl Pts',(0.000153520216631,24.2900557545739,5.55782195886724));
#43877=CARTESIAN_POINT('Ctrl Pts',(4.260514371904,23.9981118190468,6.09529824925896));
#43878=CARTESIAN_POINT('Ctrl Pts',(6.390771557857,23.7051660609652,6.63386126838838));
#43879=CARTESIAN_POINT('Ctrl Pts',(-6.390310997207,25.1149841603859,8.1839487906061));
#43880=CARTESIAN_POINT('Ctrl Pts',(-4.260207331471,25.3660581844935,7.53598959785924));
#43881=CARTESIAN_POINT('Ctrl Pts',(0.0001535202166303,25.6190363056788,
6.88615830217486));
#43882=CARTESIAN_POINT('Ctrl Pts',(4.260514371904,25.3660399519323,7.53603643231476));
#43883=CARTESIAN_POINT('Ctrl Pts',(6.390771557857,25.1149298724386,8.18408889422398));
#43884=CARTESIAN_POINT('Ctrl Pts',(-6.390310997207,25.680737599168,8.98426054544063));
#43885=CARTESIAN_POINT('Ctrl Pts',(-4.260207331471,25.9287994959116,8.27687328339766));
#43886=CARTESIAN_POINT('Ctrl Pts',(0.0001535202166303,26.1774666691521,
7.56887710148171));
#43887=CARTESIAN_POINT('Ctrl Pts',(4.260514371904,25.9287815740455,8.27692430989529));
#43888=CARTESIAN_POINT('Ctrl Pts',(6.390771557857,25.6806839625015,8.98441349877858));
#43889=CARTESIAN_POINT('Ctrl Pts',(-6.26386059984685,15.8144217559904,3.90573753014116));
#43890=CARTESIAN_POINT('Ctrl Pts',(-5.97539333098954,15.9103760885445,3.82576732795924));
#43891=CARTESIAN_POINT('Ctrl Pts',(-5.68507999445153,15.9990640254287,3.75075426795588));
#43892=CARTESIAN_POINT('Ctrl Pts',(-5.39340845737568,16.0805744084132,3.68097248655366));
#43893=CARTESIAN_POINT('Ctrl Pts',(-5.11949030830525,16.1571234383974,3.61543816465115));
#43894=CARTESIAN_POINT('Ctrl Pts',(-4.84437426792527,16.2273417544319,3.55451825621326));
#43895=CARTESIAN_POINT('Ctrl Pts',(-4.5684644297166,16.2913404726591,3.49841824263205));
#43896=CARTESIAN_POINT('Ctrl Pts',(-4.31194165949948,16.3508422598971,3.44626015002287));
#43897=CARTESIAN_POINT('Ctrl Pts',(-4.05473272615563,16.4049677060134,3.39826866251004));
#43898=CARTESIAN_POINT('Ctrl Pts',(-3.79716238633167,16.453842265351,3.35458408540851));
#43899=CARTESIAN_POINT('Ctrl Pts',(-3.57726994290746,16.4955673579271,3.31728977424918));
#43900=CARTESIAN_POINT('Ctrl Pts',(-3.35711409398038,16.5334658330865,3.28313426378421));
#43901=CARTESIAN_POINT('Ctrl Pts',(-3.13689690935008,16.5676399602686,3.25218673091632));
#43902=CARTESIAN_POINT('Ctrl Pts',(-2.89863169006324,16.6046148490387,3.21870287397966));
#43903=CARTESIAN_POINT('Ctrl Pts',(-2.6602852319021,16.6372510250138,3.18897493478523));
#43904=CARTESIAN_POINT('Ctrl Pts',(-2.42210555319733,16.6655736606144,3.16305553873815));
#43905=CARTESIAN_POINT('Ctrl Pts',(-2.18716847768624,16.6935107088753,3.13748901207462));
#43906=CARTESIAN_POINT('Ctrl Pts',(-1.95239367143694,16.7172508562373,3.11562807350144));
#43907=CARTESIAN_POINT('Ctrl Pts',(-1.71801916041739,16.7368573333217,3.09749090364961));
#43908=CARTESIAN_POINT('Ctrl Pts',(-1.48507356908385,16.7563442748775,3.07946431134709));
#43909=CARTESIAN_POINT('Ctrl Pts',(-1.25252340686986,16.7717477586243,3.06511627751505));
#43910=CARTESIAN_POINT('Ctrl Pts',(-1.02060237268687,16.7831691638654,3.05443172704252));
#43911=CARTESIAN_POINT('Ctrl Pts',(-0.790162778168551,16.7945176127108,
3.04381542616591));
#43912=CARTESIAN_POINT('Ctrl Pts',(-0.560344300001652,16.8019346801216,
3.03681598687228));
#43913=CARTESIAN_POINT('Ctrl Pts',(-0.331376187254698,16.8055591055299,
3.03338536086241));
#43914=CARTESIAN_POINT('Ctrl Pts',(-0.220817153790872,16.8073091875182,
3.03172885642048));
#43915=CARTESIAN_POINT('Ctrl Pts',(-0.110456384411538,16.8081755976358,
3.0309039262618));
#43916=CARTESIAN_POINT('Ctrl Pts',(-0.000319687765395044,16.8081772730686,
3.03090233350032));
#43917=CARTESIAN_POINT('Ctrl Pts',(-0.000213125382396117,16.8081772746896,
3.03090233195925));
#43918=CARTESIAN_POINT('Ctrl Pts',(-0.000106562793408779,16.8081772755014,
3.03090233118879));
#43919=CARTESIAN_POINT('Ctrl Pts',(1.54364816055824E-12,16.8081772755037,
3.03090233118895));
#43920=CARTESIAN_POINT('Ctrl Pts',(0.229814767883462,16.8081772805917,3.03090233154421));
#43921=CARTESIAN_POINT('Ctrl Pts',(0.460587477671531,16.8044096604372,3.03448931169225));
#43922=CARTESIAN_POINT('Ctrl Pts',(0.692092742459731,16.7967144780101,3.04172791113162));
#43923=CARTESIAN_POINT('Ctrl Pts',(0.92542107169346,16.7889586973348,3.04902351330604));
#43924=CARTESIAN_POINT('Ctrl Pts',(1.15949353884638,16.7772132495556,3.06002845784822));
#43925=CARTESIAN_POINT('Ctrl Pts',(1.39407939032145,16.7613548321441,3.07477450403601));
#43926=CARTESIAN_POINT('Ctrl Pts',(1.63013438285027,16.7453970982055,3.08961290030245));
#43927=CARTESIAN_POINT('Ctrl Pts',(1.86670921018194,16.7252747476301,3.10823935315465));
#43928=CARTESIAN_POINT('Ctrl Pts',(2.10356875608892,16.7009027147165,3.13065201869609));
#43929=CARTESIAN_POINT('Ctrl Pts',(2.34326327402721,16.6762389729281,3.15333294144335));
#43930=CARTESIAN_POINT('Ctrl Pts',(2.5832493669223,16.647223228046,3.17989120946434));
#43931=CARTESIAN_POINT('Ctrl Pts',(2.82328337477861,16.6138084331694,3.21029066606775));
#43932=CARTESIAN_POINT('Ctrl Pts',(2.92752592620592,16.599296974962,3.22349261585247));
#43933=CARTESIAN_POINT('Ctrl Pts',(3.03177751445368,16.5839563689886,3.23741858935517));
#43934=CARTESIAN_POINT('Ctrl Pts',(3.13601818225799,16.567785112841,3.2520636894151));
#43935=CARTESIAN_POINT('Ctrl Pts',(3.39880739691305,16.5270176101711,3.28898377467892));
#43936=CARTESIAN_POINT('Ctrl Pts',(3.66152138150451,16.4809439402936,3.33047470854717));
#43937=CARTESIAN_POINT('Ctrl Pts',(3.92381607763906,16.4293925584389,3.37641707163315));
#43938=CARTESIAN_POINT('Ctrl Pts',(4.19336645804413,16.3764151448881,3.42363030784813));
#43939=CARTESIAN_POINT('Ctrl Pts',(4.46247403215353,16.3176531431208,3.47554420302421));
#43940=CARTESIAN_POINT('Ctrl Pts',(4.73076539208801,16.2529691538375,3.53199295300502));
#43941=CARTESIAN_POINT('Ctrl Pts',(5.02425998648815,16.182208764075,3.59374448680043));
#43942=CARTESIAN_POINT('Ctrl Pts',(5.31677781390168,16.1043615550116,3.66092253642902));
#43943=CARTESIAN_POINT('Ctrl Pts',(5.60783003770296,16.0193026037346,3.73327326415423));
#43944=CARTESIAN_POINT('Ctrl Pts',(5.82741016918173,15.9551311108633,3.78785722197113));
#43945=CARTESIAN_POINT('Ctrl Pts',(6.04615611875628,15.886856153891,3.84538443185739));
#43946=CARTESIAN_POINT('Ctrl Pts',(6.26385797789322,15.8144409706466,3.9057366018783));
#43947=CARTESIAN_POINT('Ctrl Pts',(-6.38267922172612,15.7738523078598,3.93899334286503));
#43948=CARTESIAN_POINT('Ctrl Pts',(-6.32178394100786,15.7957619893123,3.92177794388969));
#43949=CARTESIAN_POINT('Ctrl Pts',(-5.68007566712876,16.0226513783196,3.74296990775899));
#43950=CARTESIAN_POINT('Ctrl Pts',(-4.3405628786162,16.4113546400769,3.42585487548982));
#43951=CARTESIAN_POINT('Ctrl Pts',(-2.26159155672449,16.7779842233051,3.11137634163404));
#43952=CARTESIAN_POINT('Ctrl Pts',(-0.000322645265903455,16.9116027729772,
2.99296782877783));
#43953=CARTESIAN_POINT('Ctrl Pts',(2.26104630018457,16.7780550953811,3.11131422928351));
#43954=CARTESIAN_POINT('Ctrl Pts',(4.34024112533146,16.4114385643274,3.42578519270288));
#43955=CARTESIAN_POINT('Ctrl Pts',(5.67995509241135,16.0226928958199,3.74293703686325));
#43956=CARTESIAN_POINT('Ctrl Pts',(6.32176875644207,15.7957675033798,3.92177361735684));
#43957=CARTESIAN_POINT('Ctrl Pts',(6.38269140808456,15.7738479232639,3.93899678720638));
#43958=CARTESIAN_POINT('Ctrl Pts',(-6.17947932752834,15.1606870779192,3.89075783424522));
#43959=CARTESIAN_POINT('Ctrl Pts',(-6.12049144092706,15.1819034727368,3.87432042702319));
#43960=CARTESIAN_POINT('Ctrl Pts',(-5.49889172536448,15.4016154015587,3.70358699318366));
#43961=CARTESIAN_POINT('Ctrl Pts',(-4.20155201647089,15.7780515103907,3.40068046498789));
#43962=CARTESIAN_POINT('Ctrl Pts',(-2.18881221307725,16.1330771577479,3.10022483933076));
#43963=CARTESIAN_POINT('Ctrl Pts',(-0.000312236874671785,16.2624448571322,
2.98709891979729));
#43964=CARTESIAN_POINT('Ctrl Pts',(2.18828441451265,16.1331457801785,3.10016549602611));
#43965=CARTESIAN_POINT('Ctrl Pts',(4.2012404201408,15.7781327862976,3.40061389543627));
#43966=CARTESIAN_POINT('Ctrl Pts',(5.49877493126362,15.4016556064113,3.70355560477545));
#43967=CARTESIAN_POINT('Ctrl Pts',(6.12047673185723,15.18190881228,3.87431629610783));
#43968=CARTESIAN_POINT('Ctrl Pts',(6.17949113217087,15.1606828320346,3.89076112296309));
#43969=CARTESIAN_POINT('Ctrl Pts',(-6.17606942198722,14.7511100720048,3.39035617507167));
#43970=CARTESIAN_POINT('Ctrl Pts',(-6.11724876379497,14.7720723442377,3.37412570862358));
#43971=CARTESIAN_POINT('Ctrl Pts',(-5.49737410508965,14.9891714302522,3.20552395379427));
#43972=CARTESIAN_POINT('Ctrl Pts',(-4.20278204043645,15.3615316584505,2.90602013925078));
#43973=CARTESIAN_POINT('Ctrl Pts',(-2.19095873851463,15.7134382585734,2.60822212402352));
#43974=CARTESIAN_POINT('Ctrl Pts',(-0.000312652823461832,15.841880384075,
2.4958818195532));
#43975=CARTESIAN_POINT('Ctrl Pts',(2.19043080442953,15.7135063490568,2.6081632346203));
#43976=CARTESIAN_POINT('Ctrl Pts',(4.20247098821445,15.3616121052018,2.90595426953607));
#43977=CARTESIAN_POINT('Ctrl Pts',(5.49725762526239,14.9892111622839,3.20549295254849));
#43978=CARTESIAN_POINT('Ctrl Pts',(6.11723409695662,14.77207761954,3.37412162987566));
#43979=CARTESIAN_POINT('Ctrl Pts',(6.17608119319573,14.7511058769368,3.39035942228679));
#43980=CARTESIAN_POINT('Ctrl Pts',(-6.37318055258469,14.8203254139217,2.77953975667807));
#43981=CARTESIAN_POINT('Ctrl Pts',(-6.31268764295094,14.8416410144565,2.76280981911965));
#43982=CARTESIAN_POINT('Ctrl Pts',(-5.67513346514493,15.0624217826566,2.58900295618313));
#43983=CARTESIAN_POINT('Ctrl Pts',(-4.34231715275912,15.4415875234496,2.27988148674971));
#43984=CARTESIAN_POINT('Ctrl Pts',(-2.26599033350655,15.800901109489,1.97166918135384));
#43985=CARTESIAN_POINT('Ctrl Pts',(-0.000323526748717448,15.9323422860991,
1.85512198255444));
#43986=CARTESIAN_POINT('Ctrl Pts',(2.2654449005586,15.8009707317227,1.97160814218462));
#43987=CARTESIAN_POINT('Ctrl Pts',(4.3419967397778,15.4416695062744,2.27981344950243));
#43988=CARTESIAN_POINT('Ctrl Pts',(5.67501364814971,15.0624621946197,2.58897099373883));
#43989=CARTESIAN_POINT('Ctrl Pts',(6.31267255995101,14.8416463783418,2.76280561495848));
#43990=CARTESIAN_POINT('Ctrl Pts',(6.37319265849431,14.8203211481087,2.7795431036554));
#43991=CARTESIAN_POINT('Ctrl Pts',(-6.24994620506134,14.8593873451939,2.76546786777471));
#43992=CARTESIAN_POINT('Ctrl Pts',(-6.22850662278677,14.8667761577535,2.75964861829393));
#43993=CARTESIAN_POINT('Ctrl Pts',(-6.20704358783532,14.8741272855027,2.7538527902599));
#43994=CARTESIAN_POINT('Ctrl Pts',(-6.18555718293149,14.8814406700516,2.74808058402306));
#43995=CARTESIAN_POINT('Ctrl Pts',(-5.88365929671791,14.9841984532296,2.6669773529572));
#43996=CARTESIAN_POINT('Ctrl Pts',(-5.5771472884225,15.0795079506171,2.59053465810836));
#43997=CARTESIAN_POINT('Ctrl Pts',(-5.26630871828218,15.1671888464119,2.51936495347675));
#43998=CARTESIAN_POINT('Ctrl Pts',(-5.13424536371906,15.2044410870992,2.48912768294538));
#43999=CARTESIAN_POINT('Ctrl Pts',(-5.00140109970354,15.2403158616087,2.45984266059681));
#44000=CARTESIAN_POINT('Ctrl Pts',(-4.86779840574354,15.274797334949,2.43155887951409));
#44001=CARTESIAN_POINT('Ctrl Pts',(-4.71600682495683,15.3139731718355,2.39942449873238));
#44002=CARTESIAN_POINT('Ctrl Pts',(-4.56323915278791,15.3513507651254,2.36857718708611));
#44003=CARTESIAN_POINT('Ctrl Pts',(-4.40952973635834,15.3869070844585,2.33907600634009));
#44004=CARTESIAN_POINT('Ctrl Pts',(-4.32504469211605,15.4064503062189,2.32286093885482));
#44005=CARTESIAN_POINT('Ctrl Pts',(-4.24027512903501,15.4254432749396,2.30705258251815));
#44006=CARTESIAN_POINT('Ctrl Pts',(-4.15522924912161,15.4438822756036,2.29165974001541));
#44007=CARTESIAN_POINT('Ctrl Pts',(-4.03534141761238,15.4698754431393,2.26996069345026));
#44008=CARTESIAN_POINT('Ctrl Pts',(-3.91490275773383,15.4947680749842,2.24908777917226));
#44009=CARTESIAN_POINT('Ctrl Pts',(-3.79393281020035,15.5185497764201,2.22906479297264));
#44010=CARTESIAN_POINT('Ctrl Pts',(-3.73344783643362,15.530440627138,2.21905329987282));
#44011=CARTESIAN_POINT('Ctrl Pts',(-3.67283003770224,15.5420537317391,2.20925428665817));
#44012=CARTESIAN_POINT('Ctrl Pts',(-3.61208195660669,15.5533877223801,2.19967049112853));
#44013=CARTESIAN_POINT('Ctrl Pts',(-3.58170791605892,15.5590547177007,2.19487859336371));
#44014=CARTESIAN_POINT('Ctrl Pts',(-3.55130130475809,15.5646519336992,2.1901404998973));
#44015=CARTESIAN_POINT('Ctrl Pts',(-3.52086244284463,15.5701791947916,2.18545654570334));
#44016=CARTESIAN_POINT('Ctrl Pts',(-3.5056430118879,15.5729428253378,2.18311456860636));
#44017=CARTESIAN_POINT('Ctrl Pts',(-3.49041551826924,15.5756889671052,2.18078612632016));
#44018=CARTESIAN_POINT('Ctrl Pts',(-3.47518000234777,15.578417597879,2.17847125990129));
#44019=CARTESIAN_POINT('Ctrl Pts',(-3.46756224438704,15.5797819132659,2.17731382669186));
#44020=CARTESIAN_POINT('Ctrl Pts',(-3.45994248085009,15.5811418509012,2.17615978744881));
#44021=CARTESIAN_POINT('Ctrl Pts',(-3.45232071680447,15.5824974079916,2.17500914725054));
#44022=CARTESIAN_POINT('Ctrl Pts',(-3.44469895275884,15.583852965082,2.17385850705228));
#44023=CARTESIAN_POINT('Ctrl Pts',(-3.43823529095624,15.5849992547046,2.17288527721797));
#44024=CARTESIAN_POINT('Ctrl Pts',(-3.42944942821482,15.586550934823,2.17156742885132));
#44025=CARTESIAN_POINT('Ctrl Pts',(-3.13033149385742,15.6393784561986,2.12670079562151));
#44026=CARTESIAN_POINT('Ctrl Pts',(-2.82949174433291,15.6852093579706,2.08740015843555));
#44027=CARTESIAN_POINT('Ctrl Pts',(-2.52723878681692,15.7240366908818,2.0539476436804));
#44028=CARTESIAN_POINT('Ctrl Pts',(-2.45239387379483,15.7336512481007,2.04566401735034));
#44029=CARTESIAN_POINT('Ctrl Pts',(-2.37746220520499,15.7428361780922,2.03773911348895));
#44030=CARTESIAN_POINT('Ctrl Pts',(-2.30244828060811,15.7515910036884,2.03017748529987));
#44031=CARTESIAN_POINT('Ctrl Pts',(-2.00299346058271,15.7865401779562,1.99999154288147));
#44032=CARTESIAN_POINT('Ctrl Pts',(-1.70222881863287,15.814638248534,1.97559222184925));
#44033=CARTESIAN_POINT('Ctrl Pts',(-1.40053607615597,15.8358823134265,1.95708487572244));
#44034=CARTESIAN_POINT('Ctrl Pts',(-1.10085973549657,15.8569843909093,1.93870122579747));
#44035=CARTESIAN_POINT('Ctrl Pts',(-0.800267108626436,15.871323783777,1.92613092772216));
#44036=CARTESIAN_POINT('Ctrl Pts',(-0.49912433318855,15.8788593394164,1.91951016285445));
#44037=CARTESIAN_POINT('Ctrl Pts',(-0.333015939771273,15.8830159028237,
1.91585819207822));
#44038=CARTESIAN_POINT('Ctrl Pts',(-0.166740066804234,15.8851016845639,
1.91401699144391));
#44039=CARTESIAN_POINT('Ctrl Pts',(-0.000358043406942927,15.8851047148172,
1.91401397084702));
#44040=CARTESIAN_POINT('Ctrl Pts',(-0.000345565863738448,15.8851047150445,
1.9140139706205));
#44041=CARTESIAN_POINT('Ctrl Pts',(-0.000333088319937549,15.88510471526,
1.91401397040431));
#44042=CARTESIAN_POINT('Ctrl Pts',(-0.000320610775539605,15.8851047154638,
1.91401397019847));
#44043=CARTESIAN_POINT('Ctrl Pts',(0.29646157639871,15.8851095633514,1.91400907409693));
#44044=CARTESIAN_POINT('Ctrl Pts',(0.592899678854785,15.878495752609,1.91980212803821));
#44045=CARTESIAN_POINT('Ctrl Pts',(0.888657766029018,15.8653161400331,1.93130344475154));
#44046=CARTESIAN_POINT('Ctrl Pts',(1.16839169566267,15.8528505981704,1.94218162073286));
#44047=CARTESIAN_POINT('Ctrl Pts',(1.44751760548253,15.8345110681381,1.95816672185245));
#44048=CARTESIAN_POINT('Ctrl Pts',(1.72573998854356,15.8103111796674,1.97921018196904));
#44049=CARTESIAN_POINT('Ctrl Pts',(1.91823927201675,15.7935675189328,1.99376994150266));
#44050=CARTESIAN_POINT('Ctrl Pts',(2.11031101581594,15.7740195872836,2.01073408711409));
#44051=CARTESIAN_POINT('Ctrl Pts',(2.30185594488252,15.7516674948778,2.03006063174667));
#44052=CARTESIAN_POINT('Ctrl Pts',(2.39508333324716,15.7407884431084,2.03946711037802));
#44053=CARTESIAN_POINT('Ctrl Pts',(2.48818591806944,15.7292450158588,2.04943330100437));
#44054=CARTESIAN_POINT('Ctrl Pts',(2.58115534057936,15.7170382210193,2.05994866323696));
#44055=CARTESIAN_POINT('Ctrl Pts',(2.7231475081323,15.6983947873899,2.07600877241801));
#44056=CARTESIAN_POINT('Ctrl Pts',(2.86482602552771,15.6782037050381,2.09335491489588));
#44057=CARTESIAN_POINT('Ctrl Pts',(3.00615411766162,15.6564670213138,2.11195842960335));
#44058=CARTESIAN_POINT('Ctrl Pts',(3.07681816372858,15.6455986794516,2.12126018695709));
#44059=CARTESIAN_POINT('Ctrl Pts',(3.14739460189104,15.6343439150781,2.13087628464253));
#44060=CARTESIAN_POINT('Ctrl Pts',(3.21787891819181,15.6227029013609,2.14080264019682));
#44061=CARTESIAN_POINT('Ctrl Pts',(3.25312107634219,15.6168823945023,2.14576581797396));
#44062=CARTESIAN_POINT('Ctrl Pts',(3.28834020388962,15.6109653238857,2.15080656003985));
#44063=CARTESIAN_POINT('Ctrl Pts',(3.3235357385418,15.6049517039844,2.15592434168264));
#44064=CARTESIAN_POINT('Ctrl Pts',(3.34113350586789,15.6019448940338,2.15848323250403));
#44065=CARTESIAN_POINT('Ctrl Pts',(3.35872537495863,15.5989139466725,2.16106138320784));
#44066=CARTESIAN_POINT('Ctrl Pts',(3.37631127579107,15.595858863346,2.16365872650413));
#44067=CARTESIAN_POINT('Ctrl Pts',(3.38510422620729,15.5943313216828,2.16495739815227));
#44068=CARTESIAN_POINT('Ctrl Pts',(3.39389568455815,15.5927977460227,2.16626086794778));
#44069=CARTESIAN_POINT('Ctrl Pts',(3.40268564210845,15.5912581365241,2.16756912736822));
#44070=CARTESIAN_POINT('Ctrl Pts',(3.41147559965875,15.5897185270255,2.16887738678867));
#44071=CARTESIAN_POINT('Ctrl Pts',(3.42142413678522,15.5879680264099,2.17036441991536));
#44072=CARTESIAN_POINT('Ctrl Pts',(3.42905100362602,15.586621206652,2.17150826594686));
#44073=CARTESIAN_POINT('Ctrl Pts',(3.74300305951125,15.5311807694804,2.21859350038224));
#44074=CARTESIAN_POINT('Ctrl Pts',(4.05359391333256,15.468300785322,2.27151445346201));
#44075=CARTESIAN_POINT('Ctrl Pts',(4.36044446898295,15.398179554136,2.32979150920995));
#44076=CARTESIAN_POINT('Ctrl Pts',(4.37670544692025,15.3944636091189,2.33287979404541));
#44077=CARTESIAN_POINT('Ctrl Pts',(4.39295592218156,15.3907273205417,2.33598312911675));
#44078=CARTESIAN_POINT('Ctrl Pts',(4.40919583866862,15.3869707151934,2.33910144596573));
#44079=CARTESIAN_POINT('Ctrl Pts',(4.72500831061156,15.3139172101386,2.39974235832286));
#44080=CARTESIAN_POINT('Ctrl Pts',(5.0368280494556,15.233183625842,2.46604569521785));
#44081=CARTESIAN_POINT('Ctrl Pts',(5.34437472290267,15.1449662897124,2.53746220440449));
#44082=CARTESIAN_POINT('Ctrl Pts',(5.62846729561695,15.0634765772789,2.60343235326581));
#44083=CARTESIAN_POINT('Ctrl Pts',(5.90891387849274,14.9756005513054,2.67376622484032));
#44084=CARTESIAN_POINT('Ctrl Pts',(6.18548847091395,14.8814648070078,2.74805806744846));
#44085=CARTESIAN_POINT('Ctrl Pts',(6.20699738299684,14.8741439702301,2.75383566508368));
#44086=CARTESIAN_POINT('Ctrl Pts',(6.22848287378777,14.8667852614923,2.75963721232427));
#44087=CARTESIAN_POINT('Ctrl Pts',(6.24994485533833,14.8593887340788,2.76546253801171));
#44088=CARTESIAN_POINT('Ctrl Pts',(7.10864015771174,15.2168666636805,-5.10578634035435));
#44089=CARTESIAN_POINT('Ctrl Pts',(7.1087319511891,15.2180649748934,-5.10211992456215));
#44090=CARTESIAN_POINT('Ctrl Pts',(7.11056295212648,15.2469376143842,-5.01406836458424));
#44091=CARTESIAN_POINT('Ctrl Pts',(7.0957532833273,15.3118408147158,-4.83046555613198));
#44092=CARTESIAN_POINT('Ctrl Pts',(7.0156532801071,15.4217311620991,-4.56064291735805));
#44093=CARTESIAN_POINT('Ctrl Pts',(6.86753478365422,15.544577900644,-4.30331374819862));
#44094=CARTESIAN_POINT('Ctrl Pts',(6.6575660839203,15.6691709072268,-4.08925365825966));
#44095=CARTESIAN_POINT('Ctrl Pts',(6.43827728684127,15.7687690204722,-3.96037917188944));
#44096=CARTESIAN_POINT('Ctrl Pts',(6.29372110804464,15.8227148621946,-3.91249915664003));
#44097=CARTESIAN_POINT('Ctrl Pts',(6.24006896070876,15.8413292732832,-3.89922637230209));
#44098=CARTESIAN_POINT('Ctrl Pts',(6.81411419638977,14.6698658120206,-4.91911214345852));
#44099=CARTESIAN_POINT('Ctrl Pts',(6.81419627724694,14.6709155403628,-4.91589643867816));
#44100=CARTESIAN_POINT('Ctrl Pts',(6.81583363952186,14.6962160679811,-4.83866110954873));
#44101=CARTESIAN_POINT('Ctrl Pts',(6.80258371972187,14.7534790973455,-4.67723688479289));
#44102=CARTESIAN_POINT('Ctrl Pts',(6.73069215177584,14.8512303729355,-4.43987215280684));
#44103=CARTESIAN_POINT('Ctrl Pts',(6.59792592232803,14.9609312319686,-4.21412828271034));
#44104=CARTESIAN_POINT('Ctrl Pts',(6.41046232976571,15.0721874407856,-4.02740669878977));
#44105=CARTESIAN_POINT('Ctrl Pts',(6.21582985009401,15.1607955045741,-3.91592435843964));
#44106=CARTESIAN_POINT('Ctrl Pts',(6.08830244040965,15.2085177762748,-3.87484710507141));
#44107=CARTESIAN_POINT('Ctrl Pts',(6.04108479571608,15.2249435030192,-3.86349736250906));
#44108=CARTESIAN_POINT('Ctrl Pts',(7.05418145170486,14.0948107036104,-4.73681539781006));
#44109=CARTESIAN_POINT('Ctrl Pts',(7.05428926420662,14.0961709987801,-4.73265407124799));
#44110=CARTESIAN_POINT('Ctrl Pts',(7.05643951699901,14.128938155199,-4.63273942242313));
#44111=CARTESIAN_POINT('Ctrl Pts',(7.03906591768119,14.2021863569183,-4.42547524588522));
#44112=CARTESIAN_POINT('Ctrl Pts',(6.94574281226092,14.3258056483014,-4.12160094983398));
#44113=CARTESIAN_POINT('Ctrl Pts',(6.77268165673607,14.4645602505892,-3.83060449371117));
#44114=CARTESIAN_POINT('Ctrl Pts',(6.52525480627982,14.6068210786327,-3.5862501007206));
#44115=CARTESIAN_POINT('Ctrl Pts',(6.26358456623248,14.7225229339098,-3.43716301885407));
#44116=CARTESIAN_POINT('Ctrl Pts',(6.08889668303178,14.7863755199405,-3.38117016334174));
#44117=CARTESIAN_POINT('Ctrl Pts',(6.0237377980366,14.8085815309694,-3.36561061007094));
#44118=CARTESIAN_POINT('Ctrl Pts',(7.66687013418301,13.8848570640408,-4.68358416887574));
#44119=CARTESIAN_POINT('Ctrl Pts',(7.66702167141007,13.8867765789514,-4.67772182071597));
#44120=CARTESIAN_POINT('Ctrl Pts',(7.67004350207725,13.9329883534776,-4.53700409028155));
#44121=CARTESIAN_POINT('Ctrl Pts',(7.64565945806534,14.0350125684346,-4.24694992517504));
#44122=CARTESIAN_POINT('Ctrl Pts',(7.51579920588202,14.2049730951923,-3.82267498432891));
#44123=CARTESIAN_POINT('Ctrl Pts',(7.27412333436781,14.3952858296309,-3.41381360895691));
#44124=CARTESIAN_POINT('Ctrl Pts',(6.92493243269211,14.5918721258049,-3.06591857353932));
#44125=CARTESIAN_POINT('Ctrl Pts',(6.54999799178159,14.7543797728273,-2.84972017330276));
#44126=CARTESIAN_POINT('Ctrl Pts',(6.29594778184491,14.8457775466123,-2.76720426236357));
#44127=CARTESIAN_POINT('Ctrl Pts',(6.20064104407826,14.8778126539731,-2.74415575802351));
#44128=CARTESIAN_POINT('',(6.26385988960052,15.8144313888753,-3.90573722891367));
#44129=CARTESIAN_POINT('',(6.24994527935227,14.8593853006947,-2.7654652932868));
#44130=CARTESIAN_POINT('Ctrl Pts',(6.26385592206845,15.8144315483309,-3.90575173238593));
#44131=CARTESIAN_POINT('Ctrl Pts',(6.25433095299875,15.7850306577855,-3.90346957258091));
#44132=CARTESIAN_POINT('Ctrl Pts',(6.24498623106511,15.7550023461302,-3.89974836247239));
#44133=CARTESIAN_POINT('Ctrl Pts',(6.23592367023207,15.7245194976627,-3.8944382562731));
#44134=CARTESIAN_POINT('Ctrl Pts',(6.22708767499122,15.6947987256923,-3.88926090364951));
#44135=CARTESIAN_POINT('Ctrl Pts',(6.21852020190849,15.6646461666652,-3.88257242852675));
#44136=CARTESIAN_POINT('Ctrl Pts',(6.21032175097156,15.6342621779096,-3.87426193331965));
#44137=CARTESIAN_POINT('Ctrl Pts',(6.20224971554734,15.60434669321,-3.86607958128502));
#44138=CARTESIAN_POINT('Ctrl Pts',(6.19453573488545,15.5742073104456,-3.8563242268315));
#44139=CARTESIAN_POINT('Ctrl Pts',(6.18727712052749,15.5440691681782,-3.84492712821924));
#44140=CARTESIAN_POINT('Ctrl Pts',(6.18014610180885,15.5144608096051,-3.83373037364125));
#44141=CARTESIAN_POINT('Ctrl Pts',(6.17345491813546,15.4848542830761,-3.82094865417076));
#44142=CARTESIAN_POINT('Ctrl Pts',(6.1672922922867,15.4554880016809,-3.8065606166512));
#44143=CARTESIAN_POINT('Ctrl Pts',(6.16649545488218,15.4516908944052,-3.80470022032753));
#44144=CARTESIAN_POINT('Ctrl Pts',(6.16570744531893,15.4478978303577,-3.80281303398504));
#44145=CARTESIAN_POINT('Ctrl Pts',(6.16492844635537,15.4441093467659,-3.80089907131186));
#44146=CARTESIAN_POINT('Ctrl Pts',(6.15899613680071,15.4152589137602,-3.78632367444429));
#44147=CARTESIAN_POINT('Ctrl Pts',(6.15358732682031,15.3866735129082,-3.77019140006747));
#44148=CARTESIAN_POINT('Ctrl Pts',(6.14877660702489,15.3585961452695,-3.75253620676512));
#44149=CARTESIAN_POINT('Ctrl Pts',(6.14402751803451,15.3308784807199,-3.73510719661675));
#44150=CARTESIAN_POINT('Ctrl Pts',(6.13986156567779,15.303656721696,-3.71619405950193));
#44151=CARTESIAN_POINT('Ctrl Pts',(6.13633724632498,15.2771655770841,-3.69587843831654));
#44152=CARTESIAN_POINT('Ctrl Pts',(6.13283362286278,15.2508299966468,-3.67568211672677));
#44153=CARTESIAN_POINT('Ctrl Pts',(6.12996433857516,15.2252172805214,-3.65409994594118));
#44154=CARTESIAN_POINT('Ctrl Pts',(6.12776996862142,15.2005469106632,-3.63125919646604));
#44155=CARTESIAN_POINT('Ctrl Pts',(6.12558304479817,15.175960254489,-3.60849595224508));
#44156=CARTESIAN_POINT('Ctrl Pts',(6.12406660150077,15.1523103055953,-3.58448308507558));
#44157=CARTESIAN_POINT('Ctrl Pts',(6.12324126585957,15.1297915883043,-3.55938867220841));
#44158=CARTESIAN_POINT('Ctrl Pts',(6.12241667337202,15.1072931474515,-3.5343168550026));
#44159=CARTESIAN_POINT('Ctrl Pts',(6.12228198917389,15.0859245249791,-3.50816605444565));
#44160=CARTESIAN_POINT('Ctrl Pts',(6.12283685496085,15.0658466643614,-3.48113814715521));
#44161=CARTESIAN_POINT('Ctrl Pts',(6.12339442435247,15.045670973604,-3.45397854535823));
#44162=CARTESIAN_POINT('Ctrl Pts',(6.12464823653243,15.0267991299266,-3.4259340178237));
#44163=CARTESIAN_POINT('Ctrl Pts',(6.12657673909308,15.0093526625765,-3.39723372259577));
#44164=CARTESIAN_POINT('Ctrl Pts',(6.12851270268902,14.9918386979301,-3.36842239100202));
#44165=CARTESIAN_POINT('Ctrl Pts',(6.13112843575211,14.9757613988018,-3.33895105166633));
#44166=CARTESIAN_POINT('Ctrl Pts',(6.13438231594651,14.9611962896866,-3.30906387764939));
#44167=CARTESIAN_POINT('Ctrl Pts',(6.13767358391751,14.9464638243649,-3.27883329363622));
#44168=CARTESIAN_POINT('Ctrl Pts',(6.14161752502853,14.9332785492476,-3.24817813040878));
#44169=CARTESIAN_POINT('Ctrl Pts',(6.14615364579537,14.9216678928345,-3.21735064817516));
#44170=CARTESIAN_POINT('Ctrl Pts',(6.14945760802415,14.9132110698768,-3.1948969168607));
#44171=CARTESIAN_POINT('Ctrl Pts',(6.1530753447366,14.905588505734,-3.17235178720936));
#44172=CARTESIAN_POINT('Ctrl Pts',(6.15697894263873,14.8987944830744,-3.14980875965272));
#44173=CARTESIAN_POINT('Ctrl Pts',(6.16243384140003,14.889300496573,-3.11830706911547));
#44174=CARTESIAN_POINT('Ctrl Pts',(6.16844711444727,14.8814260469965,-3.08681083225173));
#44175=CARTESIAN_POINT('Ctrl Pts',(6.17493398303811,14.8751150572397,-3.05555548377661));
#44176=CARTESIAN_POINT('Ctrl Pts',(6.18156924645999,14.8686596960893,-3.02358513204668));
#44177=CARTESIAN_POINT('Ctrl Pts',(6.18869966876894,14.8638396372848,-2.99186745460911));
#44178=CARTESIAN_POINT('Ctrl Pts',(6.19622900740018,14.8605521153216,-2.96062094277275));
#44179=CARTESIAN_POINT('Ctrl Pts',(6.20386986944998,14.8572158990831,-2.92891161235574));
#44180=CARTESIAN_POINT('Ctrl Pts',(6.21192119906387,14.855457238923,-2.89768789040987));
#44181=CARTESIAN_POINT('Ctrl Pts',(6.22028226351325,14.8551347288596,-2.8671362186537));
#44182=CARTESIAN_POINT('Ctrl Pts',(6.22884385259857,14.8548044839899,-2.83585182166933));
#44183=CARTESIAN_POINT('Ctrl Pts',(6.23772988449376,14.8559793294473,-2.80527231272382));
#44184=CARTESIAN_POINT('Ctrl Pts',(6.24683732091203,14.8584834957687,-2.77554952450875));
#44185=CARTESIAN_POINT('Ctrl Pts',(6.24787065150557,14.8587676187153,-2.77217717415927));
#44186=CARTESIAN_POINT('Ctrl Pts',(6.24890684053132,14.8590688368182,-2.76881580100156));
#44187=CARTESIAN_POINT('Ctrl Pts',(6.2499457442485,14.8593868813717,-2.76546558747461));
#44188=CARTESIAN_POINT('',(7.0000012282179,14.5427401407676,-3.16613547811813));
#44189=CARTESIAN_POINT('Ctrl Pts',(7.0000013293211,14.5427391135065,-3.16613474352585));
#44190=CARTESIAN_POINT('Ctrl Pts',(6.96887877241648,14.5590716998195,-3.1390116407485));
#44191=CARTESIAN_POINT('Ctrl Pts',(6.93707072944916,14.5752060957849,-3.11307622335859));
#44192=CARTESIAN_POINT('Ctrl Pts',(6.90460103412709,14.591151148044,-3.088301430666));
#44193=CARTESIAN_POINT('Ctrl Pts',(6.86312143260867,14.6115207390531,-3.05665196434374));
#44194=CARTESIAN_POINT('Ctrl Pts',(6.82056330189585,14.6315814111164,-3.02689528556155));
#44195=CARTESIAN_POINT('Ctrl Pts',(6.77697278425567,14.6513476542579,-2.99898817181636));
#44196=CARTESIAN_POINT('Ctrl Pts',(6.73506789076836,14.6703495463742,-2.9721602126101));
#44197=CARTESIAN_POINT('Ctrl Pts',(6.69220820290542,14.6890795109183,-2.9470414160688));
#44198=CARTESIAN_POINT('Ctrl Pts',(6.64840148543268,14.7075489660477,-2.92362425330318));
#44199=CARTESIAN_POINT('Ctrl Pts',(6.60341126352853,14.7265174013165,-2.89957444062669));
#44200=CARTESIAN_POINT('Ctrl Pts',(6.55744029917543,14.7452050310169,-2.87732107588973));
#44201=CARTESIAN_POINT('Ctrl Pts',(6.5104615664701,14.7636233772941,-2.85688934585874));
#44202=CARTESIAN_POINT('Ctrl Pts',(6.49869810258092,14.7682353269754,-2.85177324534746));
#44203=CARTESIAN_POINT('Ctrl Pts',(6.48687132345982,14.7728303613784,-2.84677157921616));
#44204=CARTESIAN_POINT('Ctrl Pts',(6.47498056272099,14.7774085926902,-2.84188519222801));
#44205=CARTESIAN_POINT('Ctrl Pts',(6.4282311540271,14.7954082490111,-2.8226739989862));
#44206=CARTESIAN_POINT('Ctrl Pts',(6.38049398200554,14.813148909004,-2.80524099676269));
#44207=CARTESIAN_POINT('Ctrl Pts',(6.3317535215381,14.8306268924779,-2.78964392165212));
#44208=CARTESIAN_POINT('Ctrl Pts',(6.30479293140245,14.8402947689059,-2.78101646213824));
#44209=CARTESIAN_POINT('Ctrl Pts',(6.27752507085231,14.8498821142477,-2.77295157353707));
#44210=CARTESIAN_POINT('Ctrl Pts',(6.2499457442485,14.8593868813717,-2.76546558747461));
#44211=CARTESIAN_POINT('',(6.99999966028507,14.7967844361631,-4.92965368890365));
#44212=CARTESIAN_POINT('Ctrl Pts',(6.999999755579,14.7967844361721,-4.92965368889445));
#44213=CARTESIAN_POINT('Ctrl Pts',(7.,14.7621585949968,-4.84258385989647));
#44214=CARTESIAN_POINT('Ctrl Pts',(7.,14.7150197661553,-4.71637142925406));
#44215=CARTESIAN_POINT('Ctrl Pts',(7.,14.6750808366962,-4.59674746789346));
#44216=CARTESIAN_POINT('Ctrl Pts',(7.,14.6500548613639,-4.51846226460458));
#44217=CARTESIAN_POINT('Ctrl Pts',(7.,14.6389243780002,-4.4820629208109));
#44218=CARTESIAN_POINT('Ctrl Pts',(7.,14.581446750461,-4.28361440547124));
#44219=CARTESIAN_POINT('Ctrl Pts',(7.,14.5473159321849,-4.12816776072898));
#44220=CARTESIAN_POINT('Ctrl Pts',(7.,14.4827629958402,-3.68737187183234));
#44221=CARTESIAN_POINT('Ctrl Pts',(7.,14.4884102191812,-3.41567190515103));
#44222=CARTESIAN_POINT('Ctrl Pts',(7.000002769616,14.5427399567595,-3.1661358977195));
#44223=CARTESIAN_POINT('Ctrl Pts',(6.99999922604844,14.7967844361462,-4.92965368893157));
#44224=CARTESIAN_POINT('Ctrl Pts',(6.99999541671933,14.8231421321045,-4.89367483326372));
#44225=CARTESIAN_POINT('Ctrl Pts',(6.99835381523207,14.8491523793382,-4.85878351348419));
#44226=CARTESIAN_POINT('Ctrl Pts',(6.99534856867432,14.8746944704123,-4.8250788148475));
#44227=CARTESIAN_POINT('Ctrl Pts',(6.99234332211657,14.9002365614864,-4.79137411621081));
#44228=CARTESIAN_POINT('Ctrl Pts',(6.98797378878021,14.925310754538,-4.7588558475189));
#44229=CARTESIAN_POINT('Ctrl Pts',(6.98248006879472,14.9498211812681,-4.7275907396323));
#44230=CARTESIAN_POINT('Ctrl Pts',(6.976606994457,14.976024110907,-4.69416670213496));
#44231=CARTESIAN_POINT('Ctrl Pts',(6.9694499941618,15.0015828464119,-4.66217424815261));
#44232=CARTESIAN_POINT('Ctrl Pts',(6.96130496289058,15.0264106533835,-4.63163259429477));
#44233=CARTESIAN_POINT('Ctrl Pts',(6.9554290502691,15.0443216987178,-4.60959951874131));
#44234=CARTESIAN_POINT('Ctrl Pts',(6.94903793998474,15.0618528940018,-4.58832087951969));
#44235=CARTESIAN_POINT('Ctrl Pts',(6.94223029564817,15.0789789048149,-4.56779549245821));
#44236=CARTESIAN_POINT('Ctrl Pts',(6.93362365721347,15.1006306503541,-4.54184604850422));
#44237=CARTESIAN_POINT('Ctrl Pts',(6.92435173065237,15.1216344536675,-4.51710097836386));
#44238=CARTESIAN_POINT('Ctrl Pts',(6.91459418292409,15.1419510597054,-4.49354340341939));
#44239=CARTESIAN_POINT('Ctrl Pts',(6.90513607886576,15.1616441813144,-4.47070877310125));
#44240=CARTESIAN_POINT('Ctrl Pts',(6.89522187554574,15.1806918465391,-4.4489893294753));
#44241=CARTESIAN_POINT('Ctrl Pts',(6.88501113930072,15.1990697417936,-4.4283466567952));
#44242=CARTESIAN_POINT('Ctrl Pts',(6.87463876704942,15.2177385592226,-4.40737721050242));
#44243=CARTESIAN_POINT('Ctrl Pts',(6.86396024783996,15.2357163136807,-4.38751882899225));
#44244=CARTESIAN_POINT('Ctrl Pts',(6.85312289688962,15.2529860247726,-4.36872385762821));
#44245=CARTESIAN_POINT('Ctrl Pts',(6.84770422141445,15.2616208803185,-4.35932637194619));
#44246=CARTESIAN_POINT('Ctrl Pts',(6.84224554360595,15.2700788492252,-4.3501946305685));
#44247=CARTESIAN_POINT('Ctrl Pts',(6.83676361365584,15.2783584971853,-4.34132207858134));
#44248=CARTESIAN_POINT('Ctrl Pts',(6.83402264868079,15.2824983211654,-4.33688580258776));
#44249=CARTESIAN_POINT('Ctrl Pts',(6.83127586167704,15.2865935652506,-4.33251432988044));
#44250=CARTESIAN_POINT('Ctrl Pts',(6.82852524201499,15.2906440957321,-4.32820679498813));
#44251=CARTESIAN_POINT('Ctrl Pts',(6.82714993218396,15.2926693609729,-4.32605302754197));
#44252=CARTESIAN_POINT('Ctrl Pts',(6.82577366363104,15.2946834478336,-4.32391524490488));
#44253=CARTESIAN_POINT('Ctrl Pts',(6.82439668045042,15.2966863408067,-4.32179333891745));
#44254=CARTESIAN_POINT('Ctrl Pts',(6.82331719383298,15.2982565097028,-4.32012986971237));
#44255=CARTESIAN_POINT('Ctrl Pts',(6.82270592634273,15.2991431246873,-4.31919185825726));
#44256=CARTESIAN_POINT('Ctrl Pts',(6.82146136389623,15.3009376438913,-4.31729558962247));
#44257=CARTESIAN_POINT('Ctrl Pts',(6.82111837395589,15.3014321968456,-4.31677299546278));
#44258=CARTESIAN_POINT('Ctrl Pts',(6.82072709014987,15.3019956963768,-4.31617776831686));
#44259=CARTESIAN_POINT('Ctrl Pts',(6.82026382823309,15.3026614233177,-4.31547514285564));
#44260=CARTESIAN_POINT('Ctrl Pts',(6.80986979753839,15.3175980844322,-4.299710603734));
#44261=CARTESIAN_POINT('Ctrl Pts',(6.79910042356942,15.3324180675512,-4.28431332886537));
#44262=CARTESIAN_POINT('Ctrl Pts',(6.7879747741671,15.3471115832376,-4.26929879229707));
#44263=CARTESIAN_POINT('Ctrl Pts',(6.75802588351796,15.3866647345756,-4.22888149191573));
#44264=CARTESIAN_POINT('Ctrl Pts',(6.72549937877864,15.4252998951193,-4.19123691311024));
#44265=CARTESIAN_POINT('Ctrl Pts',(6.69085593483662,15.4628507430421,-4.15655350064428));
#44266=CARTESIAN_POINT('Ctrl Pts',(6.66371764858482,15.4922665731088,-4.12938390465188));
#44267=CARTESIAN_POINT('Ctrl Pts',(6.63527895641645,15.5210174947097,-4.10403176413252));
#44268=CARTESIAN_POINT('Ctrl Pts',(6.60574127218368,15.5490325526764,-4.08058907629517));
#44269=CARTESIAN_POINT('Ctrl Pts',(6.5661772022082,15.5865571502388,-4.04918891185774));
#44270=CARTESIAN_POINT('Ctrl Pts',(6.52464362824406,15.6227609185537,-4.02121368452812));
#44271=CARTESIAN_POINT('Ctrl Pts',(6.4816917575019,15.6575041340452,-3.99674950069069));
#44272=CARTESIAN_POINT('Ctrl Pts',(6.44899681926555,15.6839506488303,-3.97812737863299));
#44273=CARTESIAN_POINT('Ctrl Pts',(6.41547886115081,15.7095513225518,-3.96154001705578));
#44274=CARTESIAN_POINT('Ctrl Pts',(6.3813625699735,15.7342522525339,-3.94702624011616));
#44275=CARTESIAN_POINT('Ctrl Pts',(6.34283814181153,15.7621447686835,-3.93063715039466));
#44276=CARTESIAN_POINT('Ctrl Pts',(6.30355144644052,15.7888900196305,-3.9168915304846));
#44277=CARTESIAN_POINT('Ctrl Pts',(6.26385592214248,15.8144315483213,-3.90575173240628));
#44278=CARTESIAN_POINT('Ctrl Pts',(6.99933866928551,24.8246602696117,-9.44604681568958));
#44279=CARTESIAN_POINT('Ctrl Pts',(6.99933866928551,24.8024268424346,-9.41529029807104));
#44280=CARTESIAN_POINT('Ctrl Pts',(6.99933866928551,24.437915482051,-8.91650381238244));
#44281=CARTESIAN_POINT('Ctrl Pts',(6.99933866928551,23.6489684573882,-8.00787919366893));
#44282=CARTESIAN_POINT('Ctrl Pts',(6.99933866928551,22.3090668585326,-6.88744611042101));
#44283=CARTESIAN_POINT('Ctrl Pts',(6.99933866928551,20.8065036616784,-5.99155840174367));
#44284=CARTESIAN_POINT('Ctrl Pts',(6.99933866928551,19.1801233637513,-5.34582278160595));
#44285=CARTESIAN_POINT('Ctrl Pts',(6.99933866928551,17.4735480440587,-4.9657269191405));
#44286=CARTESIAN_POINT('Ctrl Pts',(6.99933866928551,15.9617905172726,-4.87591919715298));
#44287=CARTESIAN_POINT('Ctrl Pts',(6.99933866928551,15.0338141052518,-4.93831842762876));
#44288=CARTESIAN_POINT('Ctrl Pts',(6.99933866928551,14.6872933691311,-4.97834430560805));
#44289=CARTESIAN_POINT('Ctrl Pts',(7.01704756088437,25.2191171808218,-9.16096594701436));
#44290=CARTESIAN_POINT('Ctrl Pts',(7.01704756088437,25.1958971300538,-9.12884521302238));
#44291=CARTESIAN_POINT('Ctrl Pts',(7.01704756088437,24.8152197698719,-8.60794384395676));
#44292=CARTESIAN_POINT('Ctrl Pts',(7.01704756088437,23.9915399790218,-7.65928052454269));
#44293=CARTESIAN_POINT('Ctrl Pts',(7.01704756088437,22.5916670864478,-6.48867427937066));
#44294=CARTESIAN_POINT('Ctrl Pts',(7.01704756088437,21.0226414798408,-5.55321290417034));
#44295=CARTESIAN_POINT('Ctrl Pts',(7.01704756088437,19.3239067410746,-4.87868204962013));
#44296=CARTESIAN_POINT('Ctrl Pts',(7.01704756088437,17.5412802279475,-4.48169569382117));
#44297=CARTESIAN_POINT('Ctrl Pts',(7.01704756088437,15.9624851498432,-4.38790582987388));
#44298=CARTESIAN_POINT('Ctrl Pts',(7.01704756088437,14.9934038436444,-4.45305428473393));
#44299=CARTESIAN_POINT('Ctrl Pts',(7.01704756088437,14.631431596948,-4.49486766018024));
#44300=CARTESIAN_POINT('Ctrl Pts',(6.7271181571115,25.5371657468869,-8.93110671799271));
#44301=CARTESIAN_POINT('Ctrl Pts',(6.7271181571115,25.5131501866105,-8.89788602339486));
#44302=CARTESIAN_POINT('Ctrl Pts',(6.7271181571115,25.1194382644694,-8.35915353832037));
#44303=CARTESIAN_POINT('Ctrl Pts',(6.7271181571115,24.2677536239904,-7.37820722173647));
#44304=CARTESIAN_POINT('Ctrl Pts',(6.7271181571115,22.8195261876635,-6.16714661578266));
#44305=CARTESIAN_POINT('Ctrl Pts',(6.7271181571115,21.1969122840431,-5.19977719806063));
#44306=CARTESIAN_POINT('Ctrl Pts',(6.7271181571115,19.439838534086,-4.50202889503887));
#44307=CARTESIAN_POINT('Ctrl Pts',(6.7271181571115,17.5958923372774,-4.09142382187531));
#44308=CARTESIAN_POINT('Ctrl Pts',(6.7271181571115,15.9630452284889,-3.99442317746496));
#44309=CARTESIAN_POINT('Ctrl Pts',(6.7271181571115,14.9608212588499,-4.06178831772415));
#44310=CARTESIAN_POINT('Ctrl Pts',(6.7271181571115,14.58639053915,-4.10504294312414));
#44311=CARTESIAN_POINT('Ctrl Pts',(6.25441317383083,25.6379536448148,-8.85826555162297));
#44312=CARTESIAN_POINT('Ctrl Pts',(6.25441317383083,25.6136859918143,-8.82469628537189));
#44313=CARTESIAN_POINT('Ctrl Pts',(6.25441317383083,25.215843486348,-8.28031321452375));
#44314=CARTESIAN_POINT('Ctrl Pts',(6.25441317383083,24.3552842580777,-7.28913658795351));
#44315=CARTESIAN_POINT('Ctrl Pts',(6.25441317383083,22.8917335241628,-6.06525621036345));
#44316=CARTESIAN_POINT('Ctrl Pts',(6.25441317383083,21.2521377744256,-5.08777530378322));
#44317=CARTESIAN_POINT('Ctrl Pts',(6.25441317383083,19.4765767022983,-4.3826695148969));
#44318=CARTESIAN_POINT('Ctrl Pts',(6.25441317383083,17.613198624076,-3.96774874268206));
#44319=CARTESIAN_POINT('Ctrl Pts',(6.25441317383083,15.9632227144307,-3.86973061903417));
#44320=CARTESIAN_POINT('Ctrl Pts',(6.25441317383083,14.9504960111262,-3.9377982151014));
#44321=CARTESIAN_POINT('Ctrl Pts',(6.25441317383083,14.5721172676417,-3.98150956493884));
#44322=CARTESIAN_POINT('',(7.00000000000001,24.7867247203242,-9.3325097692458));
#44323=CARTESIAN_POINT('Ctrl Pts',(7.00000000000006,24.7867247293774,-9.3325097625576));
#44324=CARTESIAN_POINT('Ctrl Pts',(7.00000000000006,24.6891826006153,-9.20047562542689));
#44325=CARTESIAN_POINT('Ctrl Pts',(7.00000000006077,24.5890285233467,-9.07101755125835));
#44326=CARTESIAN_POINT('Ctrl Pts',(6.99999999867348,24.4862283239914,-8.94403306164543));
#44327=CARTESIAN_POINT('Ctrl Pts',(6.99999999728335,24.383217075292,-8.81678787221477));
#44328=CARTESIAN_POINT('Ctrl Pts',(6.99999999423,24.2775485179081,-8.69202609764112));
#44329=CARTESIAN_POINT('Ctrl Pts',(6.99999999314812,24.1691470391679,-8.56967687293844));
#44330=CARTESIAN_POINT('Ctrl Pts',(6.99999999207005,24.061127052739,-8.44775822620449));
#44331=CARTESIAN_POINT('Ctrl Pts',(6.99999999472224,23.9503930271291,-8.32823485899167));
#44332=CARTESIAN_POINT('Ctrl Pts',(6.99999999803546,23.8368340148605,-8.21107349781402));
#44333=CARTESIAN_POINT('Ctrl Pts',(6.99999999907238,23.8012943438622,-8.17440642800796));
#44334=CARTESIAN_POINT('Ctrl Pts',(7.00000000000006,23.7654777308091,-8.13797099699824));
#44335=CARTESIAN_POINT('Ctrl Pts',(7.00000000000006,23.7293801188067,-8.10176700848402));
#44336=CARTESIAN_POINT('Ctrl Pts',(7.00000000000006,23.7004840050172,-8.07278574036939));
#44337=CARTESIAN_POINT('Ctrl Pts',(6.99999999938406,23.6714110890632,-8.04394890796352));
#44338=CARTESIAN_POINT('Ctrl Pts',(6.99999999847213,23.6421641709267,-8.01526109819976));
#44339=CARTESIAN_POINT('Ctrl Pts',(6.99999999416131,23.5039094271266,-7.87964934688404));
#44340=CARTESIAN_POINT('Ctrl Pts',(6.99999998574684,23.3617631569525,-7.7473702398002));
#44341=CARTESIAN_POINT('Ctrl Pts',(6.99999998500535,23.2160542950788,-7.61879342316149));
#44342=CARTESIAN_POINT('Ctrl Pts',(6.99999998426229,23.0700374208795,-7.48994480943497));
#44343=CARTESIAN_POINT('Ctrl Pts',(6.99999998984228,22.9204431673932,-7.36481445645444));
#44344=CARTESIAN_POINT('Ctrl Pts',(6.99999999473004,22.7676413783106,-7.24373929126517));
#44345=CARTESIAN_POINT('Ctrl Pts',(6.99999999759813,22.6779788884569,-7.17269365210419));
#44346=CARTESIAN_POINT('Ctrl Pts',(7.00000000000006,22.5872126828296,-7.10304362038108));
#44347=CARTESIAN_POINT('Ctrl Pts',(7.00000000000006,22.4954230550847,-7.03485104061892));
#44348=CARTESIAN_POINT('Ctrl Pts',(7.00000000000006,22.4321186731275,-6.98782079088417));
#44349=CARTESIAN_POINT('Ctrl Pts',(6.99999999890231,22.3683242960228,-6.94148920194487));
#44350=CARTESIAN_POINT('Ctrl Pts',(6.99999999758229,22.3040492398655,-6.8958618643371));
#44351=CARTESIAN_POINT('Ctrl Pts',(6.999999993463,22.1034710548579,-6.75347616899528));
#44352=CARTESIAN_POINT('Ctrl Pts',(6.99999998925884,21.8982142893946,-6.61794558861433));
#44353=CARTESIAN_POINT('Ctrl Pts',(6.99999999152164,21.6886162028712,-6.48945459759717));
#44354=CARTESIAN_POINT('Ctrl Pts',(6.99999999354313,21.5013710088194,-6.37466671500727));
#44355=CARTESIAN_POINT('Ctrl Pts',(7.00000000000006,21.3106603646735,-6.26549734902331));
#44356=CARTESIAN_POINT('Ctrl Pts',(7.00000000000006,21.1167056938803,-6.16210761400783));
#44357=CARTESIAN_POINT('Ctrl Pts',(7.00000000000006,21.0129457950191,-6.10679722419038));
#44358=CARTESIAN_POINT('Ctrl Pts',(6.99999999803041,20.9082630701657,-6.05312590552218));
#44359=CARTESIAN_POINT('Ctrl Pts',(6.99999999636328,20.8027238129362,-6.00113898290814));
#44360=CARTESIAN_POINT('Ctrl Pts',(6.99999999271544,20.5717938321343,-5.88738662803697));
#44361=CARTESIAN_POINT('Ctrl Pts',(6.99999999204991,20.336761374834,-5.78170184011558));
#44362=CARTESIAN_POINT('Ctrl Pts',(6.99999999506639,20.0983777911221,-5.68438505777925));
#44363=CARTESIAN_POINT('Ctrl Pts',(6.99999999705719,19.941050119291,-5.62015822404906));
#44364=CARTESIAN_POINT('Ctrl Pts',(7.00000000000006,19.7822633753942,-5.55957532148921));
#44365=CARTESIAN_POINT('Ctrl Pts',(7.00000000000006,19.6222386409051,-5.50271137547352));
#44366=CARTESIAN_POINT('Ctrl Pts',(7.00000000000006,19.4747046058049,-5.45028593365543));
#44367=CARTESIAN_POINT('Ctrl Pts',(6.99999999722485,19.3261163406549,-5.40103443266753));
#44368=CARTESIAN_POINT('Ctrl Pts',(6.99999999446477,19.1765618936819,-5.35498993307642));
#44369=CARTESIAN_POINT('Ctrl Pts',(6.99999999008284,18.9391276998962,-5.28188920715386));
#44370=CARTESIAN_POINT('Ctrl Pts',(6.99999998784252,18.6992583715269,-5.21686912534717));
#44371=CARTESIAN_POINT('Ctrl Pts',(6.99999999262696,18.4573223660356,-5.16006800350815));
#44372=CARTESIAN_POINT('Ctrl Pts',(6.99999999531402,18.3214448864838,-5.12816703343334));
#44373=CARTESIAN_POINT('Ctrl Pts',(7.00000000000006,18.1849153998852,-5.09885944130387));
#44374=CARTESIAN_POINT('Ctrl Pts',(7.00000000000006,18.0477988670123,-5.07217694339681));
#44375=CARTESIAN_POINT('Ctrl Pts',(7.00000000000006,17.856393082599,-5.03492990735382));
#44376=CARTESIAN_POINT('Ctrl Pts',(6.99999999014824,17.663843855679,-5.00273444785686));
#44377=CARTESIAN_POINT('Ctrl Pts',(6.99999998525267,17.4706055436115,-4.97570140054251));
#44378=CARTESIAN_POINT('Ctrl Pts',(6.99999998003395,17.2646116456454,-4.94688391227839));
#44379=CARTESIAN_POINT('Ctrl Pts',(6.99999998145014,17.0578350753082,-4.92393341763544));
#44380=CARTESIAN_POINT('Ctrl Pts',(6.99999998835951,16.8508303905368,-4.9068403931192));
#44381=CARTESIAN_POINT('Ctrl Pts',(6.9999999930865,16.7092102037236,-4.89514637118021));
#44382=CARTESIAN_POINT('Ctrl Pts',(7.00000000000006,16.5674833559243,-4.8861928324609));
#44383=CARTESIAN_POINT('Ctrl Pts',(7.00000000000006,16.4258270758153,-4.8799626811172));
#44384=CARTESIAN_POINT('Ctrl Pts',(7.00000000000006,16.2592199746816,-4.87263517361665));
#44385=CARTESIAN_POINT('Ctrl Pts',(6.99999999283356,16.0927257552284,-4.86914728796146));
#44386=CARTESIAN_POINT('Ctrl Pts',(6.99999999157262,15.9262294991414,-4.86944988962922));
#44387=CARTESIAN_POINT('Ctrl Pts',(6.99999999107899,15.8610504983776,-4.86956835039703));
#44388=CARTESIAN_POINT('Ctrl Pts',(6.99999999110876,15.7958711098815,-4.87026827073992));
#44389=CARTESIAN_POINT('Ctrl Pts',(6.99999999149986,15.7306842246115,-4.87154886618109));
#44390=CARTESIAN_POINT('Ctrl Pts',(6.99999999249462,15.5648782176151,-4.8748061228486));
#44391=CARTESIAN_POINT('Ctrl Pts',(6.99999999551031,15.3990235687409,-4.88181651104614));
#44392=CARTESIAN_POINT('Ctrl Pts',(6.9999999971705,15.2330389193309,-4.89260183864214));
#44393=CARTESIAN_POINT('Ctrl Pts',(6.99999999862381,15.0877376989017,-4.90204320125004));
#44394=CARTESIAN_POINT('Ctrl Pts',(6.99999999923222,14.9423366411189,-4.91437806045602));
#44395=CARTESIAN_POINT('Ctrl Pts',(6.99999999922778,14.7967844361711,-4.92965368888493));
#44396=CARTESIAN_POINT('',(6.27159471697229,25.5608579993301,-8.76071062884084));
#44397=CARTESIAN_POINT('Origin',(5.999999877385,24.7867246592848,-9.33250977407517));
#44398=CARTESIAN_POINT('Ctrl Pts',(6.27159470456983,25.5608577604478,-8.76071047658685));
#44399=CARTESIAN_POINT('Ctrl Pts',(6.27193966904855,25.4228903724782,-8.57412213201062));
#44400=CARTESIAN_POINT('Ctrl Pts',(6.2722578257596,25.2809101921298,-8.39339826441702));
#44401=CARTESIAN_POINT('Ctrl Pts',(6.2725491704145,25.1354917489078,-8.21861674188987));
#44402=CARTESIAN_POINT('Ctrl Pts',(6.27284515835287,24.9877557102086,-8.04104965202243));
#44403=CARTESIAN_POINT('Ctrl Pts',(6.27311347279902,24.8364709296681,-7.86961577203008));
#44404=CARTESIAN_POINT('Ctrl Pts',(6.27335411019051,24.6822005300308,-7.70435939028142));
#44405=CARTESIAN_POINT('Ctrl Pts',(6.27354178826528,24.5618818571093,-7.57547252286843));
#44406=CARTESIAN_POINT('Ctrl Pts',(6.27371263106456,24.4397462990353,-7.4503425101875));
#44407=CARTESIAN_POINT('Ctrl Pts',(6.27386663725764,24.3160449568949,-7.32897538004301));
#44408=CARTESIAN_POINT('Ctrl Pts',(6.27406868762992,24.1537534169881,-7.16974623907808));
#44409=CARTESIAN_POINT('Ctrl Pts',(6.27424175803524,23.9887687648483,-7.01699414752484));
#44410=CARTESIAN_POINT('Ctrl Pts',(6.27438584622067,23.8216789740255,-6.87062073725345));
#44411=CARTESIAN_POINT('Ctrl Pts',(6.27447251943017,23.7211696338436,-6.78257289893794));
#44412=CARTESIAN_POINT('Ctrl Pts',(6.2745487058153,23.6198976557413,-6.69683263130532));
#44413=CARTESIAN_POINT('Ctrl Pts',(6.27461440502469,23.5179829393777,-6.61337445203782));
#44414=CARTESIAN_POINT('Ctrl Pts',(6.27472591407379,23.3450065334529,-6.47172370315872));
#44415=CARTESIAN_POINT('Ctrl Pts',(6.27480721254685,23.1701811200194,-6.33664821756605));
#44416=CARTESIAN_POINT('Ctrl Pts',(6.27485829938236,22.994054627927,-6.20800456804343));
#44417=CARTESIAN_POINT('Ctrl Pts',(6.27487121302793,22.9495336652978,-6.17548623962592));
#44418=CARTESIAN_POINT('Ctrl Pts',(6.27488219624781,22.9049293331402,-6.14337877177348));
#44419=CARTESIAN_POINT('Ctrl Pts',(6.27489124903292,22.8602500105278,-6.11167962116953));
#44420=CARTESIAN_POINT('Ctrl Pts',(6.27492812717343,22.6782407926702,-5.98254745732212));
#44421=CARTESIAN_POINT('Ctrl Pts',(6.27493296994929,22.4949911250344,-5.86019253913393));
#44422=CARTESIAN_POINT('Ctrl Pts',(6.27490577729413,22.3110440760799,-5.7443888087212));
#44423=CARTESIAN_POINT('Ctrl Pts',(6.2748825782446,22.1541121151202,-5.64559240723818));
#44424=CARTESIAN_POINT('Ctrl Pts',(6.27483606247482,21.9966716419835,-5.55156390696271));
#44425=CARTESIAN_POINT('Ctrl Pts',(6.27476623045072,21.839031356596,-5.46215383379084));
#44426=CARTESIAN_POINT('Ctrl Pts',(6.27472435246144,21.7444950995172,-5.40853496573288));
#44427=CARTESIAN_POINT('Ctrl Pts',(6.27467408920095,21.6498864864855,-5.35657689080563));
#44428=CARTESIAN_POINT('Ctrl Pts',(6.27461544218262,21.5552677453534,-5.30624603899135));
#44429=CARTESIAN_POINT('Ctrl Pts',(6.27458611867346,21.5079583747874,-5.28108061308421));
#44430=CARTESIAN_POINT('Ctrl Pts',(6.27455469659286,21.4606464679072,-5.25632200111359));
#44431=CARTESIAN_POINT('Ctrl Pts',(6.27452117938581,21.4133394548803,-5.23196589211826));
#44432=CARTESIAN_POINT('Ctrl Pts',(6.27450442078228,21.3896859483668,-5.2197878376206));
#44433=CARTESIAN_POINT('Ctrl Pts',(6.27448713821938,21.36603366502,-5.20771040941384));
#44434=CARTESIAN_POINT('Ctrl Pts',(6.27446933169767,21.3423835227119,-5.19573306711981));
#44435=CARTESIAN_POINT('Ctrl Pts',(6.27445391976996,21.3219138156338,-5.18536641963247));
#44436=CARTESIAN_POINT('Ctrl Pts',(6.27443873000482,21.3022159979294,-5.17546006316596));
#44437=CARTESIAN_POINT('Ctrl Pts',(6.27442216616428,21.2812906867064,-5.16501291099337));
#44438=CARTESIAN_POINT('Ctrl Pts',(6.27441959259438,21.2780394629953,-5.16338970795018));
#44439=CARTESIAN_POINT('Ctrl Pts',(6.27441698585337,21.2747585611155,-5.16175354057576));
#44440=CARTESIAN_POINT('Ctrl Pts',(6.27441433995409,21.2714404304069,-5.16010075684977));
#44441=CARTESIAN_POINT('Ctrl Pts',(6.27440279826912,21.2569664027134,-5.15289114411244));
#44442=CARTESIAN_POINT('Ctrl Pts',(6.27439106676851,21.2424686881078,-5.14570647248201));
#44443=CARTESIAN_POINT('Ctrl Pts',(6.27437914545323,21.227947341887,-5.13854692036595));
#44444=CARTESIAN_POINT('Ctrl Pts',(6.27420011328074,21.0098683714745,-5.03102605209729));
#44445=CARTESIAN_POINT('Ctrl Pts',(6.27397827112255,20.786455912684,-4.9291684238133));
#44446=CARTESIAN_POINT('Ctrl Pts',(6.27371362325632,20.5579728151575,-4.8335167029945));
#44447=CARTESIAN_POINT('Ctrl Pts',(6.27345239736455,20.3324440710385,-4.73910178695646));
#44448=CARTESIAN_POINT('Ctrl Pts',(6.27314946557812,20.1019749203303,-4.65073332519588));
#44449=CARTESIAN_POINT('Ctrl Pts',(6.27280483384928,19.8668624230668,-4.5689577857274));
#44450=CARTESIAN_POINT('Ctrl Pts',(6.27260798841794,19.7325717670888,-4.52224954619952));
#44451=CARTESIAN_POINT('Ctrl Pts',(6.27239753873934,19.5967670728685,-4.47769264806433));
#44452=CARTESIAN_POINT('Ctrl Pts',(6.27217348622092,19.4595104125741,-4.43539260233193));
#44453=CARTESIAN_POINT('Ctrl Pts',(6.271770138192,19.2124156520413,-4.35924242026889));
#44454=CARTESIAN_POINT('Ctrl Pts',(6.27132270510958,18.9606118600149,-4.2904051057413));
#44455=CARTESIAN_POINT('Ctrl Pts',(6.27083119717597,18.7045322088994,-4.22947050840681));
#44456=CARTESIAN_POINT('Ctrl Pts',(6.27036732795719,18.4628525541364,-4.17196241519141));
#44457=CARTESIAN_POINT('Ctrl Pts',(6.26986420294061,18.2173647726219,-4.12149341735369));
#44458=CARTESIAN_POINT('Ctrl Pts',(6.26932183185764,17.9684809537258,-4.07857938281827));
#44459=CARTESIAN_POINT('Ctrl Pts',(6.26905885439899,17.847805578052,-4.0577718137999));
#44460=CARTESIAN_POINT('Ctrl Pts',(6.26878665041033,17.7263325216401,-4.03874067682215));
#44461=CARTESIAN_POINT('Ctrl Pts',(6.26850522122231,17.6041128540969,-4.02154646483739));
#44462=CARTESIAN_POINT('Ctrl Pts',(6.26791730047585,17.3487893793731,-3.98562682901008));
#44463=CARTESIAN_POINT('Ctrl Pts',(6.26728911939944,17.090204297127,-3.95772366469815));
#44464=CARTESIAN_POINT('Ctrl Pts',(6.26662069240957,16.8288425750066,-3.93824718398145));
#44465=CARTESIAN_POINT('Ctrl Pts',(6.26595957850088,16.5703403416834,-3.91898379023849));
#44466=CARTESIAN_POINT('Ctrl Pts',(6.26525909447508,16.3091218449081,-3.90796371321164));
#44467=CARTESIAN_POINT('Ctrl Pts',(6.26451925764027,16.0457069788102,-3.90559012140761));
#44468=CARTESIAN_POINT('Ctrl Pts',(6.26430324653886,15.968797405406,-3.9048971007904));
#44469=CARTESIAN_POINT('Ctrl Pts',(6.26408388074319,15.8917009326381,-3.90494120951631));
#44470=CARTESIAN_POINT('Ctrl Pts',(6.26386116074403,15.8144313374826,-3.90573258244604));
#44471=CARTESIAN_POINT('Ctrl Pts',(6.99999999998952,24.1259274560584,-10.9278021978677));
#44472=CARTESIAN_POINT('Ctrl Pts',(6.99999999998952,24.1259309537943,-10.9277942569083));
#44473=CARTESIAN_POINT('Ctrl Pts',(6.99999999998952,24.2426228977018,-10.6628666420065));
#44474=CARTESIAN_POINT('Ctrl Pts',(6.99999999998952,24.4687752087452,-10.1334777511239));
#44475=CARTESIAN_POINT('Ctrl Pts',(6.99999999998952,24.6831190611286,-9.59922082304237));
#44476=CARTESIAN_POINT('Ctrl Pts',(6.99999999998952,24.7867214499965,-9.33250574074716));
#44477=CARTESIAN_POINT('Ctrl Pts',(7.00000270565606,24.6668575635222,-11.166064437851));
#44478=CARTESIAN_POINT('Ctrl Pts',(7.00000270565606,24.6668611144483,-11.1660563761331));
#44479=CARTESIAN_POINT('Ctrl Pts',(7.00000270565606,24.7853275969941,-10.8970999979764));
#44480=CARTESIAN_POINT('Ctrl Pts',(7.00000270565606,25.0149154772904,-10.3596688248218));
#44481=CARTESIAN_POINT('Ctrl Pts',(7.00000270565606,25.23251564032,-9.81729560136332));
#44482=CARTESIAN_POINT('Ctrl Pts',(7.00000270565606,25.3376935135728,-9.54652457482602));
#44483=CARTESIAN_POINT('Ctrl Pts',(6.57967197777265,25.0472372157118,-11.3336093881521));
#44484=CARTESIAN_POINT('Ctrl Pts',(6.57967197777265,25.047240804041,-11.3336012415174));
#44485=CARTESIAN_POINT('Ctrl Pts',(6.57967197777265,25.1669551342874,-11.0618118549112));
#44486=CARTESIAN_POINT('Ctrl Pts',(6.57967197777265,25.3989588916405,-10.5187253845367));
#44487=CARTESIAN_POINT('Ctrl Pts',(6.57967197777265,25.6188488778711,-9.97064481817619));
#44488=CARTESIAN_POINT('Ctrl Pts',(6.57967197777265,25.7251346247603,-9.69702166963551));
#44489=CARTESIAN_POINT('Ctrl Pts',(5.98852435812717,25.0410285650909,-11.3308746780969));
#44490=CARTESIAN_POINT('Ctrl Pts',(5.98852435812717,25.0410321528096,-11.3308665328482));
#44491=CARTESIAN_POINT('Ctrl Pts',(5.98852435812717,25.1607261153798,-11.0591233873078));
#44492=CARTESIAN_POINT('Ctrl Pts',(5.98852435812717,25.3926904401917,-10.5161292240906));
#44493=CARTESIAN_POINT('Ctrl Pts',(5.98852435812717,25.6125430513673,-9.9681418143915));
#44494=CARTESIAN_POINT('Ctrl Pts',(5.98852435812717,25.7188107152653,-9.69456521889174));
#44495=CARTESIAN_POINT('',(6.99999999994009,24.1259366383783,-10.9277762175416));
#44496=CARTESIAN_POINT('',(5.98852583812712,25.0410393194101,-11.3308502415527));
#44497=CARTESIAN_POINT('Origin',(5.999999999061,24.1259421376201,-10.9277802195584));
#44498=CARTESIAN_POINT('',(5.98852581355276,25.7188095579036,-9.6945673613816));
#44499=CARTESIAN_POINT('Origin',(5.98846856209437,-11.4751154482372,4.75314848444354));
#44500=CARTESIAN_POINT('Origin',(6.,24.7867247762541,-9.33250981979305));
#44501=CARTESIAN_POINT('Origin',(6.99999997873566,-11.466399908179,4.74964876109848));
#44502=CARTESIAN_POINT('Origin',(5.999999877385,24.7867246592848,-9.33250977407517));
#44503=CARTESIAN_POINT('Origin',(5.99999764422236,24.7867226423257,-9.33250908125501));
#44504=CARTESIAN_POINT('Ctrl Pts',(-6.09415743644224,25.695632913879,-9.75660475861075));
#44505=CARTESIAN_POINT('Ctrl Pts',(-6.05606588786886,25.7001327750303,-9.74375762209026));
#44506=CARTESIAN_POINT('Ctrl Pts',(-5.71207088669795,25.7404909054814,-9.62883157111345));
#44507=CARTESIAN_POINT('Ctrl Pts',(-5.02599367437364,25.8158751281454,-9.41914130782388));
#44508=CARTESIAN_POINT('Ctrl Pts',(-3.98564775819421,25.9128460400099,-9.15673704498941));
#44509=CARTESIAN_POINT('Ctrl Pts',(-2.8121347216154,25.9981089845718,-8.93130224440336));
#44510=CARTESIAN_POINT('Ctrl Pts',(-1.52041606181854,26.0598653167182,-8.77189810582769));
#44511=CARTESIAN_POINT('Ctrl Pts',(-0.189383689790614,26.0855142661398,
-8.70820319779262));
#44512=CARTESIAN_POINT('Ctrl Pts',(1.08604876871579,26.0712746006462,-8.7432758938014));
#44513=CARTESIAN_POINT('Ctrl Pts',(2.24115591648484,26.0279846764949,-8.85386421781817));
#44514=CARTESIAN_POINT('Ctrl Pts',(3.27282426553086,25.9662680371191,-9.01516003136025));
#44515=CARTESIAN_POINT('Ctrl Pts',(4.19977149261964,25.8933059518543,-9.20943322947018));
#44516=CARTESIAN_POINT('Ctrl Pts',(5.05677934805222,25.8119848641214,-9.43016103454035));
#44517=CARTESIAN_POINT('Ctrl Pts',(5.68020727836871,25.7440091973074,-9.61906168812787));
#44518=CARTESIAN_POINT('Ctrl Pts',(6.02208888516753,25.7041476094482,-9.73229018312302));
#44519=CARTESIAN_POINT('Ctrl Pts',(6.09402271407761,25.6956511769004,-9.75655051851992));
#44520=CARTESIAN_POINT('Ctrl Pts',(-6.21832045083748,25.8362000143657,-9.42811502690297));
#44521=CARTESIAN_POINT('Ctrl Pts',(-6.17949927537105,25.8406700578237,-9.41497942109277));
#44522=CARTESIAN_POINT('Ctrl Pts',(-5.82891139971618,25.8807305423587,-9.29745967126212));
#44523=CARTESIAN_POINT('Ctrl Pts',(-5.12960176788881,25.9550321339388,-9.08280837935187));
#44524=CARTESIAN_POINT('Ctrl Pts',(-4.06864373258683,26.0495433651156,-8.81368358460258));
#44525=CARTESIAN_POINT('Ctrl Pts',(-2.87116826723681,26.1317341015626,-8.58205154196733));
#44526=CARTESIAN_POINT('Ctrl Pts',(-1.55239219357112,26.1905177359622,-8.41796833305674));
#44527=CARTESIAN_POINT('Ctrl Pts',(-0.193327228883218,26.2144487869133,
-8.3522524468396));
#44528=CARTESIAN_POINT('Ctrl Pts',(1.10884029567984,26.2012168234477,-8.38845432061946));
#44529=CARTESIAN_POINT('Ctrl Pts',(2.28827733632914,26.1602360331969,-8.50236336342224));
#44530=CARTESIAN_POINT('Ctrl Pts',(3.3413059591683,26.1011009640294,-8.66824165694523));
#44531=CARTESIAN_POINT('Ctrl Pts',(4.28702500024961,26.0305268774016,-8.86774343384528));
#44532=CARTESIAN_POINT('Ctrl Pts',(5.16096421564057,25.9511658454649,-9.09407335380042));
#44533=CARTESIAN_POINT('Ctrl Pts',(5.79643509995807,25.8842029429415,-9.28746110921518));
#44534=CARTESIAN_POINT('Ctrl Pts',(6.1448711748215,25.8446561037839,-9.40325337755369));
#44535=CARTESIAN_POINT('Ctrl Pts',(6.2181830809188,25.8362155442671,-9.42805839472418));
#44536=CARTESIAN_POINT('Ctrl Pts',(-6.32908148192128,25.7777118953252,-9.07101154408849));
#44537=CARTESIAN_POINT('Ctrl Pts',(-6.28955536356086,25.7821394193768,-9.05766430847315));
#44538=CARTESIAN_POINT('Ctrl Pts',(-5.93260993993696,25.8217847285637,-8.9382614968994));
#44539=CARTESIAN_POINT('Ctrl Pts',(-5.22075534859015,25.8947242064414,-8.7203448381954));
#44540=CARTESIAN_POINT('Ctrl Pts',(-4.14076534441269,25.9863193807797,-8.44741153118032));
#44541=CARTESIAN_POINT('Ctrl Pts',(-2.92177802350408,26.0649719169936,-8.21276332196714));
#44542=CARTESIAN_POINT('Ctrl Pts',(-1.57939308857452,26.1204058329895,-8.04679377181448));
#44543=CARTESIAN_POINT('Ctrl Pts',(-0.196603179973188,26.1424404003294,
-7.98050294385007));
#44544=CARTESIAN_POINT('Ctrl Pts',(1.12799353753121,26.1303178461725,-8.01700054852035));
#44545=CARTESIAN_POINT('Ctrl Pts',(2.32845047101542,26.0919206097672,-8.13213550603907));
#44546=CARTESIAN_POINT('Ctrl Pts',(3.40035685415087,26.0357243654915,-8.30005701232116));
#44547=CARTESIAN_POINT('Ctrl Pts',(4.36306687249998,25.9679208707662,-8.50222900241744));
#44548=CARTESIAN_POINT('Ctrl Pts',(5.25267862910245,25.890893519041,-8.7317891343879));
#44549=CARTESIAN_POINT('Ctrl Pts',(5.89955400277617,25.8251984299464,-8.92811103922429));
#44550=CARTESIAN_POINT('Ctrl Pts',(6.25429750722298,25.7860851791503,-9.04574939358607));
#44551=CARTESIAN_POINT('Ctrl Pts',(6.32894084680062,25.7777244435615,-9.07095421174326));
#44552=CARTESIAN_POINT('Ctrl Pts',(-6.39488356528743,25.5363210844092,-8.78685862136819));
#44553=CARTESIAN_POINT('Ctrl Pts',(-6.35487788319777,25.5407054572845,-8.77343701804182));
#44554=CARTESIAN_POINT('Ctrl Pts',(-5.99362024485588,25.5799359332653,-8.65339948326985));
#44555=CARTESIAN_POINT('Ctrl Pts',(-5.27348028270466,25.6516207929835,-8.43484668262279));
#44556=CARTESIAN_POINT('Ctrl Pts',(-4.18145907208881,25.7406723417186,-8.1621080481356));
#44557=CARTESIAN_POINT('Ctrl Pts',(-2.949539041277,25.8163265374911,-7.92849107071696));
#44558=CARTESIAN_POINT('Ctrl Pts',(-1.59372167497793,25.8689861431572,-7.7639717081696));
#44559=CARTESIAN_POINT('Ctrl Pts',(-0.198277517924796,25.8894849573124,
-7.69871919628221));
#44560=CARTESIAN_POINT('Ctrl Pts',(1.13804826103157,25.8782580228526,-7.73459284944474));
#44561=CARTESIAN_POINT('Ctrl Pts',(2.35022440052859,25.8419841352125,-7.84850481328988));
#44562=CARTESIAN_POINT('Ctrl Pts',(3.43314706915597,25.7882484371947,-8.01534244688904));
#44563=CARTESIAN_POINT('Ctrl Pts',(4.40622700504305,25.7228105380502,-8.21685996825643));
#44564=CARTESIAN_POINT('Ctrl Pts',(5.3057887963983,25.6478272285819,-8.44635317423841));
#44565=CARTESIAN_POINT('Ctrl Pts',(5.96018277702732,25.5832948021266,-8.64321733490893));
#44566=CARTESIAN_POINT('Ctrl Pts',(6.31919090099219,25.5446108704843,-8.76145689273703));
#44567=CARTESIAN_POINT('Ctrl Pts',(6.39473997509298,25.5363312504338,-8.78680248425463));
#44568=CARTESIAN_POINT('',(-5.98852245733802,25.7188096065183,-9.69456809190458));
#44569=CARTESIAN_POINT('Ctrl Pts',(-5.98852261949295,25.7188097472649,-9.69456765143577));
#44570=CARTESIAN_POINT('Ctrl Pts',(-5.87207793470072,25.7323476875087,-9.65602540128857));
#44571=CARTESIAN_POINT('Ctrl Pts',(-5.74893720685401,25.7463673807796,-9.61639632705623));
#44572=CARTESIAN_POINT('Ctrl Pts',(-5.61909817687992,25.7607399809517,-9.57606535652041));
#44573=CARTESIAN_POINT('Ctrl Pts',(-5.51159709928282,25.7726398696575,-9.54267306458784));
#44574=CARTESIAN_POINT('Ctrl Pts',(-5.39950421817578,25.7847813042434,-9.50880032892854));
#44575=CARTESIAN_POINT('Ctrl Pts',(-5.28282127149538,25.7970760121566,-9.47468790985182));
#44576=CARTESIAN_POINT('Ctrl Pts',(-5.21054205117668,25.8046919657068,-9.45355698091836));
#44577=CARTESIAN_POINT('Ctrl Pts',(-5.13650113477044,25.8123654142613,-9.4323371784525));
#44578=CARTESIAN_POINT('Ctrl Pts',(-5.06069864646586,25.8200697754248,-9.41109682695929));
#44579=CARTESIAN_POINT('Ctrl Pts',(-5.00141638195798,25.8260950654459,-9.39448554989407));
#44580=CARTESIAN_POINT('Ctrl Pts',(-4.94105673135458,25.8321392021902,-9.37786175899752));
#44581=CARTESIAN_POINT('Ctrl Pts',(-4.8796195626138,25.838189572322,-9.36125999719662));
#44582=CARTESIAN_POINT('Ctrl Pts',(-4.8096220277546,25.8450829725697,-9.34234502399392));
#44583=CARTESIAN_POINT('Ctrl Pts',(-4.73822586607673,25.8519843749472,-9.32345890387002));
#44584=CARTESIAN_POINT('Ctrl Pts',(-4.6654310767679,25.8588734261793,-9.30465633951433));
#44585=CARTESIAN_POINT('Ctrl Pts',(-4.62903368211348,25.8623179517954,-9.29525505733649));
#44586=CARTESIAN_POINT('Ctrl Pts',(-4.5922866305945,25.8657593845531,-9.28587466213729));
#44587=CARTESIAN_POINT('Ctrl Pts',(-4.55518992227452,25.8691950184334,-9.27652232790471));
#44588=CARTESIAN_POINT('Ctrl Pts',(-4.53664156811452,25.8709128353735,-9.27184616078842));
#44589=CARTESIAN_POINT('Ctrl Pts',(-4.5180057997557,25.8726292022635,-9.267177008788));
#44590=CARTESIAN_POINT('Ctrl Pts',(-4.49928261721151,25.8743437757585,-9.2625157760302));
#44591=CARTESIAN_POINT('Ctrl Pts',(-4.48992102593942,25.875201062506,-9.26018515965129));
#44592=CARTESIAN_POINT('Ctrl Pts',(-4.48053758112102,25.8760579008829,-9.25785652307483));
#44593=CARTESIAN_POINT('Ctrl Pts',(-4.47113228275811,25.8769142474015,-9.25552998043822));
#44594=CARTESIAN_POINT('Ctrl Pts',(-4.4617269843952,25.8777705939201,-9.2532034378016));
#44595=CARTESIAN_POINT('Ctrl Pts',(-4.45105740216065,25.8787389127704,-9.25057364239245));
#44596=CARTESIAN_POINT('Ctrl Pts',(-4.44285082703765,25.8794817676788,-9.24855674879096));
#44597=CARTESIAN_POINT('Ctrl Pts',(-4.30874234741994,25.8916211974477,-9.21559750204138));
#44598=CARTESIAN_POINT('Ctrl Pts',(-4.17030708094963,25.9036878750233,-9.1829900567557));
#44599=CARTESIAN_POINT('Ctrl Pts',(-4.02753713403268,25.9155537376321,-9.15105856413114));
#44600=CARTESIAN_POINT('Ctrl Pts',(-3.89073584476344,25.9269235345553,-9.12046200334463));
#44601=CARTESIAN_POINT('Ctrl Pts',(-3.74995452272013,25.9381087315707,-9.09048623610026));
#44602=CARTESIAN_POINT('Ctrl Pts',(-3.60520088627223,25.9489924261705,-9.06143417695892));
#44603=CARTESIAN_POINT('Ctrl Pts',(-3.45728944004113,25.9601135492601,-9.03174834530014));
#44604=CARTESIAN_POINT('Ctrl Pts',(-3.30522643331322,25.9709195633236,-9.00302795442544));
#44605=CARTESIAN_POINT('Ctrl Pts',(-3.14901186622847,25.9812763843197,-8.97561339885051));
#44606=CARTESIAN_POINT('Ctrl Pts',(-3.07090458268609,25.9864547948178,-8.96190612106305));
#44607=CARTESIAN_POINT('Ctrl Pts',(-2.99175940894427,25.9915207744709,-8.9485255226544));
#44608=CARTESIAN_POINT('Ctrl Pts',(-2.91157634414655,25.9964568067801,-8.93551526360204));
#44609=CARTESIAN_POINT('Ctrl Pts',(-2.89518327496918,25.9974659565215,-8.932855374295));
#44610=CARTESIAN_POINT('Ctrl Pts',(-2.87874682707864,25.9984696751547,-8.93021096065387));
#44611=CARTESIAN_POINT('Ctrl Pts',(-2.86226699500748,25.9994678077459,-8.92758240669926));
#44612=CARTESIAN_POINT('Ctrl Pts',(-2.83844310394662,26.000910747335,-8.92378246609356));
#44613=CARTESIAN_POINT('Ctrl Pts',(-2.81452854512119,26.0023420130239,-8.92001566975204));
#44614=CARTESIAN_POINT('Ctrl Pts',(-2.79052332849145,26.0037611565803,-8.91628315123654));
#44615=CARTESIAN_POINT('Ctrl Pts',(-2.77021808947114,26.0049615643735,-8.91312593412936));
#44616=CARTESIAN_POINT('Ctrl Pts',(-2.74984798224947,26.0061532976401,-8.90999324600946));
#44617=CARTESIAN_POINT('Ctrl Pts',(-2.72941300683531,26.0073360817096,-8.90688578004086));
#44618=CARTESIAN_POINT('Ctrl Pts',(-2.71919551912823,26.0079274737443,-8.90533204705655));
#44619=CARTESIAN_POINT('Ctrl Pts',(-2.70896181437299,26.008516628468,-8.90378461960582));
#44620=CARTESIAN_POINT('Ctrl Pts',(-2.69871189257079,26.0091035113992,-8.90224358452302));
#44621=CARTESIAN_POINT('Ctrl Pts',(-2.68846197076859,26.0096903943305,-8.90070254944022));
#44622=CARTESIAN_POINT('Ctrl Pts',(-2.67679403336959,26.0103543913698,-8.89895957144287));
#44623=CARTESIAN_POINT('Ctrl Pts',(-2.66791347602445,26.0108573102655,-8.89763974325157));
#44624=CARTESIAN_POINT('Ctrl Pts',(-2.48215217967096,26.0213772430126,-8.87003190443557));
#44625=CARTESIAN_POINT('Ctrl Pts',(-2.29149550040864,26.031141594686,-8.84454323782441));
#44626=CARTESIAN_POINT('Ctrl Pts',(-2.09593759637921,26.0399567757891,-8.82164664478182));
#44627=CARTESIAN_POINT('Ctrl Pts',(-1.99233080418927,26.0446270684126,-8.80951600465763));
#44628=CARTESIAN_POINT('Ctrl Pts',(-1.8873486414055,26.0490305925451,-8.79811362071221));
#44629=CARTESIAN_POINT('Ctrl Pts',(-1.78099278798611,26.0531361167612,-8.78751463948269));
#44630=CARTESIAN_POINT('Ctrl Pts',(-1.70012356651363,26.0562578118669,-8.77945554980521));
#44631=CARTESIAN_POINT('Ctrl Pts',(-1.61846022886176,26.0592076248522,-8.77185973311662));
#44632=CARTESIAN_POINT('Ctrl Pts',(-1.5360013136412,26.0619722371313,-8.76475833345694));
#44633=CARTESIAN_POINT('Ctrl Pts',(-1.46189047434314,26.0644569622309,-8.75837587393073));
#44634=CARTESIAN_POINT('Ctrl Pts',(-1.38713697991105,26.0667920820591,-8.75239281551445));
#44635=CARTESIAN_POINT('Ctrl Pts',(-1.3117420899921,26.0689671301156,-8.74683140022213));
#44636=CARTESIAN_POINT('Ctrl Pts',(-1.23210084237991,26.0712646802682,-8.7409567573538));
#44637=CARTESIAN_POINT('Ctrl Pts',(-1.15174319397122,26.0733836147045,-8.73555262591372));
#44638=CARTESIAN_POINT('Ctrl Pts',(-1.07066914321278,26.0753115011317,-8.73064468619408));
#44639=CARTESIAN_POINT('Ctrl Pts',(-1.03013211783356,26.0762754443453,-8.72819071633426));
#44640=CARTESIAN_POINT('Ctrl Pts',(-0.989415991865598,26.077191621347,-8.72586079302465));
#44641=CARTESIAN_POINT('Ctrl Pts',(-0.948520765211829,26.0780584628039,
-8.72365808622068));
#44642=CARTESIAN_POINT('Ctrl Pts',(-0.928073151884945,26.0784918835323,
-8.72255673281869));
#44643=CARTESIAN_POINT('Ctrl Pts',(-0.907580763387053,26.0789129700991,
-8.72148718345254));
#44644=CARTESIAN_POINT('Ctrl Pts',(-0.887043599715693,26.0793215255028,
-8.72044983132777));
#44645=CARTESIAN_POINT('Ctrl Pts',(-0.876775017880014,26.0795258032047,
-8.71993115526538));
#44646=CARTESIAN_POINT('Ctrl Pts',(-0.866495242251005,26.0797269480983,
-8.71942052850753));
#44647=CARTESIAN_POINT('Ctrl Pts',(-0.856204272829031,26.0799249355149,
-8.718917999984));
#44648=CARTESIAN_POINT('Ctrl Pts',(-0.845913303407058,26.0801229229315,
-8.71841547146047));
#44649=CARTESIAN_POINT('Ctrl Pts',(-0.833923452093846,26.0803491142949,
-8.71784146531518));
#44650=CARTESIAN_POINT('Ctrl Pts',(-0.825297783184885,26.0805094006148,
-8.71743475796202));
#44651=CARTESIAN_POINT('Ctrl Pts',(-0.603448600533726,26.084631908612,-8.70697438731385));
#44652=CARTESIAN_POINT('Ctrl Pts',(-0.379486899971072,26.0871467845146,
-8.70066381320836));
#44653=CARTESIAN_POINT('Ctrl Pts',(-0.153407990999127,26.0879157525049,
-8.6987153874091));
#44654=CARTESIAN_POINT('Ctrl Pts',(-0.0982029332275835,26.0881035228835,
-8.69823961123299));
#44655=CARTESIAN_POINT('Ctrl Pts',(-0.0428716692110073,26.0881870787357,
-8.69802412669697));
#44656=CARTESIAN_POINT('Ctrl Pts',(0.0125852468759724,26.0881662678656,
-8.69807058298918));
#44657=CARTESIAN_POINT('Ctrl Pts',(0.153868871692206,26.088113249498,-8.69818893636729));
#44658=CARTESIAN_POINT('Ctrl Pts',(0.295970722828568,26.0873812607907,-8.70001209002015));
#44659=CARTESIAN_POINT('Ctrl Pts',(0.438890814456262,26.0859637557959,-8.70357996189666));
#44660=CARTESIAN_POINT('Ctrl Pts',(0.510350860270108,26.0852550032984,-8.70536389783492));
#44661=CARTESIAN_POINT('Ctrl Pts',(0.582015465730846,26.0843748755081,-8.70758401484754));
#44662=CARTESIAN_POINT('Ctrl Pts',(0.653884630802583,26.0833230375972,-8.71024397464699));
#44663=CARTESIAN_POINT('Ctrl Pts',(0.689819213338452,26.0827971186417,-8.71157395454672));
#44664=CARTESIAN_POINT('Ctrl Pts',(0.725804935763038,26.0822282726436,-8.71301389529905));
#44665=CARTESIAN_POINT('Ctrl Pts',(0.761841798001913,26.0816164748928,-8.71456421474941));
#44666=CARTESIAN_POINT('Ctrl Pts',(0.77986022912135,26.0813105760174,-8.71533937447459));
#44667=CARTESIAN_POINT('Ctrl Pts',(0.797891445193713,26.0809939392436,-8.71614212888663));
#44668=CARTESIAN_POINT('Ctrl Pts',(0.815935446207505,26.080666563389,-8.71697252537766));
#44669=CARTESIAN_POINT('Ctrl Pts',(0.833979447221296,26.0803391875343,-8.71780292186869));
#44670=CARTESIAN_POINT('Ctrl Pts',(0.853658583946665,26.0799697510364,-8.71874048460496));
#44671=CARTESIAN_POINT('Ctrl Pts',(0.870105804060285,26.0796522180939,-8.71954668702734));
#44672=CARTESIAN_POINT('Ctrl Pts',(0.954941294048503,26.0780143691095,-8.72370511483821));
#44673=CARTESIAN_POINT('Ctrl Pts',(1.03915646093526,26.0761553385722,-8.72843526314769));
#44674=CARTESIAN_POINT('Ctrl Pts',(1.12274548012097,26.0740873004632,-8.73371107518766));
#44675=CARTESIAN_POINT('Ctrl Pts',(1.34023153458158,26.068706576378,-8.74743794452801));
#44676=CARTESIAN_POINT('Ctrl Pts',(1.5534774917799,26.0619126838085,-8.76485554934346));
#44677=CARTESIAN_POINT('Ctrl Pts',(1.76248314120672,26.0539184363475,-8.78549176678133));
#44678=CARTESIAN_POINT('Ctrl Pts',(1.93916409665569,26.0471605746181,-8.80293639865504));
#44679=CARTESIAN_POINT('Ctrl Pts',(2.11281537719476,26.039544475079,-8.82268188960559));
#44680=CARTESIAN_POINT('Ctrl Pts',(2.28344819734372,26.0311859009393,-8.84446642487241));
#44681=CARTESIAN_POINT('Ctrl Pts',(2.31468206953677,26.0296558867476,-8.84845402461854));
#44682=CARTESIAN_POINT('Ctrl Pts',(2.34581483023983,26.0281009648234,-8.85251000041726));
#44683=CARTESIAN_POINT('Ctrl Pts',(2.37684657615407,26.0265218157015,-8.85663275222822));
#44684=CARTESIAN_POINT('Ctrl Pts',(2.47767146807603,26.0213910202901,-8.87002793814233));
#44685=CARTESIAN_POINT('Ctrl Pts',(2.57829977349914,26.0159614000799,-8.88424000732834));
#44686=CARTESIAN_POINT('Ctrl Pts',(2.67796170055171,26.0102878204125,-8.89913258066258));
#44687=CARTESIAN_POINT('Ctrl Pts',(2.7797715277508,26.0044919645363,-8.91434611668933));
#44688=CARTESIAN_POINT('Ctrl Pts',(2.88057272493239,25.9984415859338,-8.93026972198904));
#44689=CARTESIAN_POINT('Ctrl Pts',(2.97955492182406,25.9922130910505,-8.94670742513009));
#44690=CARTESIAN_POINT('Ctrl Pts',(3.01344853266624,25.9900803218422,-8.95233604452729));
#44691=CARTESIAN_POINT('Ctrl Pts',(3.04712895851175,25.9879268149008,-8.95802452155688));
#44692=CARTESIAN_POINT('Ctrl Pts',(3.08056397548561,25.9857560785503,-8.96376371145562));
#44693=CARTESIAN_POINT('Ctrl Pts',(3.15906127951969,25.980659716511,-8.97723793624046));
#44694=CARTESIAN_POINT('Ctrl Pts',(3.23641909108672,25.9754553795562,-8.99102598292456));
#44695=CARTESIAN_POINT('Ctrl Pts',(3.31263593449704,25.970160509038,-9.00508309829586));
#44696=CARTESIAN_POINT('Ctrl Pts',(3.4564951477893,25.9601664463986,-9.03161588905429));
#44697=CARTESIAN_POINT('Ctrl Pts',(3.59628912015428,25.9498505824851,-9.0591058921734));
#44698=CARTESIAN_POINT('Ctrl Pts',(3.73202210285664,25.9393266493449,-9.08726369510383));
#44699=CARTESIAN_POINT('Ctrl Pts',(3.83584437087129,25.9312768843925,-9.10880162129055));
#44700=CARTESIAN_POINT('Ctrl Pts',(3.93728959599926,25.9231052112615,-9.13073051857037));
#44701=CARTESIAN_POINT('Ctrl Pts',(4.03635777759006,25.9148586837289,-9.15292779425468));
#44702=CARTESIAN_POINT('Ctrl Pts',(4.06112482298776,25.9127970518458,-9.15847711317576));
#44703=CARTESIAN_POINT('Ctrl Pts',(4.08675526254168,25.9106474134483,-9.16426728241562));
#44704=CARTESIAN_POINT('Ctrl Pts',(4.11470923701844,25.9082794988606,-9.17065119655818));
#44705=CARTESIAN_POINT('Ctrl Pts',(4.14266321149521,25.9059115842728,-9.17703511070074));
#44706=CARTESIAN_POINT('Ctrl Pts',(4.17043865126593,25.9035366069139,-9.18344354837801));
#44707=CARTESIAN_POINT('Ctrl Pts',(4.1980355563503,25.9011555857014,-9.18987381165783));
#44708=CARTESIAN_POINT('Ctrl Pts',(4.20574811720379,25.9004901570623,-9.19167088986997));
#44709=CARTESIAN_POINT('Ctrl Pts',(4.21344673427636,25.899824256114,-9.19346967337576));
#44710=CARTESIAN_POINT('Ctrl Pts',(4.221131407003,25.8991579044704,-9.1952701047956));
#44711=CARTESIAN_POINT('Ctrl Pts',(4.26844096715695,25.8950556083431,-9.20635419667437));
#44712=CARTESIAN_POINT('Ctrl Pts',(4.31522201712048,25.8909362468103,-9.21750071746783));
#44713=CARTESIAN_POINT('Ctrl Pts',(4.36147457089465,25.886805009107,-9.22869641509208));
#44714=CARTESIAN_POINT('Ctrl Pts',(4.51942902568656,25.8726966551718,-9.26693020263357));
#44715=CARTESIAN_POINT('Ctrl Pts',(4.67122070891271,25.858452365169,-9.30573242780717));
#44716=CARTESIAN_POINT('Ctrl Pts',(4.81684736679282,25.8442592310686,-9.34461209392482));
#44717=CARTESIAN_POINT('Ctrl Pts',(4.86949798770537,25.8391277713897,-9.3586688510582));
#44718=CARTESIAN_POINT('Ctrl Pts',(4.92134287243755,25.8340027593491,-9.37273615127393));
#44719=CARTESIAN_POINT('Ctrl Pts',(4.97238230340753,25.8288922459384,-9.38679219881856));
#44720=CARTESIAN_POINT('Ctrl Pts',(5.00462682864208,25.8256636425723,-9.39567220729706));
#44721=CARTESIAN_POINT('Ctrl Pts',(5.03654983724056,25.8224411457875,-9.40454687349655));
#44722=CARTESIAN_POINT('Ctrl Pts',(5.06815129371359,25.8192264788938,-9.41341144578933));
#44723=CARTESIAN_POINT('Ctrl Pts',(5.21039120874781,25.804757084225,-9.45331137922485));
#44724=CARTESIAN_POINT('Ctrl Pts',(5.34611635893376,25.7904487595192,-9.49300344357613));
#44725=CARTESIAN_POINT('Ctrl Pts',(5.4753262897967,25.7764523083133,-9.53208482760559));
#44726=CARTESIAN_POINT('Ctrl Pts',(5.60705266934046,25.7621832669828,-9.57192734738235));
#44727=CARTESIAN_POINT('Ctrl Pts',(5.73200777546778,25.748238173852,-9.61113514909158));
#44728=CARTESIAN_POINT('Ctrl Pts',(5.85019315497047,25.7347467326449,-9.64932598153051));
#44729=CARTESIAN_POINT('Ctrl Pts',(5.86232961570843,25.7333612960774,-9.65324779944399));
#44730=CARTESIAN_POINT('Ctrl Pts',(5.87439468823684,25.7319806192149,-9.65715893133953));
#44731=CARTESIAN_POINT('Ctrl Pts',(5.88638837412529,25.7306048262631,-9.66105898934999));
#44732=CARTESIAN_POINT('Ctrl Pts',(5.92102986644089,25.7266311086411,-9.67232356896765));
#44733=CARTESIAN_POINT('Ctrl Pts',(5.95507582044836,25.7226981505854,-9.68349575279175));
#44734=CARTESIAN_POINT('Ctrl Pts',(5.98852582161055,25.7188089328326,-9.6945670296992));
#44735=CARTESIAN_POINT('',(-6.27159361731479,25.5608563036375,-8.7607097378382));
#44736=CARTESIAN_POINT('Origin',(-5.999994980806,24.7867195890732,-9.33250914740904));
#44737=CARTESIAN_POINT('Ctrl Pts',(-6.2715938630759,25.5608571679648,-8.76070927462916));
#44738=CARTESIAN_POINT('Ctrl Pts',(-6.19708063874005,25.5689447885943,-8.73626652810999));
#44739=CARTESIAN_POINT('Ctrl Pts',(-6.1154389227446,25.577703521834,-8.70997409232932));
#44740=CARTESIAN_POINT('Ctrl Pts',(-6.02658468262738,25.58705204236,-8.68208171992035));
#44741=CARTESIAN_POINT('Ctrl Pts',(-5.93855991568889,25.5963132924639,-8.65444972872418));
#44742=CARTESIAN_POINT('Ctrl Pts',(-5.84345650339964,25.6061534772221,-8.62524745250685));
#44743=CARTESIAN_POINT('Ctrl Pts',(-5.74118376542963,25.6164754182921,-8.59476438981034));
#44744=CARTESIAN_POINT('Ctrl Pts',(-5.64049526630337,25.62663746905,-8.56475351992844));
#44745=CARTESIAN_POINT('Ctrl Pts',(-5.53285766337119,25.6372665650423,-8.53350118952672));
#44746=CARTESIAN_POINT('Ctrl Pts',(-5.41817807236923,25.6482508460994,-8.50132996802472));
#44747=CARTESIAN_POINT('Ctrl Pts',(-5.37925228009582,25.6519792500723,-8.49041006262196));
#44748=CARTESIAN_POINT('Ctrl Pts',(-5.33951511383068,25.6557484047636,-8.47938469052703));
#44749=CARTESIAN_POINT('Ctrl Pts',(-5.29896282541383,25.6595533901367,-8.46826772471874));
#44750=CARTESIAN_POINT('Ctrl Pts',(-5.21821391750951,25.6671299887815,-8.44613129584444));
#44751=CARTESIAN_POINT('Ctrl Pts',(-5.13423305843698,25.6748488767625,-8.42363096906741));
#44752=CARTESIAN_POINT('Ctrl Pts',(-5.04699090211752,25.6826701546544,-8.40088618232919));
#44753=CARTESIAN_POINT('Ctrl Pts',(-4.92201156784759,25.6938745785857,-8.36830298603306));
#44754=CARTESIAN_POINT('Ctrl Pts',(-4.79033921223311,25.7052898942599,-8.33521583496531));
#44755=CARTESIAN_POINT('Ctrl Pts',(-4.65188791926913,25.7167846607454,-8.30201798427405));
#44756=CARTESIAN_POINT('Ctrl Pts',(-4.51343662630514,25.728279427231,-8.26882013358279));
#44757=CARTESIAN_POINT('Ctrl Pts',(-4.36820619844028,25.7398537430577,-8.23551131174542));
#44758=CARTESIAN_POINT('Ctrl Pts',(-4.21611372757936,25.7513582417137,-8.20253791990527));
#44759=CARTESIAN_POINT('Ctrl Pts',(-4.07083064345331,25.7623476683212,-8.17104079165483));
#44760=CARTESIAN_POINT('Ctrl Pts',(-3.9192856518954,25.7732731892018,-8.13984997581947));
#44761=CARTESIAN_POINT('Ctrl Pts',(-3.76142356347455,25.7839926998624,-8.10940008417812));
#44762=CARTESIAN_POINT('Ctrl Pts',(-3.73054864169615,25.7860892390407,-8.10344464527578));
#44763=CARTESIAN_POINT('Ctrl Pts',(-3.69943211321045,25.7881778519993,-8.09751769687057));
#44764=CARTESIAN_POINT('Ctrl Pts',(-3.66807362047968,25.7902574078451,-8.09162270996234));
#44765=CARTESIAN_POINT('Ctrl Pts',(-3.58017497373741,25.7960864553775,-8.07509891284474));
#44766=CARTESIAN_POINT('Ctrl Pts',(-3.49037512731969,25.801844445983,-8.05882589668978));
#44767=CARTESIAN_POINT('Ctrl Pts',(-3.39866710747283,25.8075055236016,-8.04288325163617));
#44768=CARTESIAN_POINT('Ctrl Pts',(-3.3528130975494,25.8103360624109,-8.03491192910937));
#44769=CARTESIAN_POINT('Ctrl Pts',(-3.30648203531614,25.8131423275125,-8.0270232354011));
#44770=CARTESIAN_POINT('Ctrl Pts',(-3.25967321929016,25.8159209780059,-8.01922760696347));
#44771=CARTESIAN_POINT('Ctrl Pts',(-3.23626881127717,25.8173103032525,-8.01532979274466));
#44772=CARTESIAN_POINT('Ctrl Pts',(-3.21274496422015,25.8186927219388,-8.01145524714368));
#44773=CARTESIAN_POINT('Ctrl Pts',(-3.18910159440111,25.8200678037302,-8.00760529675011));
#44774=CARTESIAN_POINT('Ctrl Pts',(-3.17727990949158,25.8207553446259,-8.00568032155332));
#44775=CARTESIAN_POINT('Ctrl Pts',(-3.16542834385686,25.8214410511118,-8.00376149530634));
#44776=CARTESIAN_POINT('Ctrl Pts',(-3.15354688766476,25.8221248688895,-8.00184898569553));
#44777=CARTESIAN_POINT('Ctrl Pts',(-3.14166543147266,25.8228086866673,-7.99993647608473));
#44778=CARTESIAN_POINT('Ctrl Pts',(-3.12814004114031,25.8235825261987,-7.99777350825232));
#44779=CARTESIAN_POINT('Ctrl Pts',(-3.11781283770829,25.8241706012354,-7.9961305753528));
#44780=CARTESIAN_POINT('Ctrl Pts',(-3.07662183306222,25.8265161928305,-7.9895775857518));
#44781=CARTESIAN_POINT('Ctrl Pts',(-3.03569007114915,25.8288015738271,-7.98319701218292));
#44782=CARTESIAN_POINT('Ctrl Pts',(-2.99501928700432,25.8310283058371,-7.97698426024937));
#44783=CARTESIAN_POINT('Ctrl Pts',(-2.79740326302321,25.8418478151123,-7.94679700517417));
#44784=CARTESIAN_POINT('Ctrl Pts',(-2.60595262121096,25.8512834386195,-7.92057031856116));
#44785=CARTESIAN_POINT('Ctrl Pts',(-2.42086041250325,25.8595189574556,-7.89776639789247));
#44786=CARTESIAN_POINT('Ctrl Pts',(-2.23093226301904,25.8679696473226,-7.87436667467437));
#44787=CARTESIAN_POINT('Ctrl Pts',(-2.04769882625,25.8751567868988,-7.85457054853199));
#44788=CARTESIAN_POINT('Ctrl Pts',(-1.87131987055302,25.8812683271939,-7.83782008293064));
#44789=CARTESIAN_POINT('Ctrl Pts',(-1.78117209159126,25.8843919525803,-7.82925887298034));
#44790=CARTESIAN_POINT('Ctrl Pts',(-1.69281413701159,25.8872344267731,-7.8214936708302));
#44791=CARTESIAN_POINT('Ctrl Pts',(-1.60626302542332,25.8898197051797,-7.81445268897836));
#44792=CARTESIAN_POINT('Ctrl Pts',(-1.43906925792771,25.8948137766467,-7.80085138148414));
#44793=CARTESIAN_POINT('Ctrl Pts',(-1.27862000666068,25.898849112208,-7.78995007340322));
#44794=CARTESIAN_POINT('Ctrl Pts',(-1.12501483003616,25.9020960343758,-7.78123950576144));
#44795=CARTESIAN_POINT('Ctrl Pts',(-0.969937933891774,25.9053740659037,
-7.77244548056499));
#44796=CARTESIAN_POINT('Ctrl Pts',(-0.821836496383836,25.9078485158435,
-7.76588420567675));
#44797=CARTESIAN_POINT('Ctrl Pts',(-0.680780588800408,25.9096791291633,
-7.76107116675371));
#44798=CARTESIAN_POINT('Ctrl Pts',(-0.538386308398421,25.9115271117883,
-7.75621246054469));
#44799=CARTESIAN_POINT('Ctrl Pts',(-0.403171507814499,25.9127190007761,
-7.7531351475061));
#44800=CARTESIAN_POINT('Ctrl Pts',(-0.275181335910393,25.9134031565432,
-7.75138350697485));
#44801=CARTESIAN_POINT('Ctrl Pts',(-0.23621669182446,25.9136114372695,-7.75085024689049));
#44802=CARTESIAN_POINT('Ctrl Pts',(-0.197921464321872,25.9137725488857,
-7.75044015773775));
#44803=CARTESIAN_POINT('Ctrl Pts',(-0.160296520144296,25.9138903830244,
-7.7501411945641));
#44804=CARTESIAN_POINT('Ctrl Pts',(-0.153989050215633,25.9139101368154,
-7.75009107618468));
#44805=CARTESIAN_POINT('Ctrl Pts',(-0.147700417129246,25.9139286740498,
-7.75004408169272));
#44806=CARTESIAN_POINT('Ctrl Pts',(-0.14143062418855,25.9139460125369,-7.75000015385425));
#44807=CARTESIAN_POINT('Ctrl Pts',(-0.103047756247163,25.9140521565302,
-7.74973123326331));
#44808=CARTESIAN_POINT('Ctrl Pts',(-0.0662555242699623,25.9141126179072,
-7.74957970085559));
#44809=CARTESIAN_POINT('Ctrl Pts',(-0.0289807896640162,25.9141334369677,
-7.74952611301502));
#44810=CARTESIAN_POINT('Ctrl Pts',(-0.0185588351444299,25.9141392579428,
-7.74951112994289));
#44811=CARTESIAN_POINT('Ctrl Pts',(-0.00809915958435751,25.9141418859072,
-7.74950410082371));
#44812=CARTESIAN_POINT('Ctrl Pts',(0.00244355159823323,25.9141412341181,
-7.74950529176633));
#44813=CARTESIAN_POINT('Ctrl Pts',(0.127127936130238,25.9141335256725,-7.74951937656334));
#44814=CARTESIAN_POINT('Ctrl Pts',(0.258986331532658,25.9136690001181,-7.75068425796915));
#44815=CARTESIAN_POINT('Ctrl Pts',(0.397985519236686,25.9126040414671,-7.75344426483185));
#44816=CARTESIAN_POINT('Ctrl Pts',(0.535666549793538,25.9115491820323,-7.75617809799646));
#44817=CARTESIAN_POINT('Ctrl Pts',(0.680353904295599,25.9099052023948,-7.76047708456449));
#44818=CARTESIAN_POINT('Ctrl Pts',(0.831993346520431,25.9075172238835,-7.76681627110057));
#44819=CARTESIAN_POINT('Ctrl Pts',(0.942271910387529,25.9057805857312,-7.77142639348712));
#44820=CARTESIAN_POINT('Ctrl Pts',(1.0562268708477,25.9036501454434,-7.77711643635547));
#44821=CARTESIAN_POINT('Ctrl Pts',(1.17382842543845,25.9010612483794,-7.78408308820957));
#44822=CARTESIAN_POINT('Ctrl Pts',(1.33438952198139,25.8975266339528,-7.79359463986226));
#44823=CARTESIAN_POINT('Ctrl Pts',(1.50174979691909,25.8931378133859,-7.8054850775063));
#44824=CARTESIAN_POINT('Ctrl Pts',(1.6757982372772,25.8877230536469,-7.82026951813892));
#44825=CARTESIAN_POINT('Ctrl Pts',(1.84379921682465,25.8824964343315,-7.83454026083119));
#44826=CARTESIAN_POINT('Ctrl Pts',(2.0180318933548,25.876313850564,-7.85150771899027));
#44827=CARTESIAN_POINT('Ctrl Pts',(2.19835974785299,25.8690099500942,-7.87166082959492));
#44828=CARTESIAN_POINT('Ctrl Pts',(2.26108749901612,25.8664692596809,-7.87867116812908));
#44829=CARTESIAN_POINT('Ctrl Pts',(2.32455243103844,25.8637927933555,-7.88606718978257));
#44830=CARTESIAN_POINT('Ctrl Pts',(2.38874762164454,25.8609732905271,-7.8938701297493));
#44831=CARTESIAN_POINT('Ctrl Pts',(2.47500693013271,25.8571847144366,-7.90435496824498));
#44832=CARTESIAN_POINT('Ctrl Pts',(2.56258480514964,25.8531378845742,-7.91557450655615));
#44833=CARTESIAN_POINT('Ctrl Pts',(2.65146458196224,25.848815666565,-7.92757930467197));
#44834=CARTESIAN_POINT('Ctrl Pts',(2.72897715732554,25.8450462348541,-7.93804875961486));
#44835=CARTESIAN_POINT('Ctrl Pts',(2.80747992813828,25.8410673768089,-7.9491155169345));
#44836=CARTESIAN_POINT('Ctrl Pts',(2.88696060599889,25.8368674947661,-7.96081344720335));
#44837=CARTESIAN_POINT('Ctrl Pts',(2.9267009449292,25.8347675537447,-7.96666241233777));
#44838=CARTESIAN_POINT('Ctrl Pts',(2.96668575943288,25.8326123506864,-7.97266917549959));
#44839=CARTESIAN_POINT('Ctrl Pts',(3.00691339244417,25.8304004308499,-7.97883801236851));
#44840=CARTESIAN_POINT('Ctrl Pts',(3.02702720894982,25.8292944709316,-7.98192243080296));
#44841=CARTESIAN_POINT('Ctrl Pts',(3.0472017300277,25.8281743314571,-7.98504736795455));
#44842=CARTESIAN_POINT('Ctrl Pts',(3.06743674395561,25.8270398286313,-7.98821335935204));
#44843=CARTESIAN_POINT('Ctrl Pts',(3.07755425091957,25.8264725772184,-7.98979635505079));
#44844=CARTESIAN_POINT('Ctrl Pts',(3.0876868810919,25.825901734945,-7.99138961432908));
#44845=CARTESIAN_POINT('Ctrl Pts',(3.09783460752958,25.8253272787821,-7.99299320423445));
#44846=CARTESIAN_POINT('Ctrl Pts',(3.10798233396726,25.8247528226193,-7.99459679413982));
#44847=CARTESIAN_POINT('Ctrl Pts',(3.11649242506835,25.8242692127508,-7.99594695059774));
#44848=CARTESIAN_POINT('Ctrl Pts',(3.12832304853956,25.82359304553,-7.99783503294886));
#44849=CARTESIAN_POINT('Ctrl Pts',(3.24396953136902,25.8169833887294,-8.01629137920404));
#44850=CARTESIAN_POINT('Ctrl Pts',(3.35682435864532,25.8101922685851,-8.03535487522875));
#44851=CARTESIAN_POINT('Ctrl Pts',(3.46689563034231,25.8032667769389,-8.05487934571839));
#44852=CARTESIAN_POINT('Ctrl Pts',(3.6391333436612,25.7924298816586,-8.08543091561534));
#44853=CARTESIAN_POINT('Ctrl Pts',(3.80455492699797,25.7812649336087,-8.11710823621666));
#44854=CARTESIAN_POINT('Ctrl Pts',(3.96321661982111,25.7699421395512,-8.14939090713435));
#44855=CARTESIAN_POINT('Ctrl Pts',(4.12187831264424,25.7586193454937,-8.18167357805204));
#44856=CARTESIAN_POINT('Ctrl Pts',(4.27378038615049,25.7471386169463,-8.21456188766466));
#44857=CARTESIAN_POINT('Ctrl Pts',(4.41899134481302,25.7356523279005,-8.24759224460065));
#44858=CARTESIAN_POINT('Ctrl Pts',(4.56352096949038,25.7242199328525,-8.28046762215402));
#44859=CARTESIAN_POINT('Ctrl Pts',(4.70142263449432,25.7127820946714,-8.31348398400438));
#44860=CARTESIAN_POINT('Ctrl Pts',(4.83277716227932,25.701475689374,-8.34623545712527));
#44861=CARTESIAN_POINT('Ctrl Pts',(4.90532510903957,25.6952310893333,-8.364324305438));
#44862=CARTESIAN_POINT('Ctrl Pts',(4.97587596872295,25.6890262679304,-8.38233324870066));
#44863=CARTESIAN_POINT('Ctrl Pts',(5.04444366156708,25.6828820630984,-8.40020029227818));
#44864=CARTESIAN_POINT('Ctrl Pts',(5.13538873989178,25.6747326684417,-8.42389832863012));
#44865=CARTESIAN_POINT('Ctrl Pts',(5.22284501849858,25.6666900645241,-8.44734628553018));
#44866=CARTESIAN_POINT('Ctrl Pts',(5.30684506809983,25.6587988385195,-8.47041118653151));
#44867=CARTESIAN_POINT('Ctrl Pts',(5.42689981782459,25.6475205218101,-8.50337605893679));
#44868=CARTESIAN_POINT('Ctrl Pts',(5.5398950614998,25.6365523282452,-8.53555660222992));
#44869=CARTESIAN_POINT('Ctrl Pts',(5.64592784626714,25.626011852568,-8.56661221179925));
#44870=CARTESIAN_POINT('Ctrl Pts',(5.75378710344553,25.615289811462,-8.59820277114107));
#44871=CARTESIAN_POINT('Ctrl Pts',(5.8544421213826,25.6050102665336,-8.6286293612162));
#44872=CARTESIAN_POINT('Ctrl Pts',(5.94798770048386,25.5952770852613,-8.65758355223814));
#44873=CARTESIAN_POINT('Ctrl Pts',(6.0249647423883,25.5872678184433,-8.68140945611321));
#44874=CARTESIAN_POINT('Ctrl Pts',(6.09712761964016,25.5796281190708,-8.70423930677315));
#44875=CARTESIAN_POINT('Ctrl Pts',(6.16452450090577,25.5724066275389,-8.72592555602332));
#44876=CARTESIAN_POINT('Ctrl Pts',(6.201659121019,25.5684276994394,-8.73787433781357));
#44877=CARTESIAN_POINT('Ctrl Pts',(6.23734677867825,25.5645756133094,-8.74947634942516));
#44878=CARTESIAN_POINT('Ctrl Pts',(6.27159479316256,25.5608580129641,-8.76071029006199));
#44879=CARTESIAN_POINT('Ctrl Pts',(-6.390311350175,25.6807323022503,-8.98425322501931));
#44880=CARTESIAN_POINT('Ctrl Pts',(-4.260207566783,25.9287942543074,-8.27686643699921));
#44881=CARTESIAN_POINT('Ctrl Pts',(0.0001663376502052,26.1774622431302,
-7.56886858723369));
#44882=CARTESIAN_POINT('Ctrl Pts',(4.260540242084,25.9287748360782,-8.27692172383348));
#44883=CARTESIAN_POINT('Ctrl Pts',(6.390810363126,25.680674187269,-8.98441894883408));
#44884=CARTESIAN_POINT('Ctrl Pts',(-6.390311350175,25.1149800030297,-8.18394436969906));
#44885=CARTESIAN_POINT('Ctrl Pts',(-4.260207566783,25.3660541768592,-7.53598542510633));
#44886=CARTESIAN_POINT('Ctrl Pts',(0.0001663376502052,25.6190332007536,
-6.88615243075911));
#44887=CARTESIAN_POINT('Ctrl Pts',(4.260540242084,25.3660344219837,-7.53603616990792));
#44888=CARTESIAN_POINT('Ctrl Pts',(6.390810363126,25.1149211823672,-8.18409617097628));
#44889=CARTESIAN_POINT('Ctrl Pts',(-6.390311350175,23.7052267659156,-6.6337432666024));
#44890=CARTESIAN_POINT('Ctrl Pts',(-4.260207566783,23.9981304018685,-6.09525796678867));
#44891=CARTESIAN_POINT('Ctrl Pts',(0.0001663376502052,24.2900543482721,
-5.55781881254414));
#44892=CARTESIAN_POINT('Ctrl Pts',(4.260540242084,23.9981076058214,-6.09529993486804));
#44893=CARTESIAN_POINT('Ctrl Pts',(6.390810363126,23.7051581455831,-6.63386942084684));
#44894=CARTESIAN_POINT('Ctrl Pts',(-6.390311350175,21.0044950488536,-4.89945807529049));
#44895=CARTESIAN_POINT('Ctrl Pts',(-4.260207566783,21.4424839272,-4.44478852896696));
#44896=CARTESIAN_POINT('Ctrl Pts',(0.0001663376502052,21.8807691942899,
-3.98943207395094));
#44897=CARTESIAN_POINT('Ctrl Pts',(4.260540242084,21.4424497019397,-4.44482408729352));
#44898=CARTESIAN_POINT('Ctrl Pts',(6.390810363126,21.0043924385214,-4.89956459350057));
#44899=CARTESIAN_POINT('Ctrl Pts',(-6.390311350175,18.1258724665889,-4.02654101163599));
#44900=CARTESIAN_POINT('Ctrl Pts',(-4.260207566783,18.7395194568021,-3.53815117609504));
#44901=CARTESIAN_POINT('Ctrl Pts',(0.0001663376502052,19.3531464197629,
-3.05107327276496));
#44902=CARTESIAN_POINT('Ctrl Pts',(4.260540242084,18.7394715392942,-3.53818921151541));
#44903=CARTESIAN_POINT('Ctrl Pts',(6.390810363126,18.1257287037498,-4.02665542972081));
#44904=CARTESIAN_POINT('Ctrl Pts',(-6.390311350175,16.240422330399,-3.91824273036391));
#44905=CARTESIAN_POINT('Ctrl Pts',(-4.260207566783,16.9591796068581,-3.34435593602518));
#44906=CARTESIAN_POINT('Ctrl Pts',(0.0001663376502052,17.6779466440266,
-2.76852020743102));
#44907=CARTESIAN_POINT('Ctrl Pts',(4.260540242084,16.9591234790623,-3.34440090245649));
#44908=CARTESIAN_POINT('Ctrl Pts',(6.390810363126,16.2402539427348,-3.91837717831515));
#44909=CARTESIAN_POINT('Ctrl Pts',(-6.390311350175,15.4604268853052,-3.94960622933079));
#44910=CARTESIAN_POINT('Ctrl Pts',(-4.260207566783,16.2185124735635,-3.32899325071769));
#44911=CARTESIAN_POINT('Ctrl Pts',(0.0001663376502052,16.9766190503815,
-2.70682781485386));
#44912=CARTESIAN_POINT('Ctrl Pts',(4.260540242084,16.2184532737935,-3.32904183498501));
#44913=CARTESIAN_POINT('Ctrl Pts',(6.390810363126,15.4602492839623,-3.9497516241131));
#44914=CARTESIAN_POINT('',(-6.26385894387447,15.8144218171323,-3.90574358261498));
#44915=CARTESIAN_POINT('Ctrl Pts',(-6.27159552384793,25.5608567088063,-8.76070944182709));
#44916=CARTESIAN_POINT('Ctrl Pts',(-6.27195777365649,25.4158727521427,-8.56459404632321));
#44917=CARTESIAN_POINT('Ctrl Pts',(-6.27229031339005,25.2662939880144,-8.37478230713065));
#44918=CARTESIAN_POINT('Ctrl Pts',(-6.27259314329467,25.1127468329758,-8.19135361540759));
#44919=CARTESIAN_POINT('Ctrl Pts',(-6.27289863603481,24.9578495113491,-8.00631200359623));
#44920=CARTESIAN_POINT('Ctrl Pts',(-6.27317389416156,24.7989136560697,-7.82776610778095));
#44921=CARTESIAN_POINT('Ctrl Pts',(-6.27341891792754,24.6365419304632,-7.65576216835644));
#44922=CARTESIAN_POINT('Ctrl Pts',(-6.27366754313708,24.4717836094022,-7.48123005588655));
#44923=CARTESIAN_POINT('Ctrl Pts',(-6.27388503866392,24.3034876610362,-7.3134335727354));
#44924=CARTESIAN_POINT('Ctrl Pts',(-6.27407140477198,24.1322426600605,-7.15238583194492));
#44925=CARTESIAN_POINT('Ctrl Pts',(-6.27421804520854,23.997500125787,-7.02566691688459));
#44926=CARTESIAN_POINT('Ctrl Pts',(-6.27434541285329,23.8609309481042,-6.90312555205716));
#44927=CARTESIAN_POINT('Ctrl Pts',(-6.27445350783479,23.7228045338919,-6.78475354206035));
#44928=CARTESIAN_POINT('Ctrl Pts',(-6.27450263029994,23.6600346450967,-6.73096080483236));
#44929=CARTESIAN_POINT('Ctrl Pts',(-6.27454777269265,23.5969429742338,-6.67802891099079));
#44930=CARTESIAN_POINT('Ctrl Pts',(-6.27458893502498,23.5335572607895,-6.62595230104111));
#44931=CARTESIAN_POINT('Ctrl Pts',(-6.2747071268515,23.351554132648,-6.47642166710454));
#44932=CARTESIAN_POINT('Ctrl Pts',(-6.27479250388727,23.1671305121251,-6.33394416675351));
#44933=CARTESIAN_POINT('Ctrl Pts',(-6.27484506613229,22.9809077959271,-6.19837352650065));
#44934=CARTESIAN_POINT('Ctrl Pts',(-6.27489762837732,22.7946850797292,-6.0628028862478));
#44935=CARTESIAN_POINT('Ctrl Pts',(-6.27491737583159,22.6066631058893,-5.93413899916805));
#44936=CARTESIAN_POINT('Ctrl Pts',(-6.27490430849512,22.4174128626672,-5.81221513152887));
#44937=CARTESIAN_POINT('Ctrl Pts',(-6.27489476886027,22.2792532446046,-5.72320623675051));
#44938=CARTESIAN_POINT('Ctrl Pts',(-6.27486754212272,22.1401875184331,-5.63763292305786));
#44939=CARTESIAN_POINT('Ctrl Pts',(-6.27482284547966,22.0006885576582,-5.5556073289692));
#44940=CARTESIAN_POINT('Ctrl Pts',(-6.27477793189728,21.8605125256569,-5.47318361600363));
#44941=CARTESIAN_POINT('Ctrl Pts',(-6.27471537841422,21.7198993850789,-5.39434222334161));
#44942=CARTESIAN_POINT('Ctrl Pts',(-6.27463540540562,21.5793421829761,-5.31914585597933));
#44943=CARTESIAN_POINT('Ctrl Pts',(-6.27457693026747,21.4765687353424,-5.26416333066059));
#44944=CARTESIAN_POINT('Ctrl Pts',(-6.27450914207864,21.3738254880783,-5.2111284861831));
#44945=CARTESIAN_POINT('Ctrl Pts',(-6.27443212698732,21.2713080572712,-5.16004844385829));
#44946=CARTESIAN_POINT('Ctrl Pts',(-6.27435635557793,21.1704461341697,-5.10979327007536));
#44947=CARTESIAN_POINT('Ctrl Pts',(-6.2742702487733,21.0681857430153,-5.06062314250506));
#44948=CARTESIAN_POINT('Ctrl Pts',(-6.27417380657344,20.9645377930346,-5.01262251543797));
#44949=CARTESIAN_POINT('Ctrl Pts',(-6.27399075735707,20.7678119193992,-4.92151636913622));
#44950=CARTESIAN_POINT('Ctrl Pts',(-6.27377047509006,20.5660845709857,-4.83462207821818));
#44951=CARTESIAN_POINT('Ctrl Pts',(-6.27351295977241,20.359498064142,-4.75246107710196));
#44952=CARTESIAN_POINT('Ctrl Pts',(-6.27325823661086,20.155151508612,-4.67119092140055));
#44953=CARTESIAN_POINT('Ctrl Pts',(-6.2729670834335,19.946050481584,-4.59455195740143));
#44954=CARTESIAN_POINT('Ctrl Pts',(-6.27263950024032,19.7323768917561,-4.52307344733918));
#44955=CARTESIAN_POINT('Ctrl Pts',(-6.2723170042366,19.5220215369732,-4.45270495979887));
#44956=CARTESIAN_POINT('Ctrl Pts',(-6.27195920090826,19.3072344669029,-4.38733790193485));
#44957=CARTESIAN_POINT('Ctrl Pts',(-6.27156609025531,19.0882335843155,-4.3275012229039));
#44958=CARTESIAN_POINT('Ctrl Pts',(-6.27136275697641,18.9749571640432,-4.29655118872356));
#44959=CARTESIAN_POINT('Ctrl Pts',(-6.27114997760678,18.86055411936,-4.26708114042404));
#44960=CARTESIAN_POINT('Ctrl Pts',(-6.27092775214643,18.7450594689835,-4.23916684282755));
#44961=CARTESIAN_POINT('Ctrl Pts',(-6.27050608511531,18.525911373813,-4.18620018916566));
#44962=CARTESIAN_POINT('Ctrl Pts',(-6.2700504091853,18.3028302897812,-4.13883345388171));
#44963=CARTESIAN_POINT('Ctrl Pts',(-6.26956072372642,18.0760898397093,-4.09760201550297));
#44964=CARTESIAN_POINT('Ctrl Pts',(-6.26938505591299,17.9947498726805,-4.0828108133279));
#44965=CARTESIAN_POINT('Ctrl Pts',(-6.26920501136115,17.9129394062442,-4.06880939222112));
#44966=CARTESIAN_POINT('Ctrl Pts',(-6.26902059004181,17.830672539127,-4.05562321484025));
#44967=CARTESIAN_POINT('Ctrl Pts',(-6.26850854405841,17.6022584977174,-4.0190117797407));
#44968=CARTESIAN_POINT('Ctrl Pts',(-6.26796275775828,17.3703223746845,-3.98868456769828));
#44969=CARTESIAN_POINT('Ctrl Pts',(-6.2673832305189,17.1352158000369,-3.96507801654729));
#44970=CARTESIAN_POINT('Ctrl Pts',(-6.26681232023244,16.9036050097943,-3.94182246967379));
#44971=CARTESIAN_POINT('Ctrl Pts',(-6.26620866493078,16.6689173034159,-3.92508923644793));
#44972=CARTESIAN_POINT('Ctrl Pts',(-6.26557226401876,16.4315383934375,-3.91530365129545));
#44973=CARTESIAN_POINT('Ctrl Pts',(-6.26502584939568,16.2277245629199,-3.90690173558202));
#44974=CARTESIAN_POINT('Ctrl Pts',(-6.26445529483575,16.0219275203492,-3.90362173020364));
#44975=CARTESIAN_POINT('Ctrl Pts',(-6.26386059996225,15.8144217505981,-3.90573752907647));
#44976=CARTESIAN_POINT('Ctrl Pts',(6.26385988960052,15.8144313888753,-3.90573722891367));
#44977=CARTESIAN_POINT('Ctrl Pts',(5.97383890811555,15.9109016778241,-3.82533638560084));
#44978=CARTESIAN_POINT('Ctrl Pts',(5.68187770057698,16.0000524237085,-3.74992558202442));
#44979=CARTESIAN_POINT('Ctrl Pts',(5.38846872966892,16.0819645988975,-3.67979129585554));
#44980=CARTESIAN_POINT('Ctrl Pts',(5.11338321554584,16.1587613401665,-3.61403691176594));
#44981=CARTESIAN_POINT('Ctrl Pts',(4.8370251180331,16.2291950416424,-3.55292118456409));
#44982=CARTESIAN_POINT('Ctrl Pts',(4.55980027851165,16.2933699268073,-3.49665879142387));
#44983=CARTESIAN_POINT('Ctrl Pts',(4.30239166101817,16.3529575470819,-3.44441807280681));
#44984=CARTESIAN_POINT('Ctrl Pts',(4.04423578353628,16.4071490501026,-3.39636191484229));
#44985=CARTESIAN_POINT('Ctrl Pts',(3.78565753068499,16.4560640033003,-3.35263740201647));
#44986=CARTESIAN_POINT('Ctrl Pts',(3.57067796546936,16.4967314424799,-3.31628524690324));
#44987=CARTESIAN_POINT('Ctrl Pts',(3.35540644993641,16.53375215926,-3.28292688525913));
#44988=CARTESIAN_POINT('Ctrl Pts',(3.14002968425104,16.5672169853369,-3.25263029902007));
#44989=CARTESIAN_POINT('Ctrl Pts',(2.89780164180822,16.6048539109611,-3.21855660145092));
#44990=CARTESIAN_POINT('Ctrl Pts',(2.65545154831624,16.6380109389512,-3.18835920226728));
#44991=CARTESIAN_POINT('Ctrl Pts',(2.41322309383044,16.6667127080183,-3.16209554360299));
#44992=CARTESIAN_POINT('Ctrl Pts',(2.17467399151019,16.6949785088322,-3.13623081928184));
#44993=CARTESIAN_POINT('Ctrl Pts',(1.93624286096661,16.7189233572091,-3.11418128167405));
#44994=CARTESIAN_POINT('Ctrl Pts',(1.69816245541642,16.7386097374021,-3.09596954709885));
#44995=CARTESIAN_POINT('Ctrl Pts',(1.46175003732677,16.7581581951347,-3.07788540364077));
#44996=CARTESIAN_POINT('Ctrl Pts',(1.22568344709819,16.7735076019663,-3.06358553975951));
#44997=CARTESIAN_POINT('Ctrl Pts',(0.990190580144821,16.7847583353012,-3.05305920629704));
#44998=CARTESIAN_POINT('Ctrl Pts',(0.756490769869116,16.7959234048841,-3.04261302096284));
#44999=CARTESIAN_POINT('Ctrl Pts',(0.523355979403398,16.8030519622097,-3.03588315603065));
#45000=CARTESIAN_POINT('Ctrl Pts',(0.291008938069498,16.8062812827463,-3.0328258709267));
#45001=CARTESIAN_POINT('Ctrl Pts',(0.193862822501669,16.8076314869247,-3.03154759610845));
#45002=CARTESIAN_POINT('Ctrl Pts',(0.0968544166298517,16.8083005240372,
-3.03091093566987));
#45003=CARTESIAN_POINT('Ctrl Pts',(-5.14033260401447E-13,16.8083004872782,
-3.03091093310305));
#45004=CARTESIAN_POINT('Ctrl Pts',(-7.96995737912801E-7,16.8083004872779,
-3.03091093310303));
#45005=CARTESIAN_POINT('Ctrl Pts',(-1.59399094937538E-6,16.8083004872776,
-3.03091093310305));
#45006=CARTESIAN_POINT('Ctrl Pts',(-2.39098615129052E-6,16.8083004872772,
-3.03091093310312));
#45007=CARTESIAN_POINT('Ctrl Pts',(-0.230506131557345,16.8083003735928,
-3.03091095192717));
#45008=CARTESIAN_POINT('Ctrl Pts',(-0.461891800831802,16.8045079999109,
-3.03451929091951));
#45009=CARTESIAN_POINT('Ctrl Pts',(-0.693935583712521,16.7967708693938,
-3.04179370678685));
#45010=CARTESIAN_POINT('Ctrl Pts',(-0.928010239167388,16.7889660226639,
-3.04913178913771));
#45011=CARTESIAN_POINT('Ctrl Pts',(-1.1627545784042,16.7771470646875,-3.06020038435807));
#45012=CARTESIAN_POINT('Ctrl Pts',(-1.39793885818094,16.7611979788335,-3.07502429701105));
#45013=CARTESIAN_POINT('Ctrl Pts',(-1.63471559035675,16.7451409003871,-3.08994858361459));
#45014=CARTESIAN_POINT('Ctrl Pts',(-1.87193824099098,16.7248976083887,-3.10867916066466));
#45015=CARTESIAN_POINT('Ctrl Pts',(-2.10937236833873,16.7003903422879,-3.13120709605691));
#45016=CARTESIAN_POINT('Ctrl Pts',(-2.34982826438089,16.6755711779342,-3.1540217392223));
#45017=CARTESIAN_POINT('Ctrl Pts',(-2.59050105421909,16.6463788347557,-3.18073096523689));
#45018=CARTESIAN_POINT('Ctrl Pts',(-2.83114723065116,16.6127737269867,-3.21129121206657));
#45019=CARTESIAN_POINT('Ctrl Pts',(-2.93418537812882,16.5983849338563,-3.22437627855912));
#45020=CARTESIAN_POINT('Ctrl Pts',(-3.0372186465189,16.5831876475592,-3.23816694041524));
#45021=CARTESIAN_POINT('Ctrl Pts',(-3.14022792105303,16.5671810042051,-3.25265793254405));
#45022=CARTESIAN_POINT('Ctrl Pts',(-3.40298085139679,16.5263517442645,-3.28962111535118));
#45023=CARTESIAN_POINT('Ctrl Pts',(-3.66557290592767,16.4802294293196,-3.3311415890159));
#45024=CARTESIAN_POINT('Ctrl Pts',(-3.92766532767384,16.4286539573448,-3.37709229468276));
#45025=CARTESIAN_POINT('Ctrl Pts',(-4.19885767852042,16.3752877691976,-3.42463842291429));
#45026=CARTESIAN_POINT('Ctrl Pts',(-4.46951509946873,16.3160835074943,-3.47692733800474));
#45027=CARTESIAN_POINT('Ctrl Pts',(-4.73926230901666,16.2509126285198,-3.53378214924202));
#45028=CARTESIAN_POINT('Ctrl Pts',(-5.03507254493692,16.1794449269006,-3.59613028308734));
#45029=CARTESIAN_POINT('Ctrl Pts',(-5.32978818261875,16.1008019704071,-3.6639688704703));
#45030=CARTESIAN_POINT('Ctrl Pts',(-5.62291431247201,16.014869556307,-3.73702784181589));
#45031=CARTESIAN_POINT('Ctrl Pts',(-5.83747944819202,15.9519679647521,-3.79050621343079));
#45032=CARTESIAN_POINT('Ctrl Pts',(-6.05119291280412,15.8851618807612,-3.84678083666339));
#45033=CARTESIAN_POINT('Ctrl Pts',(-6.26386059996225,15.8144217505981,-3.90573752907647));
#45034=CARTESIAN_POINT('Ctrl Pts',(6.38247014577615,15.7729006312219,-3.93895139429922));
#45035=CARTESIAN_POINT('Ctrl Pts',(5.83981133037685,15.9681476187677,-3.78553079687121));
#45036=CARTESIAN_POINT('Ctrl Pts',(4.52590233473943,16.369552788887,-3.46059646224381));
#45037=CARTESIAN_POINT('Ctrl Pts',(2.3863676788619,16.7684714876093,-3.11895962047874));
#45038=CARTESIAN_POINT('Ctrl Pts',(0.000145921253848828,16.9128764845052,
-2.99096322074304));
#45039=CARTESIAN_POINT('Ctrl Pts',(-2.38607593148343,16.7685070072141,-3.11892840793774));
#45040=CARTESIAN_POINT('Ctrl Pts',(-4.52571177279445,16.369604017143,-3.4605539154598));
#45041=CARTESIAN_POINT('Ctrl Pts',(-5.83971599368801,15.9681816437148,-3.78550400961911));
#45042=CARTESIAN_POINT('Ctrl Pts',(-6.38246546509551,15.7729022400972,-3.93895010743252));
#45043=CARTESIAN_POINT('Ctrl Pts',(6.17792611310107,15.1551690118173,-3.88975075307634));
#45044=CARTESIAN_POINT('Ctrl Pts',(5.65238026945388,15.3441929863978,-3.74331335325337));
#45045=CARTESIAN_POINT('Ctrl Pts',(4.38005561086563,15.7328411772922,-3.43305555917197));
#45046=CARTESIAN_POINT('Ctrl Pts',(2.30906659857668,16.119049889924,-3.10675668983587));
#45047=CARTESIAN_POINT('Ctrl Pts',(0.000141183631923982,16.2588285236581,
-2.98451005281823));
#45048=CARTESIAN_POINT('Ctrl Pts',(-2.3087842620022,16.119084273518,-3.10672687830997));
#45049=CARTESIAN_POINT('Ctrl Pts',(-4.37987109836434,15.7328907786648,-3.43301492630012));
#45050=CARTESIAN_POINT('Ctrl Pts',(-5.65228794008332,15.3442259268502,-3.743287783153));
#45051=CARTESIAN_POINT('Ctrl Pts',(-6.177921579923,15.1551705696293,-3.88974952300261));
#45052=CARTESIAN_POINT('Ctrl Pts',(6.17628882186073,14.7460473480683,-3.38362402344176));
#45053=CARTESIAN_POINT('Ctrl Pts',(5.65209551729923,14.9328346346656,-3.23898800415555));
#45054=CARTESIAN_POINT('Ctrl Pts',(4.3823925489299,15.3172277280071,-2.93223668842095));
#45055=CARTESIAN_POINT('Ctrl Pts',(2.31204710154926,15.7000802439509,-2.60875661073035));
#45056=CARTESIAN_POINT('Ctrl Pts',(0.000141413130813221,15.8388906345013,
-2.48731588780259));
#45057=CARTESIAN_POINT('Ctrl Pts',(-2.31176457385417,15.7001143733183,-2.60872701329724));
#45058=CARTESIAN_POINT('Ctrl Pts',(-4.38220833686575,15.3172768284095,-2.93219647030261));
#45059=CARTESIAN_POINT('Ctrl Pts',(-5.65200342190241,14.9328671899495,-3.23896275109574));
#45060=CARTESIAN_POINT('Ctrl Pts',(-6.176284300804,14.7460488896197,-3.38362281162595));
#45061=CARTESIAN_POINT('Ctrl Pts',(6.37612500939897,14.8213329701347,-2.77073838960337));
#45062=CARTESIAN_POINT('Ctrl Pts',(5.83680124907823,15.0113419617907,-2.62156111143535));
#45063=CARTESIAN_POINT('Ctrl Pts',(4.52946237799516,15.4027707876115,-2.30490021431075));
#45064=CARTESIAN_POINT('Ctrl Pts',(2.3922729610528,15.7937874269067,-1.96995867414585));
#45065=CARTESIAN_POINT('Ctrl Pts',(0.000146391209654873,15.9359006779543,
-1.84389364375196));
#45066=CARTESIAN_POINT('Ctrl Pts',(-2.39198089092465,15.7938223457685,-1.96992797308875));
#45067=CARTESIAN_POINT('Ctrl Pts',(-4.52927258508639,15.4028208397379,-2.30485864836242));
#45068=CARTESIAN_POINT('Ctrl Pts',(-5.83670648990435,15.0113750845678,-2.62153507085255));
#45069=CARTESIAN_POINT('Ctrl Pts',(-6.376120358534,14.8213345408617,-2.77073714556678));
#45070=CARTESIAN_POINT('',(-6.24994532642006,14.8593843574536,-2.76546731080821));
#45071=CARTESIAN_POINT('Origin',(-6.52772047565603,15.803815900541,-2.9412381944653));
#45072=CARTESIAN_POINT('Ctrl Pts',(6.24994434955625,14.8593821393419,-2.76546470491022));
#45073=CARTESIAN_POINT('Ctrl Pts',(5.96223477282027,14.9585365244006,-2.68736489781825));
#45074=CARTESIAN_POINT('Ctrl Pts',(5.66971282350541,15.0511199847504,-2.613288972184));
#45075=CARTESIAN_POINT('Ctrl Pts',(5.3725988245355,15.1368745061914,-2.54385966649289));
#45076=CARTESIAN_POINT('Ctrl Pts',(5.16122334739288,15.1978827486491,-2.4944656538613));
#45077=CARTESIAN_POINT('Ctrl Pts',(4.94752407483941,15.2554341029525,-2.4474241767453));
#45078=CARTESIAN_POINT('Ctrl Pts',(4.7315875681965,15.3094273221724,-2.4029712482205));
#45079=CARTESIAN_POINT('Ctrl Pts',(4.7256242571508,15.3109184010343,-2.40174363440102));
#45080=CARTESIAN_POINT('Ctrl Pts',(4.71965924273307,15.3124067666448,-2.40051798699696));
#45081=CARTESIAN_POINT('Ctrl Pts',(4.71369252616525,15.3138924170786,-2.39929431020639));
#45082=CARTESIAN_POINT('Ctrl Pts',(4.45978012163924,15.3771139677675,-2.34722099438445));
#45083=CARTESIAN_POINT('Ctrl Pts',(4.20278480382731,15.435420451617,-2.298714158249));
#45084=CARTESIAN_POINT('Ctrl Pts',(3.94288022045684,15.4886619316243,-2.2540814333537));
#45085=CARTESIAN_POINT('Ctrl Pts',(3.80987416504048,15.5159082354349,-2.23124065615838));
#45086=CARTESIAN_POINT('Ctrl Pts',(3.67610656094729,15.541827855014,-2.20941360390684));
#45087=CARTESIAN_POINT('Ctrl Pts',(3.54160298166754,15.5663992231882,-2.18863623548886));
#45088=CARTESIAN_POINT('Ctrl Pts',(3.47435119202767,15.5786849072753,-2.17824755127986));
#45089=CARTESIAN_POINT('Ctrl Pts',(3.40691540524463,15.5906335095712,-2.16812128533049));
#45090=CARTESIAN_POINT('Ctrl Pts',(3.33929900391423,15.6022422426552,-2.15826152779633));
#45091=CARTESIAN_POINT('Ctrl Pts',(3.30549080324904,15.6080466091972,-2.15333164902926));
#45092=CARTESIAN_POINT('Ctrl Pts',(3.27163744877826,15.6137660072614,-2.14846839720879));
#45093=CARTESIAN_POINT('Ctrl Pts',(3.23773936865723,15.6194000821641,-2.14367226990373));
#45094=CARTESIAN_POINT('Ctrl Pts',(3.21152573531064,15.6237569535037,-2.13996338957158));
#45095=CARTESIAN_POINT('Ctrl Pts',(3.18421433654936,15.6282372847887,-2.13614588435894));
#45096=CARTESIAN_POINT('Ctrl Pts',(3.1582898601169,15.63243545858,-2.13256563781385));
#45097=CARTESIAN_POINT('Ctrl Pts',(3.15069017881112,15.6336661404402,-2.13151609944382));
#45098=CARTESIAN_POINT('Ctrl Pts',(3.14320976052125,15.6348728406731,-2.13048673700716));
#45099=CARTESIAN_POINT('Ctrl Pts',(3.1359113824538,15.6360459784053,-2.12948575159818));
#45100=CARTESIAN_POINT('Ctrl Pts',(2.87775719540782,15.6775415565695,-2.0940794500733));
#45101=CARTESIAN_POINT('Ctrl Pts',(2.61837526546646,15.7138739789539,-2.06281531592252));
#45102=CARTESIAN_POINT('Ctrl Pts',(2.35795007230111,15.7450248387696,-2.03590284652233));
#45103=CARTESIAN_POINT('Ctrl Pts',(2.05596056132431,15.7811474304739,-2.00469509978109));
#45104=CARTESIAN_POINT('Ctrl Pts',(1.75256804347705,15.8103033922598,-1.97933798480163));
#45105=CARTESIAN_POINT('Ctrl Pts',(1.44816290506226,15.8324815067107,-1.95997140574192));
#45106=CARTESIAN_POINT('Ctrl Pts',(1.14644744569396,15.8544636586031,-1.94077594692731));
#45107=CARTESIAN_POINT('Ctrl Pts',(0.843736620889954,15.8695907029274,-1.92746554146444));
#45108=CARTESIAN_POINT('Ctrl Pts',(0.540407879657201,15.8778133211475,-1.92020969609162));
#45109=CARTESIAN_POINT('Ctrl Pts',(0.360510778949315,15.8826899614948,-1.91590642584941));
#45110=CARTESIAN_POINT('Ctrl Pts',(0.180396322194014,15.885137313928,-1.91373342287414));
#45111=CARTESIAN_POINT('Ctrl Pts',(0.000144007191481506,15.8851386638734,
-1.91373185548263));
#45112=CARTESIAN_POINT('Ctrl Pts',(9.53315880905156E-5,15.8851386642379,
-1.91373185505937));
#45113=CARTESIAN_POINT('Ctrl Pts',(4.66559746552919E-5,15.885138664424,
-1.91373185479448));
#45114=CARTESIAN_POINT('Ctrl Pts',(-2.01964882728384E-6,15.8851386644318,
-1.91373185468797));
#45115=CARTESIAN_POINT('Ctrl Pts',(-0.298062756534573,15.8851387118627,
-1.91373120245655));
#45116=CARTESIAN_POINT('Ctrl Pts',(-0.595730756791502,15.8784609266372,
-1.91959815322724));
#45117=CARTESIAN_POINT('Ctrl Pts',(-0.892664018370692,15.8651644845163,
-1.93123666047278));
#45118=CARTESIAN_POINT('Ctrl Pts',(-1.12138444999966,15.8549225602372,-1.94020151805242));
#45119=CARTESIAN_POINT('Ctrl Pts',(-1.34966889347301,15.840752819092,-1.95259155229056));
#45120=CARTESIAN_POINT('Ctrl Pts',(-1.57735595186607,15.8226670203481,-1.96837642029373));
#45121=CARTESIAN_POINT('Ctrl Pts',(-1.8383182568047,15.8019380787905,-1.98646816238189));
#45122=CARTESIAN_POINT('Ctrl Pts',(-2.0984992486968,15.7760676159358,-2.00899841000987));
#45123=CARTESIAN_POINT('Ctrl Pts',(-2.35766799609165,15.7450658005388,-2.03581781779785));
#45124=CARTESIAN_POINT('Ctrl Pts',(-2.35834041617024,15.7449853655197,-2.03588740145126));
#45125=CARTESIAN_POINT('Ctrl Pts',(-2.3590128294376,15.7449048959452,-2.03595701398876));
#45126=CARTESIAN_POINT('Ctrl Pts',(-2.35968523589097,15.744824391816,-2.03602665540553));
#45127=CARTESIAN_POINT('Ctrl Pts',(-2.48960318705321,15.7292699135974,-2.04948231178473));
#45128=CARTESIAN_POINT('Ctrl Pts',(-2.61926666928655,15.712425704544,-2.06401477308485));
#45129=CARTESIAN_POINT('Ctrl Pts',(-2.74864747588165,15.6942949274031,-2.07959991770205));
#45130=CARTESIAN_POINT('Ctrl Pts',(-2.81333787917919,15.6852295388327,-2.08739249001066));
#45131=CARTESIAN_POINT('Ctrl Pts',(-2.87795761323466,15.675842495087,-2.09544823158194));
#45132=CARTESIAN_POINT('Ctrl Pts',(-2.94250321346813,15.6661341570901,-2.1037637162872));
#45133=CARTESIAN_POINT('Ctrl Pts',(-2.97477601358486,15.6612799880917,-2.10792145863982));
#45134=CARTESIAN_POINT('Ctrl Pts',(-3.00703028020938,15.6563454946965,-2.11214413667789));
#45135=CARTESIAN_POINT('Ctrl Pts',(-3.03926558210551,15.6513307183264,-2.11643130961707));
#45136=CARTESIAN_POINT('Ctrl Pts',(-3.064364380523,15.6474261524059,-2.11976935465006));
#45137=CARTESIAN_POINT('Ctrl Pts',(-3.08836657723838,15.6436450931043,-2.1229994894086));
#45138=CARTESIAN_POINT('Ctrl Pts',(-3.11380677381553,15.6395860007454,-2.12646439387274));
#45139=CARTESIAN_POINT('Ctrl Pts',(-3.12104034923816,15.6384318527955,-2.12744959254043));
#45140=CARTESIAN_POINT('Ctrl Pts',(-3.12839011457528,15.6372549869322,-2.1284539648356));
#45141=CARTESIAN_POINT('Ctrl Pts',(-3.13591416326753,15.6360455791301,-2.12948586516546));
#45142=CARTESIAN_POINT('Ctrl Pts',(-3.43719649088153,15.5876177695101,-2.1708058174891));
#45143=CARTESIAN_POINT('Ctrl Pts',(-3.73502117399232,15.5324414885685,-2.21754192480206));
#45144=CARTESIAN_POINT('Ctrl Pts',(-4.02908029278226,15.4707748211256,-2.26918834452949));
#45145=CARTESIAN_POINT('Ctrl Pts',(-4.25953208892564,15.4224471435727,-2.30966323352303));
#45146=CARTESIAN_POINT('Ctrl Pts',(-4.48767165484889,15.3701326152782,-2.35315478653788));
#45147=CARTESIAN_POINT('Ctrl Pts',(-4.71335824231695,15.3139426610573,-2.39943616491744));
#45148=CARTESIAN_POINT('Ctrl Pts',(-5.01356244980717,15.2391998025426,-2.46099881546688));
#45149=CARTESIAN_POINT('Ctrl Pts',(-5.3094265767787,15.1576010421758,-2.52749625938663));
#45150=CARTESIAN_POINT('Ctrl Pts',(-5.60075678418667,15.069395087537,-2.59838443704975));
#45151=CARTESIAN_POINT('Ctrl Pts',(-5.8197409198287,15.0030933301364,-2.65166894348975));
#45152=CARTESIAN_POINT('Ctrl Pts',(-6.0361635747021,14.9330577376595,-2.70743518407641));
#45153=CARTESIAN_POINT('Ctrl Pts',(-6.24994452515074,14.8593816330971,-2.76546680377027));
#45154=CARTESIAN_POINT('Ctrl Pts',(-6.2427709657445,15.8383026749575,-3.89994404666797));
#45155=CARTESIAN_POINT('Ctrl Pts',(-6.29815583222613,15.8190276923523,-3.91383371439998));
#45156=CARTESIAN_POINT('Ctrl Pts',(-6.44474178978945,15.7640294246474,-3.96332153595004));
#45157=CARTESIAN_POINT('Ctrl Pts',(-6.66526185116382,15.663015036285,-4.09559797813337));
#45158=CARTESIAN_POINT('Ctrl Pts',(-6.87369342521677,15.5379585762815,-4.31230158072116));
#45159=CARTESIAN_POINT('Ctrl Pts',(-7.01918565228154,15.4153897468304,-4.57079555903126));
#45160=CARTESIAN_POINT('Ctrl Pts',(-7.09651835747178,15.3064823826313,-4.83972908208072));
#45161=CARTESIAN_POINT('Ctrl Pts',(-7.10969900601091,15.2437103395232,-5.01815780639156));
#45162=CARTESIAN_POINT('Ctrl Pts',(-7.10784879018326,15.2163983333452,-5.10154097469548));
#45163=CARTESIAN_POINT('Ctrl Pts',(-6.04395578033757,15.2228359720061,-3.86290031537712));
#45164=CARTESIAN_POINT('Ctrl Pts',(-6.09276946335539,15.2058036729393,-3.87479654436034));
#45165=CARTESIAN_POINT('Ctrl Pts',(-6.22228199032594,15.1570815317897,-3.91732220179018));
#45166=CARTESIAN_POINT('Ctrl Pts',(-6.41829648081485,15.0670943798548,-4.03193268370061));
#45167=CARTESIAN_POINT('Ctrl Pts',(-6.60464058492451,14.9552980626184,-4.22123672601488));
#45168=CARTESIAN_POINT('Ctrl Pts',(-6.73521157215934,14.8457420429051,-4.44829710876009));
#45169=CARTESIAN_POINT('Ctrl Pts',(-6.80469367850032,14.7487886821563,-4.68514860236371));
#45170=CARTESIAN_POINT('Ctrl Pts',(-6.81649571524118,14.6933666369333,-4.84218285847006));
#45171=CARTESIAN_POINT('Ctrl Pts',(-6.81483976787885,14.6694087006988,-4.91540371267267));
#45172=CARTESIAN_POINT('Ctrl Pts',(-6.02805603627548,14.8073272184145,-3.3655266670929));
#45173=CARTESIAN_POINT('Ctrl Pts',(-6.09538291851958,14.7843156654749,-3.38182744412473));
#45174=CARTESIAN_POINT('Ctrl Pts',(-6.27265849572073,14.7191838386095,-3.43975761399766));
#45175=CARTESIAN_POINT('Ctrl Pts',(-6.53595052706497,14.6017994961237,-3.592883556401));
#45176=CARTESIAN_POINT('Ctrl Pts',(-6.78171369715551,14.4589479168646,-3.84041911230593));
#45177=CARTESIAN_POINT('Ctrl Pts',(-6.95183436314053,14.3204156154418,-4.13296218348673));
#45178=CARTESIAN_POINT('Ctrl Pts',(-7.0420260852345,14.1977825871932,-4.43614337260094));
#45179=CARTESIAN_POINT('Ctrl Pts',(-7.05751523271005,14.1268472965378,-4.63782502157415));
#45180=CARTESIAN_POINT('Ctrl Pts',(-7.05533881082366,14.0958150745125,-4.73255226145534));
#45181=CARTESIAN_POINT('Ctrl Pts',(-6.20650782976424,14.8758369048666,-2.74558929006944));
#45182=CARTESIAN_POINT('Ctrl Pts',(-6.30488567809951,14.8426759833281,-2.76970897684925));
#45183=CARTESIAN_POINT('Ctrl Pts',(-6.56239158597099,14.7495682389862,-2.85497534271012));
#45184=CARTESIAN_POINT('Ctrl Pts',(-6.93915150013541,14.584925472277,-3.07670868851015));
#45185=CARTESIAN_POINT('Ctrl Pts',(-7.28557448399626,14.3877425186133,-3.42866438866332));
#45186=CARTESIAN_POINT('Ctrl Pts',(-7.52291531247474,14.1978736014857,-3.83925449985577));
#45187=CARTESIAN_POINT('Ctrl Pts',(-7.64834332641638,14.0293214778286,-4.26225227400094));
#45188=CARTESIAN_POINT('Ctrl Pts',(-7.67008673407683,13.9305172526115,-4.54438303023317));
#45189=CARTESIAN_POINT('Ctrl Pts',(-7.66702779568007,13.8867739926947,-4.67771839241253));
#45190=CARTESIAN_POINT('',(-7.00001043090743,14.7967990244186,-4.92966193641599));
#45191=CARTESIAN_POINT('',(-7.00000027445822,14.5427414083387,-3.16613020376588));
#45192=CARTESIAN_POINT('Ctrl Pts',(-7.,14.7967990243833,-4.92966193665079));
#45193=CARTESIAN_POINT('Ctrl Pts',(-7.,14.7552771220866,-4.82520423675662));
#45194=CARTESIAN_POINT('Ctrl Pts',(-7.,14.7204230598774,-4.73114199069113));
#45195=CARTESIAN_POINT('Ctrl Pts',(-7.,14.6925169059846,-4.64926898759083));
#45196=CARTESIAN_POINT('Ctrl Pts',(-7.,14.6785638290383,-4.60833248604069));
#45197=CARTESIAN_POINT('Ctrl Pts',(-7.,14.6662969026635,-4.5704573646326));
#45198=CARTESIAN_POINT('Ctrl Pts',(-7.,14.65553053564,-4.53589212276887));
#45199=CARTESIAN_POINT('Ctrl Pts',(-7.,14.6501473521282,-4.518609501837));
#45200=CARTESIAN_POINT('Ctrl Pts',(-7.,14.6451376851526,-4.50215438545475));
#45201=CARTESIAN_POINT('Ctrl Pts',(-7.,14.6404714582614,-4.48655657212187));
#45202=CARTESIAN_POINT('Ctrl Pts',(-7.,14.6381383448158,-4.47875766545543));
#45203=CARTESIAN_POINT('Ctrl Pts',(-7.,14.6358910913914,-4.47117308455133));
#45204=CARTESIAN_POINT('Ctrl Pts',(-7.,14.6337256779967,-4.46380634029146));
#45205=CARTESIAN_POINT('Ctrl Pts',(-7.,14.6326429712994,-4.46012296816153));
#45206=CARTESIAN_POINT('Ctrl Pts',(-7.,14.6315807246095,-4.45649405519266));
#45207=CARTESIAN_POINT('Ctrl Pts',(-7.,14.6305384389577,-4.45292002921339));
#45208=CARTESIAN_POINT('Ctrl Pts',(-7.,14.6294961533059,-4.44934600323413));
#45209=CARTESIAN_POINT('Ctrl Pts',(-7.,14.6289683953982,-4.44753506389562));
#45210=CARTESIAN_POINT('Ctrl Pts',(-7.,14.6274709645299,-4.44236303548761));
#45211=CARTESIAN_POINT('Ctrl Pts',(-7.,14.6035120706366,-4.3596105809594));
#45212=CARTESIAN_POINT('Ctrl Pts',(-7.,14.5830405217098,-4.27937746873487));
#45213=CARTESIAN_POINT('Ctrl Pts',(-7.,14.5661444668209,-4.20228869892318));
#45214=CARTESIAN_POINT('Ctrl Pts',(-7.,14.5492484119319,-4.12519992911148));
#45215=CARTESIAN_POINT('Ctrl Pts',(-7.,14.5361344232984,-4.05274778190799));
#45216=CARTESIAN_POINT('Ctrl Pts',(-7.,14.5256556230562,-3.98124889454358));
#45217=CARTESIAN_POINT('Ctrl Pts',(-7.,14.5046980225716,-3.83825111981476));
#45218=CARTESIAN_POINT('Ctrl Pts',(-7.,14.4945186462401,-3.69578424712143));
#45219=CARTESIAN_POINT('Ctrl Pts',(-7.,14.4974035759029,-3.55816691131067));
#45220=CARTESIAN_POINT('Ctrl Pts',(-7.,14.5002885055657,-3.42054957549992));
#45221=CARTESIAN_POINT('Ctrl Pts',(-7.,14.516205703975,-3.28800621878016));
#45222=CARTESIAN_POINT('Ctrl Pts',(-7.,14.542741062884,-3.1661309938642));
#45223=CARTESIAN_POINT('Ctrl Pts',(-6.24994591275502,14.8593863510063,-2.76546768184339));
#45224=CARTESIAN_POINT('Ctrl Pts',(-6.299845029724,14.8421892411351,-2.77901288816629));
#45225=CARTESIAN_POINT('Ctrl Pts',(-6.34871496761958,14.8247258705584,-2.79444809502116));
#45226=CARTESIAN_POINT('Ctrl Pts',(-6.39657992132363,14.8070063190978,-2.81168411646804));
#45227=CARTESIAN_POINT('Ctrl Pts',(-6.42793513327259,14.7953986552708,-2.82297503108932));
#45228=CARTESIAN_POINT('Ctrl Pts',(-6.45885895078646,14.783680793141,-2.83503980941021));
#45229=CARTESIAN_POINT('Ctrl Pts',(-6.48935510410294,14.7718531612462,-2.8478647965535));
#45230=CARTESIAN_POINT('Ctrl Pts',(-6.53665117765749,14.7535098461971,-2.86775489642839));
#45231=CARTESIAN_POINT('Ctrl Pts',(-6.58292000167124,14.7349027780747,-2.88947137235263));
#45232=CARTESIAN_POINT('Ctrl Pts',(-6.62819541826187,14.7160216008304,-2.91297873974637));
#45233=CARTESIAN_POINT('Ctrl Pts',(-6.63503348051049,14.7131699282221,-2.91652911771402));
#45234=CARTESIAN_POINT('Ctrl Pts',(-6.64184883446373,14.7103119908072,-2.92012043062703));
#45235=CARTESIAN_POINT('Ctrl Pts',(-6.64864154341018,14.7074477408645,-2.92375264317202));
#45236=CARTESIAN_POINT('Ctrl Pts',(-6.69594095403225,14.6875032186967,-2.94904468998083));
#45237=CARTESIAN_POINT('Ctrl Pts',(-6.74212292260707,14.6672603945742,-2.97631459532374));
#45238=CARTESIAN_POINT('Ctrl Pts',(-6.78718059541533,14.6467045734034,-3.00556997718216));
#45239=CARTESIAN_POINT('Ctrl Pts',(-6.83223826822359,14.6261487522327,-3.03482535904057));
#45240=CARTESIAN_POINT('Ctrl Pts',(-6.87617231393712,14.605279683737,-3.0660666811726));
#45241=CARTESIAN_POINT('Ctrl Pts',(-6.9189314546316,14.5840807130254,-3.09934282893694));
#45242=CARTESIAN_POINT('Ctrl Pts',(-6.94644683168257,14.5704392398165,-3.12075592886526));
#45243=CARTESIAN_POINT('Ctrl Pts',(-6.97347470733396,14.5566611364393,-3.14301246594803));
#45244=CARTESIAN_POINT('Ctrl Pts',(-7.00000082163496,14.5427407797108,-3.1661291973434));
#45245=CARTESIAN_POINT('Ctrl Pts',(-6.26385534037038,15.8144219619575,-3.90575675456612));
#45246=CARTESIAN_POINT('Ctrl Pts',(-6.30612912668385,15.7872214193081,-3.91762094721362));
#45247=CARTESIAN_POINT('Ctrl Pts',(-6.34794394428928,15.7586530202396,-3.93244141861837));
#45248=CARTESIAN_POINT('Ctrl Pts',(-6.38887221657581,15.7287855297124,-3.95026172552475));
#45249=CARTESIAN_POINT('Ctrl Pts',(-6.43384338942066,15.6959677242225,-3.9698423248822));
#45250=CARTESIAN_POINT('Ctrl Pts',(-6.47774451336698,15.6615808963665,-3.99304561857202));
#45251=CARTESIAN_POINT('Ctrl Pts',(-6.52005083552343,15.6257531868192,-4.0197782938412));
#45252=CARTESIAN_POINT('Ctrl Pts',(-6.53777952313905,15.6107393960151,-4.03098076252246));
#45253=CARTESIAN_POINT('Ctrl Pts',(-6.55522760380306,15.5954728200784,-4.04280298375156));
#45254=CARTESIAN_POINT('Ctrl Pts',(-6.5723539047681,15.5799639707862,-4.05523818474512));
#45255=CARTESIAN_POINT('Ctrl Pts',(-6.58619729733292,15.5674279836271,-4.06528970546332));
#45256=CARTESIAN_POINT('Ctrl Pts',(-6.59983045220702,15.5547337111189,-4.07574174794345));
#45257=CARTESIAN_POINT('Ctrl Pts',(-6.61323081388031,15.5418870223125,-4.08659088585896));
#45258=CARTESIAN_POINT('Ctrl Pts',(-6.64590220353243,15.5105655411489,-4.11304214298688));
#45259=CARTESIAN_POINT('Ctrl Pts',(-6.67719136733343,15.4783372184194,-4.14185401750552));
#45260=CARTESIAN_POINT('Ctrl Pts',(-6.70681950123728,15.4453015233143,-4.17289744569691));
#45261=CARTESIAN_POINT('Ctrl Pts',(-6.72770964444803,15.4220087839183,-4.19478548166891));
#45262=CARTESIAN_POINT('Ctrl Pts',(-6.74777361636949,15.3983149027798,-4.2177828371642));
#45263=CARTESIAN_POINT('Ctrl Pts',(-6.76690562067418,15.3742584345528,-4.24184469883051));
#45264=CARTESIAN_POINT('Ctrl Pts',(-6.77618564902021,15.3625897821995,-4.25351596728547));
#45265=CARTESIAN_POINT('Ctrl Pts',(-6.7852463335436,15.3508358260357,-4.2654377471286));
#45266=CARTESIAN_POINT('Ctrl Pts',(-6.79407487600683,15.3390012936185,-4.27760496147909));
#45267=CARTESIAN_POINT('Ctrl Pts',(-6.79434693680216,15.33863660009,-4.27797990695021));
#45268=CARTESIAN_POINT('Ctrl Pts',(-6.79461877711129,15.338271830059,-4.27835508549851));
#45269=CARTESIAN_POINT('Ctrl Pts',(-6.79489039665138,15.3379069836732,-4.27873049688523));
#45270=CARTESIAN_POINT('Ctrl Pts',(-6.79943331814915,15.3318048141144,-4.2850093693798));
#45271=CARTESIAN_POINT('Ctrl Pts',(-6.80391448952032,15.3256812783291,-4.29135338184373));
#45272=CARTESIAN_POINT('Ctrl Pts',(-6.80833257737852,15.3195370717944,-4.29776142244535));
#45273=CARTESIAN_POINT('Ctrl Pts',(-6.81054162130762,15.3164649685271,-4.30096544274615));
#45274=CARTESIAN_POINT('Ctrl Pts',(-6.81273489404392,15.3133876975829,-4.30418547019675));
#45275=CARTESIAN_POINT('Ctrl Pts',(-6.81491222677554,15.3103053465848,-4.30742136632205));
#45276=CARTESIAN_POINT('Ctrl Pts',(-6.81652751375196,15.3080186582199,-4.30982196444484));
#45277=CARTESIAN_POINT('Ctrl Pts',(-6.8185572820015,15.3051233541833,-4.3128693695528));
#45278=CARTESIAN_POINT('Ctrl Pts',(-6.82005847796644,15.3029677319571,-4.31514418563211));
#45279=CARTESIAN_POINT('Ctrl Pts',(-6.82058082528438,15.3022176743267,-4.31593571725461));
#45280=CARTESIAN_POINT('Ctrl Pts',(-6.82103962524178,15.3015571937407,-4.31663336823083));
#45281=CARTESIAN_POINT('Ctrl Pts',(-6.82139623449801,15.3010431417636,-4.31717652240758));
#45282=CARTESIAN_POINT('Ctrl Pts',(-6.83575184522523,15.2803495395993,-4.33904165851986));
#45283=CARTESIAN_POINT('Ctrl Pts',(-6.85002639055998,15.2584767386076,-4.36258429588056));
#45284=CARTESIAN_POINT('Ctrl Pts',(-6.86393640900324,15.2354494940946,-4.38791385863263));
#45285=CARTESIAN_POINT('Ctrl Pts',(-6.87708940977073,15.2136754492946,-4.41186492380748));
#45286=CARTESIAN_POINT('Ctrl Pts',(-6.88991660004127,15.1908690825995,-4.4374138196626));
#45287=CARTESIAN_POINT('Ctrl Pts',(-6.90213804434222,15.1670684973955,-4.46463760236649));
#45288=CARTESIAN_POINT('Ctrl Pts',(-6.90769940804151,15.15623804992,-4.47702577459544));
#45289=CARTESIAN_POINT('Ctrl Pts',(-6.91313475985191,15.1452019823458,-4.48976053775622));
#45290=CARTESIAN_POINT('Ctrl Pts',(-6.91841457854223,15.1339652658698,-4.50284791920425));
#45291=CARTESIAN_POINT('Ctrl Pts',(-6.92704804648557,15.1155911819904,-4.52424817834588));
#45292=CARTESIAN_POINT('Ctrl Pts',(-6.93526620688473,15.096680157031,-4.54659190807374));
#45293=CARTESIAN_POINT('Ctrl Pts',(-6.94294163519944,15.0772610284527,-4.56988881411136));
#45294=CARTESIAN_POINT('Ctrl Pts',(-6.95237987912846,15.0533819086308,-4.5985363205382));
#45295=CARTESIAN_POINT('Ctrl Pts',(-6.96099870124445,15.0287337634886,-4.62862589435581));
#45296=CARTESIAN_POINT('Ctrl Pts',(-6.96853214143094,15.0033880804351,-4.66015381903064));
#45297=CARTESIAN_POINT('Ctrl Pts',(-6.97439397594545,14.9836663867549,-4.68468596801629));
#45298=CARTESIAN_POINT('Ctrl Pts',(-6.97959814083466,14.9635227136263,-4.71008852577051));
#45299=CARTESIAN_POINT('Ctrl Pts',(-6.98400298712196,14.9430003235828,-4.73634858810239));
#45300=CARTESIAN_POINT('Ctrl Pts',(-6.98927533274534,14.9184362125401,-4.76778036021766));
#45301=CARTESIAN_POINT('Ctrl Pts',(-6.9934029386722,14.8933287532684,-4.8004419443322));
#45302=CARTESIAN_POINT('Ctrl Pts',(-6.99614956570734,14.8677747239439,-4.83426271362839));
#45303=CARTESIAN_POINT('Ctrl Pts',(-6.99865578088694,14.8444574350024,-4.86512315602239));
#45304=CARTESIAN_POINT('Ctrl Pts',(-7.00001226509507,14.8207684317736,-4.89694850040556));
#45305=CARTESIAN_POINT('Ctrl Pts',(-7.00001530551468,14.7967990246409,-4.92966193612583));
#45306=CARTESIAN_POINT('Ctrl Pts',(-6.23412736340852,25.6421127780222,-8.85535177831017));
#45307=CARTESIAN_POINT('Ctrl Pts',(-6.23490266413302,25.3447921922583,-8.44426356616765));
#45308=CARTESIAN_POINT('Ctrl Pts',(-6.23649046053314,24.5993917002302,-7.54006523054698));
#45309=CARTESIAN_POINT('Ctrl Pts',(-6.23803731643754,23.2351603117236,-6.30682882468332));
#45310=CARTESIAN_POINT('Ctrl Pts',(-6.23759012311847,21.554594420239,-5.23225230543038));
#45311=CARTESIAN_POINT('Ctrl Pts',(-6.23570095048077,19.7179583713161,-4.44990267765729));
#45312=CARTESIAN_POINT('Ctrl Pts',(-6.23204712515177,17.7794232167923,-3.98190829741467));
#45313=CARTESIAN_POINT('Ctrl Pts',(-6.22725857217666,16.0460302754405,-3.85975908900695));
#45314=CARTESIAN_POINT('Ctrl Pts',(-6.22399902673659,14.9771463891637,-3.92718775185178));
#45315=CARTESIAN_POINT('Ctrl Pts',(-6.22266349997794,14.5714121948162,-3.97374893451381));
#45316=CARTESIAN_POINT('Ctrl Pts',(-6.72598868298147,25.5461091699583,-8.92473325230161));
#45317=CARTESIAN_POINT('Ctrl Pts',(-6.72668184133724,25.2514068069937,-8.5179410961706));
#45318=CARTESIAN_POINT('Ctrl Pts',(-6.72805010629819,24.5127407420923,-7.62319006625967));
#45319=CARTESIAN_POINT('Ctrl Pts',(-6.72941765802146,23.1617892511338,-6.40302838449347));
#45320=CARTESIAN_POINT('Ctrl Pts',(-6.72902265940225,21.4982103197369,-5.33903582949243));
#45321=CARTESIAN_POINT('Ctrl Pts',(-6.72736659887997,19.680427704485,-4.56367388117981));
#45322=CARTESIAN_POINT('Ctrl Pts',(-6.7241629162859,17.7615692934668,-4.09848834078605));
#45323=CARTESIAN_POINT('Ctrl Pts',(-6.71993204305552,16.0451905586601,-3.97507508254132));
#45324=CARTESIAN_POINT('Ctrl Pts',(-6.71707752304265,14.9863207288799,-4.04020996538142));
#45325=CARTESIAN_POINT('Ctrl Pts',(-6.71588880214766,14.5843404536859,-4.08565613536179));
#45326=CARTESIAN_POINT('Ctrl Pts',(-7.02718524992886,25.2169081072125,-9.16264615230095));
#45327=CARTESIAN_POINT('Ctrl Pts',(-7.02756394516156,24.9320808125448,-8.76993740843315));
#45328=CARTESIAN_POINT('Ctrl Pts',(-7.02824885826503,24.218150878117,-7.90599885534894));
#45329=CARTESIAN_POINT('Ctrl Pts',(-7.0289771823686,22.9136335544715,-6.72847731374345));
#45330=CARTESIAN_POINT('Ctrl Pts',(-7.02876725796423,21.3070974217811,-5.70076816462786));
#45331=CARTESIAN_POINT('Ctrl Pts',(-7.02790271803788,19.5522390185827,-4.95159305632285));
#45332=CARTESIAN_POINT('Ctrl Pts',(-7.02622935620566,17.6995251453896,-4.5011314991558));
#45333=CARTESIAN_POINT('Ctrl Pts',(-7.02397932362077,16.0419195973798,-4.38031971054423));
#45334=CARTESIAN_POINT('Ctrl Pts',(-7.02249264002466,15.018878224234,-4.44215006170692));
#45335=CARTESIAN_POINT('Ctrl Pts',(-7.02184968078489,14.6305433081597,-4.4855945803032));
#45336=CARTESIAN_POINT('Ctrl Pts',(-6.99838063092152,24.807947129522,-9.4582014980152));
#45337=CARTESIAN_POINT('Ctrl Pts',(-6.99835913541704,24.5356483926749,-9.08279986617113));
#45338=CARTESIAN_POINT('Ctrl Pts',(-6.99821532761512,23.8529257690149,-8.25667875130623));
#45339=CARTESIAN_POINT('Ctrl Pts',(-6.99814245713621,22.6063536722315,-7.13149025517221));
#45340=CARTESIAN_POINT('Ctrl Pts',(-6.9981642204857,21.0703299742658,-6.14885260427005));
#45341=CARTESIAN_POINT('Ctrl Pts',(-6.99828069521003,19.3931394797008,-5.43285637063545));
#45342=CARTESIAN_POINT('Ctrl Pts',(-6.9985045739756,17.6222095925353,-5.00216737521387));
#45343=CARTESIAN_POINT('Ctrl Pts',(-6.99873523975645,16.0377422523945,-4.88660480595007));
#45344=CARTESIAN_POINT('Ctrl Pts',(-6.99894168369694,15.0596432996674,-4.94565663341864));
#45345=CARTESIAN_POINT('Ctrl Pts',(-6.99898903543767,14.6884846232875,-4.98714443423185));
#45346=CARTESIAN_POINT('',(-7.00000308919871,24.7867179209017,-9.33251796323064));
#45347=CARTESIAN_POINT('Origin',(-5.99998370356801,24.7867138050937,-9.33252808562228));
#45348=CARTESIAN_POINT('Ctrl Pts',(-7.00001101651655,24.7867134185415,-9.33251828871336));
#45349=CARTESIAN_POINT('Ctrl Pts',(-7.00001786888999,24.6735525722877,-9.17932102897506));
#45350=CARTESIAN_POINT('Ctrl Pts',(-7.00001802523188,24.5580143029184,-9.03121154693793));
#45351=CARTESIAN_POINT('Ctrl Pts',(-7.00001556839463,24.4406111277544,-8.88816531793989));
#45352=CARTESIAN_POINT('Ctrl Pts',(-7.00001306417432,24.3209436913995,-8.74236027066983));
#45353=CARTESIAN_POINT('Ctrl Pts',(-7.0000078435676,24.199338696344,-8.60181555932676));
#45354=CARTESIAN_POINT('Ctrl Pts',(-7.00000354839009,24.0762964133774,-8.466471695584));
#45355=CARTESIAN_POINT('Ctrl Pts',(-7.00000225630901,24.0392826682261,-8.42575737234825));
#45356=CARTESIAN_POINT('Ctrl Pts',(-7.00000104345646,24.0021385728783,-8.38551347172416));
#45357=CARTESIAN_POINT('Ctrl Pts',(-6.99999999753986,23.9648770204239,-8.34573781928481));
#45358=CARTESIAN_POINT('Ctrl Pts',(-6.9999988766632,23.9249449603375,-8.30311147554537));
#45359=CARTESIAN_POINT('Ctrl Pts',(-6.9999979469053,23.8848780062048,-8.26102289425667));
#45360=CARTESIAN_POINT('Ctrl Pts',(-6.9999971808686,23.8446913133936,-8.21946684648591));
#45361=CARTESIAN_POINT('Ctrl Pts',(-6.99999462214768,23.7104594524111,-8.08066105687884));
#45362=CARTESIAN_POINT('Ctrl Pts',(-6.99999387751261,23.5748953627083,-7.94779826807436));
#45363=CARTESIAN_POINT('Ctrl Pts',(-6.99999403436151,23.4385317260012,-7.82067003236729));
#45364=CARTESIAN_POINT('Ctrl Pts',(-6.99999406718201,23.409997754318,-7.79406856026382));
#45365=CARTESIAN_POINT('Ctrl Pts',(-6.99999414004824,23.3814286057908,-7.7677181073587));
#45366=CARTESIAN_POINT('Ctrl Pts',(-6.99999424550307,23.3528288963755,-7.74161665661631));
#45367=CARTESIAN_POINT('Ctrl Pts',(-6.99999432423887,23.3314754804659,-7.72212851687852));
#45368=CARTESIAN_POINT('Ctrl Pts',(-6.99999441864844,23.3106151852605,-7.70323911051233));
#45369=CARTESIAN_POINT('Ctrl Pts',(-6.99999453140734,23.2890698406971,-7.68388257740629));
#45370=CARTESIAN_POINT('Ctrl Pts',(-6.99999463683964,23.2689244221075,-7.66578375050118));
#45371=CARTESIAN_POINT('Ctrl Pts',(-6.99999475849122,23.2481799713201,-7.64727658207253));
#45372=CARTESIAN_POINT('Ctrl Pts',(-6.99999490352849,23.2258462288783,-7.62752044062178));
#45373=CARTESIAN_POINT('Ctrl Pts',(-6.99999520368183,23.1796267491328,-7.58663528301742));
#45374=CARTESIAN_POINT('Ctrl Pts',(-6.99999556267854,23.1331494864943,-7.54621522276226));
#45375=CARTESIAN_POINT('Ctrl Pts',(-6.99999595372392,23.0864243015881,-7.5062613627382));
#45376=CARTESIAN_POINT('Ctrl Pts',(-6.99999673581468,22.9929739317757,-7.42635364269007));
#45377=CARTESIAN_POINT('Ctrl Pts',(-6.99999764539602,22.8985318728929,-7.3483107235662));
#45378=CARTESIAN_POINT('Ctrl Pts',(-6.99999847634363,22.8031748666945,-7.27213985850401));
#45379=CARTESIAN_POINT('Ctrl Pts',(-6.99999902467255,22.7402503163646,-7.22187593324709));
#45380=CARTESIAN_POINT('Ctrl Pts',(-6.99999953898535,22.6769273082929,-7.17242715339307));
#45381=CARTESIAN_POINT('Ctrl Pts',(-6.99999996276667,22.6132273489527,-7.12379520528499));
#45382=CARTESIAN_POINT('Ctrl Pts',(-7.00000126736585,22.41712876638,-6.97408308316544));
#45383=CARTESIAN_POINT('Ctrl Pts',(-7.00000171384891,22.217461340655,-6.83211389992002));
#45384=CARTESIAN_POINT('Ctrl Pts',(-7.00000170643164,22.0149178030739,-6.69789294448405));
#45385=CARTESIAN_POINT('Ctrl Pts',(-7.00000169893506,21.8102086021931,-6.56223685366578));
#45386=CARTESIAN_POINT('Ctrl Pts',(-7.00000122941368,21.6025614301284,-6.43449553455437));
#45387=CARTESIAN_POINT('Ctrl Pts',(-7.00000072342701,21.3926444044191,-6.31464932663616));
#45388=CARTESIAN_POINT('Ctrl Pts',(-7.00000046988867,21.2874597908477,-6.25459713684695));
#45389=CARTESIAN_POINT('Ctrl Pts',(-7.00000020716685,21.1817045351281,-6.19652684959421));
#45390=CARTESIAN_POINT('Ctrl Pts',(-6.9999999876654,21.0754583563051,-6.14043370312219));
#45391=CARTESIAN_POINT('Ctrl Pts',(-6.99999993928893,21.0520424943101,-6.12807119379527));
#45392=CARTESIAN_POINT('Ctrl Pts',(-6.99999989300575,21.0286027758283,-6.11580471396694));
#45393=CARTESIAN_POINT('Ctrl Pts',(-6.99999984878329,21.0051400649146,-6.10363406323595));
#45394=CARTESIAN_POINT('Ctrl Pts',(-6.99999965374504,20.9016603977064,-6.04995676686628));
#45395=CARTESIAN_POINT('Ctrl Pts',(-6.999999498637,20.7977336996679,-5.99814355137489));
#45396=CARTESIAN_POINT('Ctrl Pts',(-6.99999938184612,20.6934324619098,-5.94817675977887));
#45397=CARTESIAN_POINT('Ctrl Pts',(-6.99999932345068,20.6412818430308,-5.92319336398087));
#45398=CARTESIAN_POINT('Ctrl Pts',(-6.99999927466585,20.5890375892218,-5.8986715741567));
#45399=CARTESIAN_POINT('Ctrl Pts',(-6.99999923547398,20.5367084691644,-5.87460910041797));
#45400=CARTESIAN_POINT('Ctrl Pts',(-6.99999921587804,20.5105439091356,-5.86257786354861));
#45401=CARTESIAN_POINT('Ctrl Pts',(-6.99999919868237,20.4843581325447,-5.8506614557006));
#45402=CARTESIAN_POINT('Ctrl Pts',(-6.99999918389672,20.4581522268333,-5.83885958823657));
#45403=CARTESIAN_POINT('Ctrl Pts',(-6.9999991728316,20.4385405337695,-5.83002743395683));
#45404=CARTESIAN_POINT('Ctrl Pts',(-6.99999916268855,20.4179923363439,-5.82084769630923));
#45405=CARTESIAN_POINT('Ctrl Pts',(-6.99999915446007,20.3985848805957,-5.81224565595625));
#45406=CARTESIAN_POINT('Ctrl Pts',(-6.99999915169334,20.3920593404632,-5.80935331600849));
#45407=CARTESIAN_POINT('Ctrl Pts',(-6.99999914913303,20.3856629518266,-5.80652587657329));
#45408=CARTESIAN_POINT('Ctrl Pts',(-6.99999914678765,20.3794752048421,-5.80379731697459));
#45409=CARTESIAN_POINT('Ctrl Pts',(-6.99999907529436,20.1908565103081,-5.72062369162249));
#45410=CARTESIAN_POINT('Ctrl Pts',(-6.99999912491866,19.997467426613,-5.64168479882575));
#45411=CARTESIAN_POINT('Ctrl Pts',(-6.99999933315965,19.7994484267587,-5.56752045890149));
#45412=CARTESIAN_POINT('Ctrl Pts',(-6.99999947285736,19.6666081079875,-5.51776758385295));
#45413=CARTESIAN_POINT('Ctrl Pts',(-6.99999968443231,19.5316850177846,-5.47016399769346));
#45414=CARTESIAN_POINT('Ctrl Pts',(-6.99999998816762,19.3947326008755,-5.42487991153454));
#45415=CARTESIAN_POINT('Ctrl Pts',(-7.00000042903658,19.1959474430728,-5.3591504821735));
#45416=CARTESIAN_POINT('Ctrl Pts',(-7.00000106780694,18.9928846417257,-5.29830694871975));
#45417=CARTESIAN_POINT('Ctrl Pts',(-7.00000153331201,18.7857670354442,-5.2428642781925));
#45418=CARTESIAN_POINT('Ctrl Pts',(-7.00000199134807,18.5819726260479,-5.18831118394662));
#45419=CARTESIAN_POINT('Ctrl Pts',(-7.0000022813202,18.3742524289665,-5.13898704366274));
#45420=CARTESIAN_POINT('Ctrl Pts',(-7.0000020266282,18.1628635746473,-5.0954046588484));
#45421=CARTESIAN_POINT('Ctrl Pts',(-7.00000181209342,17.9848043394636,-5.05869389596303));
#45422=CARTESIAN_POINT('Ctrl Pts',(-7.00000121063125,17.8041428262805,-5.02605738962653));
#45423=CARTESIAN_POINT('Ctrl Pts',(-6.99999998662421,17.6210585944206,-4.99781411446671));
#45424=CARTESIAN_POINT('Ctrl Pts',(-6.99999852881455,17.4030026883872,-4.96417597484234));
#45425=CARTESIAN_POINT('Ctrl Pts',(-6.99999617286851,17.1815088161742,-4.93677017707439));
#45426=CARTESIAN_POINT('Ctrl Pts',(-6.99999449845778,16.9569202000096,-4.91605392211338));
#45427=CARTESIAN_POINT('Ctrl Pts',(-6.99999284826951,16.7355805405395,-4.89563735382567));
#45428=CARTESIAN_POINT('Ctrl Pts',(-6.99999186158928,16.5112349764961,-4.88171820714913));
#45429=CARTESIAN_POINT('Ctrl Pts',(-6.99999320068089,16.2842613693983,-4.8747443371105));
#45430=CARTESIAN_POINT('Ctrl Pts',(-6.9999941339609,16.126072094649,-4.86988389779461));
#45431=CARTESIAN_POINT('Ctrl Pts',(-6.99999620011936,15.9666072927035,-4.86839726412075));
#45432=CARTESIAN_POINT('Ctrl Pts',(-6.99999999965512,15.80600961461,-4.87043896575524));
#45433=CARTESIAN_POINT('Ctrl Pts',(-7.00000506883584,15.5917469503153,-4.87316291816286));
#45434=CARTESIAN_POINT('Ctrl Pts',(-7.00001329849009,15.3754653810258,-4.88216722490851));
#45435=CARTESIAN_POINT('Ctrl Pts',(-7.00001657716831,15.1576281619852,-4.89779630238528));
#45436=CARTESIAN_POINT('Ctrl Pts',(-7.00001838080227,15.037793710345,-4.90639401556449));
#45437=CARTESIAN_POINT('Ctrl Pts',(-7.00001867122265,14.9174893804563,-4.91699659995693));
#45438=CARTESIAN_POINT('Ctrl Pts',(-7.00001598720761,14.7967990242442,-4.92966193645403));
#45439=CARTESIAN_POINT('Origin',(-5.999994980806,24.7867195890732,-9.33250914740904));
#45440=CARTESIAN_POINT('Origin',(-6.,24.7867243677925,-9.33251101143268));
#45441=CARTESIAN_POINT('Ctrl Pts',(-7.1043551019301,14.3540695603781,-7.16139801889706));
#45442=CARTESIAN_POINT('Ctrl Pts',(-7.10505840364598,14.3262466614253,-7.2166440006466));
#45443=CARTESIAN_POINT('Ctrl Pts',(-7.09599870842687,14.250813032227,-7.37231361286277));
#45444=CARTESIAN_POINT('Ctrl Pts',(-7.02992031322268,14.1377144382614,-7.63343902919195));
#45445=CARTESIAN_POINT('Ctrl Pts',(-6.87962835847259,14.0336429995058,-7.92131943416508));
#45446=CARTESIAN_POINT('Ctrl Pts',(-6.66675658014908,13.9662230204584,-8.17059025983369));
#45447=CARTESIAN_POINT('Ctrl Pts',(-6.44849849026614,13.9438645604057,-8.33481728798434));
#45448=CARTESIAN_POINT('Ctrl Pts',(-6.30562810957406,13.9470394167763,-8.40803755460183));
#45449=CARTESIAN_POINT('Ctrl Pts',(-6.25403108440681,13.9502324530738,-8.43056626115595));
#45450=CARTESIAN_POINT('Ctrl Pts',(-6.81769315740398,13.8371643132692,-6.90501019096244));
#45451=CARTESIAN_POINT('Ctrl Pts',(-6.81832491766206,13.8126035966522,-6.95375927642177));
#45452=CARTESIAN_POINT('Ctrl Pts',(-6.81018068214544,13.7460176756343,-7.09142431241616));
#45453=CARTESIAN_POINT('Ctrl Pts',(-6.75054164470443,13.6465473839494,-7.32312337578426));
#45454=CARTESIAN_POINT('Ctrl Pts',(-6.61500606191396,13.5560338595191,-7.57861801524689));
#45455=CARTESIAN_POINT('Ctrl Pts',(-6.42374559388827,13.4986449647106,-7.79929848485672));
#45456=CARTESIAN_POINT('Ctrl Pts',(-6.2287190790081,13.4808603575806,-7.94407139582291));
#45457=CARTESIAN_POINT('Ctrl Pts',(-6.10176442006207,13.4845982242126,-8.00837466920298));
#45458=CARTESIAN_POINT('Ctrl Pts',(-6.05601366185832,13.4876931636193,-8.02813942562704));
#45459=CARTESIAN_POINT('Ctrl Pts',(-7.05994136368923,13.3052082606372,-6.63417610553049));
#45460=CARTESIAN_POINT('Ctrl Pts',(-7.06077434405811,13.2734780527966,-6.69718330261341));
#45461=CARTESIAN_POINT('Ctrl Pts',(-7.05006316137364,13.1877446689244,-6.87408086960113));
#45462=CARTESIAN_POINT('Ctrl Pts',(-6.9726777229904,13.0596165904912,-7.16954064266108));
#45463=CARTESIAN_POINT('Ctrl Pts',(-6.79632560572774,12.9411861766716,-7.4964228042818));
#45464=CARTESIAN_POINT('Ctrl Pts',(-6.5443353497334,12.8637753759665,-7.78232843918036));
#45465=CARTESIAN_POINT('Ctrl Pts',(-6.28263461591015,12.8380285719052,-7.97358623594707));
#45466=CARTESIAN_POINT('Ctrl Pts',(-6.10912624217055,12.8422479165076,-8.0601704519397));
#45467=CARTESIAN_POINT('Ctrl Pts',(-6.04615886818837,12.8462520261003,-8.08697139379655));
#45468=CARTESIAN_POINT('Ctrl Pts',(-7.66740328026631,13.1170710760981,-6.53161011949029));
#45469=CARTESIAN_POINT('Ctrl Pts',(-7.66857435637506,13.0725817013203,-6.62000105264184));
#45470=CARTESIAN_POINT('Ctrl Pts',(-7.65354730602362,12.952637211568,-6.86687204017496));
#45471=CARTESIAN_POINT('Ctrl Pts',(-7.54621409601368,12.7729199260003,-7.2762178468624));
#45472=CARTESIAN_POINT('Ctrl Pts',(-7.30103647553656,12.6039522523028,-7.73004848906578));
#45473=CARTESIAN_POINT('Ctrl Pts',(-6.94698677236901,12.4899890553448,-8.13094481283146));
#45474=CARTESIAN_POINT('Ctrl Pts',(-6.5737315426479,12.4491218575515,-8.40323327799303));
#45475=CARTESIAN_POINT('Ctrl Pts',(-6.32263787429271,12.45341638109,-8.5282493153534));
#45476=CARTESIAN_POINT('Ctrl Pts',(-6.23101741108753,12.4587230728515,-8.56713483649188));
#45477=CARTESIAN_POINT('',(-6.26386059966982,13.9442583573344,-8.42071137120996));
#45478=CARTESIAN_POINT('',(-6.24994560412829,12.4626529248953,-8.55169129771482));
#45479=CARTESIAN_POINT('Ctrl Pts',(-6.26385531438063,13.9442721684155,-8.42069786050422));
#45480=CARTESIAN_POINT('Ctrl Pts',(-6.25431876900276,13.9218692534565,-8.40152732455114));
#45481=CARTESIAN_POINT('Ctrl Pts',(-6.24496566034452,13.898005006553,-8.38292933852713));
#45482=CARTESIAN_POINT('Ctrl Pts',(-6.23589696786197,13.8726957646131,-8.36513250150588));
#45483=CARTESIAN_POINT('Ctrl Pts',(-6.22705466583233,13.8480183415111,-8.34777994396607));
#45484=CARTESIAN_POINT('Ctrl Pts',(-6.2184830520658,13.8219669051049,-8.33118973070111));
#45485=CARTESIAN_POINT('Ctrl Pts',(-6.21028187793343,13.7946047513556,-8.31558229425693));
#45486=CARTESIAN_POINT('Ctrl Pts',(-6.20220717037243,13.7676645369181,-8.3002155329823));
#45487=CARTESIAN_POINT('Ctrl Pts',(-6.19449189366985,13.7394535982295,-8.28580222594987));
#45488=CARTESIAN_POINT('Ctrl Pts',(-6.18723271225038,13.7100825577268,-8.2725504751593));
#45489=CARTESIAN_POINT('Ctrl Pts',(-6.18010114805958,13.6812278634311,-8.25953169164331));
#45490=CARTESIAN_POINT('Ctrl Pts',(-6.1734101242466,13.6512536412055,-8.24763473584261));
#45491=CARTESIAN_POINT('Ctrl Pts',(-6.16724777116303,13.6203134060684,-8.23704356365176));
#45492=CARTESIAN_POINT('Ctrl Pts',(-6.16645167093337,13.6163163082124,-8.23567531446202));
#45493=CARTESIAN_POINT('Ctrl Pts',(-6.16566438487322,13.6123031533829,-8.23432883038793));
#45494=CARTESIAN_POINT('Ctrl Pts',(-6.16488609396448,13.6082743301702,-8.2330044812538));
#45495=CARTESIAN_POINT('Ctrl Pts',(-6.15895413328033,13.5775675332214,-8.22291058588955));
#45496=CARTESIAN_POINT('Ctrl Pts',(-6.15354561085793,13.5459472765254,-8.21410500969514));
#45497=CARTESIAN_POINT('Ctrl Pts',(-6.14873512281968,13.5136094010613,-8.20673556407136));
#45498=CARTESIAN_POINT('Ctrl Pts',(-6.14398626259485,13.4816858104971,-8.19946052941302));
#45499=CARTESIAN_POINT('Ctrl Pts',(-6.13982048464334,13.4490634552977,-8.19358561892249));
#45500=CARTESIAN_POINT('Ctrl Pts',(-6.13629629272268,13.4159660304879,-8.1892190615961));
#45501=CARTESIAN_POINT('Ctrl Pts',(-6.13279279596087,13.3830629641238,-8.18487814606208));
#45502=CARTESIAN_POINT('Ctrl Pts',(-6.12992359196701,13.3496911104767,-8.18202834059126));
#45503=CARTESIAN_POINT('Ctrl Pts',(-6.12772926495945,13.3160956606706,-8.18073484260766));
#45504=CARTESIAN_POINT('Ctrl Pts',(-6.12554238394843,13.2826142101007,-8.17944573384293));
#45505=CARTESIAN_POINT('Ctrl Pts',(-6.12402594639205,13.2489115085795,-8.17970261237211));
#45506=CARTESIAN_POINT('Ctrl Pts',(-6.12320058978627,13.2152439538066,-8.18152417251487));
#45507=CARTESIAN_POINT('Ctrl Pts',(-6.12237597635794,13.181606714375,-8.18334409246671));
#45508=CARTESIAN_POINT('Ctrl Pts',(-6.12224124458969,13.1480054342186,-8.18672588281752));
#45509=CARTESIAN_POINT('Ctrl Pts',(-6.12279604741047,13.1146966651274,-8.19164059249816));
#45510=CARTESIAN_POINT('Ctrl Pts',(-6.12335355350003,13.081225599537,-8.19657924903116));
#45511=CARTESIAN_POINT('Ctrl Pts',(-6.12460728679828,13.048050768882,-8.20306560627659));
#45512=CARTESIAN_POINT('Ctrl Pts',(-6.12653570663021,13.0154201453311,-8.21102355208262));
#45513=CARTESIAN_POINT('Ctrl Pts',(-6.12847158715998,12.9826632799634,-8.21901228570164));
#45514=CARTESIAN_POINT('Ctrl Pts',(-6.13108723330755,12.9504556062705,-8.22848358864234));
#45515=CARTESIAN_POINT('Ctrl Pts',(-6.13434103434159,12.9190231830349,-8.23931820150807));
#45516=CARTESIAN_POINT('Ctrl Pts',(-6.13763222177764,12.8872295990525,-8.25027730483523));
#45517=CARTESIAN_POINT('Ctrl Pts',(-6.14157609014089,12.8562298310844,-8.26263064964509));
#45518=CARTESIAN_POINT('Ctrl Pts',(-6.14611215712109,12.8262216470255,-8.2762192495679));
#45519=CARTESIAN_POINT('Ctrl Pts',(-6.14941594017699,12.8043655918867,-8.28611632259929));
#45520=CARTESIAN_POINT('Ctrl Pts',(-6.15303348114506,12.7830347782143,-8.29666786989227));
#45521=CARTESIAN_POINT('Ctrl Pts',(-6.15693687422531,12.7622912696509,-8.30780374079499));
#45522=CARTESIAN_POINT('Ctrl Pts',(-6.16239173227345,12.7333029273786,-8.32336573872032));
#45523=CARTESIAN_POINT('Ctrl Pts',(-6.16840510191083,12.7054636338093,-8.34006900844475));
#45524=CARTESIAN_POINT('Ctrl Pts',(-6.17489262861964,12.6789001914872,-8.35770723169384));
#45525=CARTESIAN_POINT('Ctrl Pts',(-6.18152856588358,12.6517290761028,-8.37574895208775));
#45526=CARTESIAN_POINT('Ctrl Pts',(-6.18866024944796,12.6258929457347,-8.39476808136235));
#45527=CARTESIAN_POINT('Ctrl Pts',(-6.19619197334983,12.6014736028412,-8.41453721976038));
#45528=CARTESIAN_POINT('Ctrl Pts',(-6.20383525725669,12.5766925602823,-8.43459917892654));
#45529=CARTESIAN_POINT('Ctrl Pts',(-6.21189016673278,12.5533703503877,-8.45543275336067));
#45530=CARTESIAN_POINT('Ctrl Pts',(-6.22025661292607,12.5315387851256,-8.47680583653422));
#45531=CARTESIAN_POINT('Ctrl Pts',(-6.22882371433385,12.509183626296,-8.4986915173495));
#45532=CARTESIAN_POINT('Ctrl Pts',(-6.23771714857315,12.488391076784,-8.52114219668428));
#45533=CARTESIAN_POINT('Ctrl Pts',(-6.24683464861735,12.4691441717878,-8.54392588646561));
#45534=CARTESIAN_POINT('Ctrl Pts',(-6.24786889296593,12.4669608975763,-8.54651035614283));
#45535=CARTESIAN_POINT('Ctrl Pts',(-6.24890602880747,12.4647974632093,-8.54909913490104));
#45536=CARTESIAN_POINT('Ctrl Pts',(-6.24994591367904,12.4626538076691,-8.55169190342477));
#45537=CARTESIAN_POINT('',(-6.99999993308851,12.5220609673846,-8.04448262432736));
#45538=CARTESIAN_POINT('Ctrl Pts',(-6.99999979926552,12.522060623473,-8.04448240338846));
#45539=CARTESIAN_POINT('Ctrl Pts',(-6.97542285739824,12.5160357668641,-8.06874693229243));
#45540=CARTESIAN_POINT('Ctrl Pts',(-6.95040800356331,12.5104440175142,-8.092411446419));
#45541=CARTESIAN_POINT('Ctrl Pts',(-6.92495762901603,12.5052794586727,-8.11549292092594));
#45542=CARTESIAN_POINT('Ctrl Pts',(-6.88589911077916,12.4973534450368,-8.1509159042415));
#45543=CARTESIAN_POINT('Ctrl Pts',(-6.84581661617226,12.4904323745383,-8.18496704826789));
#45544=CARTESIAN_POINT('Ctrl Pts',(-6.80471668547353,12.4845032510779,-8.21769224628849));
#45545=CARTESIAN_POINT('Ctrl Pts',(-6.79363454055424,12.4829045280554,-8.2265162365194));
#45546=CARTESIAN_POINT('Ctrl Pts',(-6.78247820901056,12.4813780594646,-8.23524367399069));
#45547=CARTESIAN_POINT('Ctrl Pts',(-6.77124736772588,12.4799238936921,-8.24387511076992));
#45548=CARTESIAN_POINT('Ctrl Pts',(-6.70998521883027,12.4719916900564,-8.29095799189599));
#45549=CARTESIAN_POINT('Ctrl Pts',(-6.6465178674323,12.4661981270724,-8.33519774227364));
#45550=CARTESIAN_POINT('Ctrl Pts',(-6.5811239193887,12.4625979661439,-8.37641200247287));
#45551=CARTESIAN_POINT('Ctrl Pts',(-6.56109760139874,12.4614954487134,-8.38903350499969));
#45552=CARTESIAN_POINT('Ctrl Pts',(-6.5408902874965,12.4605987859764,-8.4013711331731));
#45553=CARTESIAN_POINT('Ctrl Pts',(-6.52050919424535,12.4599099639518,-8.41341925274955));
#45554=CARTESIAN_POINT('Ctrl Pts',(-6.51186917965474,12.4596179564393,-8.41852672797903));
#45555=CARTESIAN_POINT('Ctrl Pts',(-6.50319799142138,12.459363514444,-8.42358182730049));
#45556=CARTESIAN_POINT('Ctrl Pts',(-6.49449523374268,12.4591467968089,-8.42858461341113));
#45557=CARTESIAN_POINT('Ctrl Pts',(-6.45012191074507,12.4580418043481,-8.45409264801016));
#45558=CARTESIAN_POINT('Ctrl Pts',(-6.40492956497043,12.4579153804756,-8.47824371821814));
#45559=CARTESIAN_POINT('Ctrl Pts',(-6.35888373115315,12.458787611434,-8.50103476438739));
#45560=CARTESIAN_POINT('Ctrl Pts',(-6.32309503968703,12.4594655447467,-8.51874889076804));
#45561=CARTESIAN_POINT('Ctrl Pts',(-6.28679018132058,12.4607472817652,-8.53564077229362));
#45562=CARTESIAN_POINT('Ctrl Pts',(-6.24994591368686,12.462653807653,-8.55169190344427));
#45563=CARTESIAN_POINT('',(-7.00000699063831,13.9486956645825,-6.97707644718775));
#45564=CARTESIAN_POINT('Ctrl Pts',(-7.00000699063831,13.9486956645825,-6.97707644718775));
#45565=CARTESIAN_POINT('Ctrl Pts',(-7.00000696201984,13.9388631272801,-6.98132934556522));
#45566=CARTESIAN_POINT('Ctrl Pts',(-6.99999999999998,13.8939388286958,-7.00116680182805));
#45567=CARTESIAN_POINT('Ctrl Pts',(-6.99999999999998,13.7156828472741,-7.08002168518265));
#45568=CARTESIAN_POINT('Ctrl Pts',(-7.,13.390887431638,-7.2290274543114));
#45569=CARTESIAN_POINT('Ctrl Pts',(-7.,12.8079631824901,-7.66311431918244));
#45570=CARTESIAN_POINT('Ctrl Pts',(-7.,12.6357805654568,-7.86746450612831));
#45571=CARTESIAN_POINT('Ctrl Pts',(-7.,12.5220605681818,-8.04448236787108));
#45572=CARTESIAN_POINT('Ctrl Pts',(-7.00000698845854,13.9487142985806,-6.97711952785195));
#45573=CARTESIAN_POINT('Ctrl Pts',(-7.00000440247537,13.9417124577176,-7.02271343158893));
#45574=CARTESIAN_POINT('Ctrl Pts',(-6.9982617039689,13.9352233858386,-7.06743899796608));
#45575=CARTESIAN_POINT('Ctrl Pts',(-6.99501560109673,13.9292493585815,-7.11111644741427));
#45576=CARTESIAN_POINT('Ctrl Pts',(-6.99400447902474,13.927388520815,-7.12472144852615));
#45577=CARTESIAN_POINT('Ctrl Pts',(-6.99284724471071,13.9255776194665,-7.1382250551963));
#45578=CARTESIAN_POINT('Ctrl Pts',(-6.99155043900581,13.9238166198075,-7.15162262632134));
#45579=CARTESIAN_POINT('Ctrl Pts',(-6.98721566830246,13.9179302100688,-7.19640604961227));
#45580=CARTESIAN_POINT('Ctrl Pts',(-6.98132457884879,13.9126014783713,-7.2400021018724));
#45581=CARTESIAN_POINT('Ctrl Pts',(-6.97415403051326,13.9078036282271,-7.28229317583046));
#45582=CARTESIAN_POINT('Ctrl Pts',(-6.96663085873588,13.9027698359551,-7.32666398251757));
#45583=CARTESIAN_POINT('Ctrl Pts',(-6.95769892916249,13.8983205261988,-7.36959827165777));
#45584=CARTESIAN_POINT('Ctrl Pts',(-6.94763652196407,13.8944217247386,-7.41099935405376));
#45585=CARTESIAN_POINT('Ctrl Pts',(-6.9449082656302,13.8933646288003,-7.42222457710907));
#45586=CARTESIAN_POINT('Ctrl Pts',(-6.94209669584886,13.8923479811363,-7.43333730319684));
#45587=CARTESIAN_POINT('Ctrl Pts',(-6.93920691998523,13.891371053529,-7.4443360722963));
#45588=CARTESIAN_POINT('Ctrl Pts',(-6.93549800688392,13.8901172055586,-7.45845255770426));
#45589=CARTESIAN_POINT('Ctrl Pts',(-6.93166027951993,13.8889287888692,-7.47238130999926));
#45590=CARTESIAN_POINT('Ctrl Pts',(-6.92770413969251,13.8878042041527,-7.48611969781178));
#45591=CARTESIAN_POINT('Ctrl Pts',(-6.91583249176674,13.8844295322757,-7.52734607258448));
#45592=CARTESIAN_POINT('Ctrl Pts',(-6.90289794786343,13.8816295401607,-7.56685615963965));
#45593=CARTESIAN_POINT('Ctrl Pts',(-6.88919659010306,13.8793390685756,-7.60462800461149));
#45594=CARTESIAN_POINT('Ctrl Pts',(-6.87483949860464,13.8769389772345,-7.64420757357169));
#45595=CARTESIAN_POINT('Ctrl Pts',(-6.85964015705107,13.8750984351494,-7.68187857528357));
#45596=CARTESIAN_POINT('Ctrl Pts',(-6.84389294039583,13.8737425403749,-7.71764776642021));
#45597=CARTESIAN_POINT('Ctrl Pts',(-6.84271076881642,13.8736407509411,-7.72033302325676));
#45598=CARTESIAN_POINT('Ctrl Pts',(-6.84152549002593,13.8735416925283,-7.72300757600783));
#45599=CARTESIAN_POINT('Ctrl Pts',(-6.84033721930421,13.8734453332486,-7.72567143426748));
#45600=CARTESIAN_POINT('Ctrl Pts',(-6.83414454227264,13.8729431565244,-7.73955414092537));
#45601=CARTESIAN_POINT('Ctrl Pts',(-6.82787067434591,13.872514290194,-7.75314633620957));
#45602=CARTESIAN_POINT('Ctrl Pts',(-6.82153140754412,13.8721542004677,-7.76644977163411));
#45603=CARTESIAN_POINT('Ctrl Pts',(-6.81836177414322,13.8719741556045,-7.77310148934638));
#45604=CARTESIAN_POINT('Ctrl Pts',(-6.81517578531874,13.8718113078776,-7.77968101442203));
#45605=CARTESIAN_POINT('Ctrl Pts',(-6.81197532766753,13.8716650831134,-7.78618863946136));
#45606=CARTESIAN_POINT('Ctrl Pts',(-6.81037509884193,13.8715919707312,-7.78944245198102));
#45607=CARTESIAN_POINT('Ctrl Pts',(-6.80877125245983,13.8715230142659,-7.79267828933442));
#45608=CARTESIAN_POINT('Ctrl Pts',(-6.80716402087194,13.8714581422824,-7.79589618956667));
#45609=CARTESIAN_POINT('Ctrl Pts',(-6.80578119710739,13.8714023279733,-7.79866479425727));
#45610=CARTESIAN_POINT('Ctrl Pts',(-6.80477551129168,13.8713635671486,-7.80066840713703));
#45611=CARTESIAN_POINT('Ctrl Pts',(-6.80316743052006,13.8713054813963,-7.80384746390922));
#45612=CARTESIAN_POINT('Ctrl Pts',(-6.80290646747114,13.8712960551067,-7.80436336855941));
#45613=CARTESIAN_POINT('Ctrl Pts',(-6.80262955743476,13.871286162908,-7.80491017874213));
#45614=CARTESIAN_POINT('Ctrl Pts',(-6.80233240072437,13.8712757085966,-7.80549611779183));
#45615=CARTESIAN_POINT('Ctrl Pts',(-6.80117192980019,13.8712348819082,-7.80778435563652));
#45616=CARTESIAN_POINT('Ctrl Pts',(-6.80000721951744,13.8711961246117,-7.81006857574347));
#45617=CARTESIAN_POINT('Ctrl Pts',(-6.7988382919471,13.8711594425164,-7.81234875510117));
#45618=CARTESIAN_POINT('Ctrl Pts',(-6.76921159976319,13.8702297278157,-7.87014033575078));
#45619=CARTESIAN_POINT('Ctrl Pts',(-6.73688041703603,13.8706311177965,-7.92533559663938));
#45620=CARTESIAN_POINT('Ctrl Pts',(-6.70230805444698,13.8723877950923,-7.9776628787557));
#45621=CARTESIAN_POINT('Ctrl Pts',(-6.67499636244358,13.8737755460488,-8.0190007135321));
#45622=CARTESIAN_POINT('Ctrl Pts',(-6.64628463556096,13.8760097247121,-8.05854875323045));
#45623=CARTESIAN_POINT('Ctrl Pts',(-6.61638074962212,13.8791106998596,-8.09617745463876));
#45624=CARTESIAN_POINT('Ctrl Pts',(-6.57642476260087,13.8832540584519,-8.14645493055517));
#45625=CARTESIAN_POINT('Ctrl Pts',(-6.53434261580545,13.8889438259581,-8.19330604016633));
#45626=CARTESIAN_POINT('Ctrl Pts',(-6.49070743375913,13.8961521103861,-8.23654095029581));
#45627=CARTESIAN_POINT('Ctrl Pts',(-6.45843664964803,13.9014830607725,-8.26851570977706));
#45628=CARTESIAN_POINT('Ctrl Pts',(-6.42531520566761,13.9076451739511,-8.29851261540396));
#45629=CARTESIAN_POINT('Ctrl Pts',(-6.39155836829281,13.9146333113849,-8.32645867036084));
#45630=CARTESIAN_POINT('Ctrl Pts',(-6.3498114974705,13.9232754974849,-8.36101938270853));
#45631=CARTESIAN_POINT('Ctrl Pts',(-6.30709401505599,13.9331804020228,-8.39244392968853));
#45632=CARTESIAN_POINT('Ctrl Pts',(-6.26385531438063,13.9442721684154,-8.42069786050422));
#45633=CARTESIAN_POINT('Ctrl Pts',(-6.2226671525855,13.113406883036,-7.49367536133247));
#45634=CARTESIAN_POINT('Ctrl Pts',(-6.22400268361015,13.3673812776541,-7.81349762199499));
#45635=CARTESIAN_POINT('Ctrl Pts',(-6.22726226983453,14.0755184331267,-8.61699371744871));
#45636=CARTESIAN_POINT('Ctrl Pts',(-6.23205080008166,15.3875854737378,-9.75631552861892));
#45637=CARTESIAN_POINT('Ctrl Pts',(-6.23570462908324,17.0892588497341,-10.7961449380645));
#45638=CARTESIAN_POINT('Ctrl Pts',(-6.23759379811576,18.9411612581294,-11.5416379309798));
#45639=CARTESIAN_POINT('Ctrl Pts',(-6.23804099158829,20.889340946093,-11.9701370898467));
#45640=CARTESIAN_POINT('Ctrl Pts',(-6.23649414006684,22.7260240230269,-12.0627643382486));
#45641=CARTESIAN_POINT('Ctrl Pts',(-6.2349063534325,23.8924620138941,-11.950478265913));
#45642=CARTESIAN_POINT('Ctrl Pts',(-6.23413106088457,24.393378813603,-11.8700335727714));
#45643=CARTESIAN_POINT('Ctrl Pts',(-6.71588969012869,13.2016799428778,-7.42368590845217));
#45644=CARTESIAN_POINT('Ctrl Pts',(-6.71707840875763,13.4537883131605,-7.74006526921503));
#45645=CARTESIAN_POINT('Ctrl Pts',(-6.71993293840253,14.1564663174282,-8.53485828384865));
#45646=CARTESIAN_POINT('Ctrl Pts',(-6.72416379703351,15.4573961547951,-9.66125530951553));
#45647=CARTESIAN_POINT('Ctrl Pts',(-6.72736747360088,17.1431696324249,-10.6891572004536));
#45648=CARTESIAN_POINT('Ctrl Pts',(-6.7290235300564,18.9767994120935,-11.4262597642551));
#45649=CARTESIAN_POINT('Ctrl Pts',(-6.72941852491458,20.9054833059166,-11.8502312766459));
#45650=CARTESIAN_POINT('Ctrl Pts',(-6.72805098959961,22.7235306892769,-11.9427134310675));
#45651=CARTESIAN_POINT('Ctrl Pts',(-6.7266827144802,23.8785263901091,-11.8323456482745));
#45652=CARTESIAN_POINT('Ctrl Pts',(-6.72598956820625,24.3745540375429,-11.7530873535714));
#45653=CARTESIAN_POINT('Ctrl Pts',(-7.02184866845526,13.5171483052377,-7.17355825144612));
#45654=CARTESIAN_POINT('Ctrl Pts',(-7.02249162233139,13.7610233403838,-7.47887351087227));
#45655=CARTESIAN_POINT('Ctrl Pts',(-7.02397828640646,14.4407034652188,-8.24599533105423));
#45656=CARTESIAN_POINT('Ctrl Pts',(-7.02622832975696,15.698235042491,-9.33267312724308));
#45657=CARTESIAN_POINT('Ctrl Pts',(-7.02790168586848,17.3268260635882,-10.3242153344646));
#45658=CARTESIAN_POINT('Ctrl Pts',(-7.02876622716094,19.0974450740525,-11.0353407644723));
#45659=CARTESIAN_POINT('Ctrl Pts',(-7.02897614585137,20.9601376524492,-11.4446332304759));
#45660=CARTESIAN_POINT('Ctrl Pts',(-7.02824784215516,22.7152003710236,-11.5344326158821));
#45661=CARTESIAN_POINT('Ctrl Pts',(-7.02756289660507,23.8309176062701,-11.4283614102117));
#45662=CARTESIAN_POINT('Ctrl Pts',(-7.02718421187953,24.3100042451047,-11.352078808438));
#45663=CARTESIAN_POINT('Ctrl Pts',(-6.99898915854136,13.9127665113907,-6.85988137561707));
#45664=CARTESIAN_POINT('Ctrl Pts',(-6.9989418013608,14.1458797420746,-7.15166760754954));
#45665=CARTESIAN_POINT('Ctrl Pts',(-6.99873531963908,14.7957455165646,-7.88504566691922));
#45666=CARTESIAN_POINT('Ctrl Pts',(-6.99850468870856,15.9978490959828,-8.92371893442041));
#45667=CARTESIAN_POINT('Ctrl Pts',(-6.99828080917683,17.5546291317113,-9.87141264151665));
#45668=CARTESIAN_POINT('Ctrl Pts',(-6.99816434192788,19.2468680171176,-10.5510797293928));
#45669=CARTESIAN_POINT('Ctrl Pts',(-6.99814257314777,21.0278308193474,-10.9423828250013));
#45670=CARTESIAN_POINT('Ctrl Pts',(-6.99821546033242,22.7049155574539,-11.0282138250255));
#45671=CARTESIAN_POINT('Ctrl Pts',(-6.99835922371807,23.7718253763724,-10.9268166310602));
#45672=CARTESIAN_POINT('Ctrl Pts',(-6.99838072447693,24.2298152718707,-10.8539129111309));
#45673=CARTESIAN_POINT('',(-7.00000355772629,24.1259406808705,-10.9277699389936));
#45674=CARTESIAN_POINT('Ctrl Pts',(-7.00001601631083,13.9487142982008,-6.97711952796313));
#45675=CARTESIAN_POINT('Ctrl Pts',(-7.00002088955871,14.0875642651609,-7.14852826728832));
#45676=CARTESIAN_POINT('Ctrl Pts',(-7.00001598262134,14.2303296025025,-7.31421367370573));
#45677=CARTESIAN_POINT('Ctrl Pts',(-7.00000988115996,14.3764173564029,-7.47407309340898));
#45678=CARTESIAN_POINT('Ctrl Pts',(-7.00000652438907,14.4567887769833,-7.56202111308673));
#45679=CARTESIAN_POINT('Ctrl Pts',(-7.00000279083418,14.5381665194036,-7.6482063638788));
#45680=CARTESIAN_POINT('Ctrl Pts',(-6.9999999996556,14.6204569538272,-7.7326160850522));
#45681=CARTESIAN_POINT('Ctrl Pts',(-6.99999455429067,14.7809989736415,-7.89729266288357));
#45682=CARTESIAN_POINT('Ctrl Pts',(-6.99999266088662,14.945012257854,-8.0552099081169));
#45683=CARTESIAN_POINT('Ctrl Pts',(-6.99999257352113,15.1118864367878,-8.20639691426214));
#45684=CARTESIAN_POINT('Ctrl Pts',(-6.99999248489059,15.2811769408462,-8.35977309649074));
#45685=CARTESIAN_POINT('Ctrl Pts',(-6.99999425322475,15.4534118096271,-8.50622277538367));
#45686=CARTESIAN_POINT('Ctrl Pts',(-6.99999619758536,15.6279986773723,-8.64580626644339));
#45687=CARTESIAN_POINT('Ctrl Pts',(-6.9999975442495,15.7489175403573,-8.74248179105995));
#45688=CARTESIAN_POINT('Ctrl Pts',(-6.99999897835629,15.8709655864557,-8.83586426951038));
#45689=CARTESIAN_POINT('Ctrl Pts',(-6.99999998662344,15.9939582392987,-8.92598173680061));
#45690=CARTESIAN_POINT('Ctrl Pts',(-7.00000143707747,16.1708906990695,-9.05562122978986));
#45691=CARTESIAN_POINT('Ctrl Pts',(-7.00000201440485,16.3497755095874,-9.17850353424194));
#45692=CARTESIAN_POINT('Ctrl Pts',(-7.00000210874344,16.5300313646543,-9.29479362824702));
#45693=CARTESIAN_POINT('Ctrl Pts',(-7.0000022045962,16.7131803904388,-9.41295021970705));
#45694=CARTESIAN_POINT('Ctrl Pts',(-7.0000018021616,16.8977448553806,-9.52430133802055));
#45695=CARTESIAN_POINT('Ctrl Pts',(-7.00000129011705,17.0831663074433,-9.62903785732185));
#45696=CARTESIAN_POINT('Ctrl Pts',(-7.0000008616697,17.2383155596398,-9.7166749266387));
#45697=CARTESIAN_POINT('Ctrl Pts',(-7.000000356192,17.3940657682826,-9.7996812518257));
#45698=CARTESIAN_POINT('Ctrl Pts',(-6.99999998816679,17.5501163155923,-9.87817756443021));
#45699=CARTESIAN_POINT('Ctrl Pts',(-6.99999970373598,17.6707210515928,-9.93884397811405));
#45700=CARTESIAN_POINT('Ctrl Pts',(-6.99999950020172,17.7915056704017,-9.99681676418069));
#45701=CARTESIAN_POINT('Ctrl Pts',(-6.99999936067781,17.9123402394409,-10.052163549305));
#45702=CARTESIAN_POINT('Ctrl Pts',(-6.99999924479288,18.0127022819856,-10.0981331459818));
#45703=CARTESIAN_POINT('Ctrl Pts',(-6.99999917321868,18.1130989356455,-10.1422912225978));
#45704=CARTESIAN_POINT('Ctrl Pts',(-6.99999913936894,18.2134600000256,-10.1846774209558));
#45705=CARTESIAN_POINT('Ctrl Pts',(-6.99999912244407,18.2636405322157,-10.2058705201348));
#45706=CARTESIAN_POINT('Ctrl Pts',(-6.99999911499166,18.3138121670858,-10.2266206497493));
#45707=CARTESIAN_POINT('Ctrl Pts',(-6.99999911640469,18.3639665498459,-10.2469328507477));
#45708=CARTESIAN_POINT('Ctrl Pts',(-6.99999911711121,18.3890437412259,-10.257088951247));
#45709=CARTESIAN_POINT('Ctrl Pts',(-6.99999912003628,18.4141166195784,-10.2671355695921));
#45710=CARTESIAN_POINT('Ctrl Pts',(-6.99999912511624,18.4391841515938,-10.2770733379868));
#45711=CARTESIAN_POINT('Ctrl Pts',(-6.99999912765622,18.4517179176014,-10.2820422221842));
#45712=CARTESIAN_POINT('Ctrl Pts',(-6.99999913073504,18.4642503470248,-10.2869838938939));
#45713=CARTESIAN_POINT('Ctrl Pts',(-6.99999913434545,18.4767813121668,-10.2918984324336));
#45714=CARTESIAN_POINT('Ctrl Pts',(-6.99999913750167,18.4877358965313,-10.2961947277656));
#45715=CARTESIAN_POINT('Ctrl Pts',(-6.99999914057212,18.4972872989131,-10.2999248866138));
#45716=CARTESIAN_POINT('Ctrl Pts',(-6.9999991448373,18.5091124036526,-10.3045195519568));
#45717=CARTESIAN_POINT('Ctrl Pts',(-6.99999914545106,18.5108140535906,-10.3051807310472));
#45718=CARTESIAN_POINT('Ctrl Pts',(-6.99999914609152,18.512562817932,-10.3058597313892));
#45719=CARTESIAN_POINT('Ctrl Pts',(-6.99999914676459,18.5143696874875,-10.3065607279455));
#45720=CARTESIAN_POINT('Ctrl Pts',(-6.99999923697446,18.756538526747,-10.4005130123415));
#45721=CARTESIAN_POINT('Ctrl Pts',(-6.99999952144524,19.0001653869772,-10.4851674521453));
#45722=CARTESIAN_POINT('Ctrl Pts',(-6.9999999901845,19.2445368529083,-10.5606734172128));
#45723=CARTESIAN_POINT('Ctrl Pts',(-7.00000044364536,19.4809431068111,-10.6337182888017));
#45724=CARTESIAN_POINT('Ctrl Pts',(-7.00000106797385,19.7180461077543,-10.6982022220885));
#45725=CARTESIAN_POINT('Ctrl Pts',(-7.00000142593571,19.9551865679679,-10.7543697435462));
#45726=CARTESIAN_POINT('Ctrl Pts',(-7.00000178766101,20.1948202019461,-10.8111277816571));
#45727=CARTESIAN_POINT('Ctrl Pts',(-7.00000187627591,20.4344921235716,-10.8593936415268));
#45728=CARTESIAN_POINT('Ctrl Pts',(-7.00000131558885,20.6735749882544,-10.8994259487503));
#45729=CARTESIAN_POINT('Ctrl Pts',(-7.00000103872944,20.7916307599478,-10.9191933416507));
#45730=CARTESIAN_POINT('Ctrl Pts',(-7.00000060480682,20.9095437108038,-10.9369532860267));
#45731=CARTESIAN_POINT('Ctrl Pts',(-6.99999997635804,21.0272429493937,-10.952737451835));
#45732=CARTESIAN_POINT('Ctrl Pts',(-6.99999887928568,21.2327085093352,-10.9802916017586));
#45733=CARTESIAN_POINT('Ctrl Pts',(-6.99999719588043,21.4375214653267,-11.0018249277698));
#45734=CARTESIAN_POINT('Ctrl Pts',(-6.99999590265544,21.64135379194,-11.017557249433));
#45735=CARTESIAN_POINT('Ctrl Pts',(-6.99999568173141,21.6761748475984,-11.0202448312183));
#45736=CARTESIAN_POINT('Ctrl Pts',(-6.99999546003679,21.7128796212977,-11.0229065687753));
#45737=CARTESIAN_POINT('Ctrl Pts',(-6.99999525389925,21.7501379488206,-11.0254108675337));
#45738=CARTESIAN_POINT('Ctrl Pts',(-6.99999512031343,21.7742829151731,-11.0270337586638));
#45739=CARTESIAN_POINT('Ctrl Pts',(-6.99999499325457,21.7986602566777,-11.0285915188677));
#45740=CARTESIAN_POINT('Ctrl Pts',(-6.99999487632653,21.8229070721095,-11.0300601215468));
#45741=CARTESIAN_POINT('Ctrl Pts',(-6.99999457896569,21.8845693793482,-11.0337949390062));
#45742=CARTESIAN_POINT('Ctrl Pts',(-6.99999434329364,21.9460662483819,-11.0369990609859));
#45743=CARTESIAN_POINT('Ctrl Pts',(-6.99999419422111,22.0073884293069,-11.0396820509392));
#45744=CARTESIAN_POINT('Ctrl Pts',(-6.99999365475363,22.229302706117,-11.0493913236069));
#45745=CARTESIAN_POINT('Ctrl Pts',(-6.99999426201958,22.4489302340576,-11.052275764615));
#45746=CARTESIAN_POINT('Ctrl Pts',(-6.99999708882621,22.6658974946071,-11.0487792497662));
#45747=CARTESIAN_POINT('Ctrl Pts',(-6.99999738657651,22.6887508674568,-11.048410958452));
#45748=CARTESIAN_POINT('Ctrl Pts',(-6.99999770879897,22.7115747727124,-11.0479718660013));
#45749=CARTESIAN_POINT('Ctrl Pts',(-6.99999805663936,22.7343688068517,-11.0474624862398));
#45750=CARTESIAN_POINT('Ctrl Pts',(-6.99999863108817,22.7720125263258,-11.0466212595955));
#45751=CARTESIAN_POINT('Ctrl Pts',(-6.99999927541435,22.8095747740487,-11.0455883343058));
#45752=CARTESIAN_POINT('Ctrl Pts',(-6.99999999465569,22.8470537700766,-11.0443660188129));
#45753=CARTESIAN_POINT('Ctrl Pts',(-7.00000393353181,23.0523049357241,-11.0376720913791));
#45754=CARTESIAN_POINT('Ctrl Pts',(-7.00001006487458,23.2550551876909,-11.025299315509));
#45755=CARTESIAN_POINT('Ctrl Pts',(-7.00001375756537,23.4549607434785,-11.0076804777777));
#45756=CARTESIAN_POINT('Ctrl Pts',(-7.00001750474234,23.6578159341913,-10.9898016715884));
#45757=CARTESIAN_POINT('Ctrl Pts',(-7.00001874207268,23.8577419415626,-10.9665208647451));
#45758=CARTESIAN_POINT('Ctrl Pts',(-7.00001328548954,24.0544307360115,-10.9382749572289));
#45759=CARTESIAN_POINT('Ctrl Pts',(-7.00001262288608,24.0783150372645,-10.934845001973));
#45760=CARTESIAN_POINT('Ctrl Pts',(-7.0000118623437,24.1021516637156,-10.9313418142916));
#45761=CARTESIAN_POINT('Ctrl Pts',(-7.00001099700081,24.1259401133038,-10.9277661612309));
#45762=CARTESIAN_POINT('',(-6.271594443024,24.2690120587724,-11.8794941632625));
#45763=CARTESIAN_POINT('Origin',(-5.99998362344297,24.1259473036637,-10.9277594519388));
#45764=CARTESIAN_POINT('Ctrl Pts',(-6.26386059979505,13.9442583574626,-8.42071137129207));
#45765=CARTESIAN_POINT('Ctrl Pts',(-6.26455151948238,14.1129908023888,-8.59292016862684));
#45766=CARTESIAN_POINT('Ctrl Pts',(-6.26520985509005,14.2852417224813,-8.75834762210823));
#45767=CARTESIAN_POINT('Ctrl Pts',(-6.26583560718918,14.4604060134602,-8.91699520035935));
#45768=CARTESIAN_POINT('Ctrl Pts',(-6.26647066052081,14.6381739613785,-9.07800092972525));
#45769=CARTESIAN_POINT('Ctrl Pts',(-6.26707215449678,14.8189425471099,-9.23202378228874));
#45770=CARTESIAN_POINT('Ctrl Pts',(-6.26764008971406,15.0021229851888,-9.37909727117105));
#45771=CARTESIAN_POINT('Ctrl Pts',(-6.26812468084495,15.1584218251682,-9.50458783088976));
#45772=CARTESIAN_POINT('Ctrl Pts',(-6.26858483996506,15.3164773504787,-9.62501957376955));
#45773=CARTESIAN_POINT('Ctrl Pts',(-6.26902056744525,15.4759481442513,-9.74043079566719));
#45774=CARTESIAN_POINT('Ctrl Pts',(-6.26953467292203,15.6641043019273,-9.87660201267336));
#45775=CARTESIAN_POINT('Ctrl Pts',(-6.27001476678973,15.8542290240486,-10.0057845274972));
#45776=CARTESIAN_POINT('Ctrl Pts',(-6.27046084965745,16.0457324355046,-10.1281576247455));
#45777=CARTESIAN_POINT('Ctrl Pts',(-6.27062083269891,16.1144131682359,-10.1720454799107));
#45778=CARTESIAN_POINT('Ctrl Pts',(-6.2707764411619,16.1832716979968,-10.2150576431113));
#45779=CARTESIAN_POINT('Ctrl Pts',(-6.27092767507453,16.2522823588231,-10.2572028832353));
#45780=CARTESIAN_POINT('Ctrl Pts',(-6.27136815533791,16.4532811528737,-10.3799540978805));
#45781=CARTESIAN_POINT('Ctrl Pts',(-6.27177152493213,16.6555663660736,-10.4953498283191));
#45782=CARTESIAN_POINT('Ctrl Pts',(-6.27213778385719,16.8585418381092,-10.6036186820221));
#45783=CARTESIAN_POINT('Ctrl Pts',(-6.27250404278226,17.0615173101449,-10.7118875357251));
#45784=CARTESIAN_POINT('Ctrl Pts',(-6.27283319103817,17.2651832295118,-10.8130296163902));
#45785=CARTESIAN_POINT('Ctrl Pts',(-6.27312522862493,17.4689977328183,-10.9072900744684));
#45786=CARTESIAN_POINT('Ctrl Pts',(-6.27334042191518,17.6191822143953,-10.9767476341614));
#45787=CARTESIAN_POINT('Ctrl Pts',(-6.27353526444441,17.7691758351741,-11.042347876032));
#45788=CARTESIAN_POINT('Ctrl Pts',(-6.27370997792537,17.9190755664926,-11.1043414616088));
#45789=CARTESIAN_POINT('Ctrl Pts',(-6.27388469140633,18.0689752978111,-11.1663350471856));
#45790=CARTESIAN_POINT('Ctrl Pts',(-6.27403927583901,18.2187815654056,-11.2247220206197));
#45791=CARTESIAN_POINT('Ctrl Pts',(-6.27417395293615,18.3686262123522,-11.2797074204369));
#45792=CARTESIAN_POINT('Ctrl Pts',(-6.27427013778255,18.4756435497946,-11.3189773657205));
#45793=CARTESIAN_POINT('Ctrl Pts',(-6.27435616858698,18.5826811784756,-11.3565113915369));
#45794=CARTESIAN_POINT('Ctrl Pts',(-6.27443212611559,18.6897920788877,-11.3923811462087));
#45795=CARTESIAN_POINT('Ctrl Pts',(-6.27457884520034,18.8966868207852,-11.4616669388422));
#45796=CARTESIAN_POINT('Ctrl Pts',(-6.27469165502992,19.1080560626436,-11.5261457010041));
#45797=CARTESIAN_POINT('Ctrl Pts',(-6.2747705556043,19.323695632466,-11.5853119206409));
#45798=CARTESIAN_POINT('Ctrl Pts',(-6.27484862874894,19.5370737916784,-11.6438576645601));
#45799=CARTESIAN_POINT('Ctrl Pts',(-6.27489350012138,19.7546332935116,-11.6972017097186));
#45800=CARTESIAN_POINT('Ctrl Pts',(-6.27490516972162,19.9761304716923,-11.7448336552605));
#45801=CARTESIAN_POINT('Ctrl Pts',(-6.27491664573162,20.1939531716346,-11.7916754212218));
#45802=CARTESIAN_POINT('Ctrl Pts',(-6.27489601241902,20.4155840381427,-11.8329930159802));
#45803=CARTESIAN_POINT('Ctrl Pts',(-6.2748432697838,20.6407456233376,-11.8682811185367));
#45804=CARTESIAN_POINT('Ctrl Pts',(-6.2747905672207,20.8657361381505,-11.9035424103511));
#45805=CARTESIAN_POINT('Ctrl Pts',(-6.27470580410768,21.0942521822708,-11.9327834027245));
#45806=CARTESIAN_POINT('Ctrl Pts',(-6.27458898044473,21.3259690497801,-11.9554796923451));
#45807=CARTESIAN_POINT('Ctrl Pts',(-6.27454781417929,21.4076213266664,-11.9634773998245));
#45808=CARTESIAN_POINT('Ctrl Pts',(-6.27450266695934,21.4896706048662,-11.9706622567438));
#45809=CARTESIAN_POINT('Ctrl Pts',(-6.27445353877278,21.5721011963913,-11.9770107061708));
#45810=CARTESIAN_POINT('Ctrl Pts',(-6.27431624112677,21.8024684655282,-11.9947526018758));
#45811=CARTESIAN_POINT('Ctrl Pts',(-6.27414785115202,22.0358175823162,-12.0059621193271));
#45812=CARTESIAN_POINT('Ctrl Pts',(-6.2739483685844,22.2717646695394,-12.0102364741364));
#45813=CARTESIAN_POINT('Ctrl Pts',(-6.27375072707306,22.5055341636434,-12.0144713802468));
#45814=CARTESIAN_POINT('Ctrl Pts',(-6.2735225642374,22.7418539878509,-12.0118985196058));
#45815=CARTESIAN_POINT('Ctrl Pts',(-6.27326387982054,22.9803003608198,-12.0021219073502));
#45816=CARTESIAN_POINT('Ctrl Pts',(-6.27300884337127,23.2153841630831,-11.9924831648788));
#45817=CARTESIAN_POINT('Ctrl Pts',(-6.27272414010175,23.4525350029681,-11.975842386317));
#45818=CARTESIAN_POINT('Ctrl Pts',(-6.27240976976577,23.6912965883486,-11.9518163382874));
#45819=CARTESIAN_POINT('Ctrl Pts',(-6.27215746673689,23.8829185840646,-11.9325338424652));
#45820=CARTESIAN_POINT('Ctrl Pts',(-6.27188605477603,24.0755771621085,-11.9084943263574));
#45821=CARTESIAN_POINT('Ctrl Pts',(-6.27159553375594,24.269012168963,-11.8794980525045));
#45822=CARTESIAN_POINT('Origin',(-5.999994993362,24.1259380195517,-10.9277770074801));
#45823=CARTESIAN_POINT('',(-5.98852246661529,25.0410395152426,-11.3308498387572));
#45824=CARTESIAN_POINT('Origin',(-5.999994993362,24.1259380195517,-10.9277770074801));
#45825=CARTESIAN_POINT('Origin',(-6.,24.1259427050578,-10.9277790633915));
#45826=CARTESIAN_POINT('Ctrl Pts',(-5.98841833147186,25.040839013447,-11.3313022800101));
#45827=CARTESIAN_POINT('Ctrl Pts',(-5.98810627263551,25.0938945834088,-11.2108442555191));
#45828=CARTESIAN_POINT('Ctrl Pts',(-5.98726405067241,25.2768814426334,-10.7897532281002));
#45829=CARTESIAN_POINT('Ctrl Pts',(-5.98726405067148,25.5029619533758,-10.243946592786));
#45830=CARTESIAN_POINT('Ctrl Pts',(-5.98810627265534,25.6713270262133,-9.81679902016955));
#45831=CARTESIAN_POINT('Ctrl Pts',(-5.98841833150937,25.7189877605111,-9.69410637652636));
#45832=CARTESIAN_POINT('Ctrl Pts',(-6.58019637618801,25.0471116846997,-11.3340652770895));
#45833=CARTESIAN_POINT('Ctrl Pts',(-6.57988216879889,25.1003453887023,-11.2136609913314));
#45834=CARTESIAN_POINT('Ctrl Pts',(-6.57903377750892,25.283822419077,-10.7926927015325));
#45835=CARTESIAN_POINT('Ctrl Pts',(-6.57903377750808,25.5099484864861,-10.2467760826941));
#45836=CARTESIAN_POINT('Ctrl Pts',(-6.57988216881772,25.6778801673696,-9.81936869533563));
#45837=CARTESIAN_POINT('Ctrl Pts',(-6.58019637622491,25.7253769428462,-9.69658809092832));
#45838=CARTESIAN_POINT('Ctrl Pts',(-7.00079677429206,24.6661026394801,-11.1662377629589));
#45839=CARTESIAN_POINT('Ctrl Pts',(-7.00061248963685,24.71890239789,-11.0471442760213));
#45840=CARTESIAN_POINT('Ctrl Pts',(-7.00011448915271,24.9007955994558,-10.6307100868733));
#45841=CARTESIAN_POINT('Ctrl Pts',(-7.00011448915269,25.1245686196564,-10.0904742265064));
#45842=CARTESIAN_POINT('Ctrl Pts',(-7.00061248964794,25.2904141432989,-9.66739286858448));
#45843=CARTESIAN_POINT('Ctrl Pts',(-7.00079677431321,25.3372908898922,-9.5458459848272));
#45844=CARTESIAN_POINT('Ctrl Pts',(-6.99999917318422,24.1245144806645,-10.927678086825));
#45845=CARTESIAN_POINT('Ctrl Pts',(-6.99999957776486,24.1765264252401,-10.8103725307981));
#45846=CARTESIAN_POINT('Ctrl Pts',(-7.00000004362128,24.355704215903,-10.400186001978));
#45847=CARTESIAN_POINT('Ctrl Pts',(-7.0000000436221,24.5761256622778,-9.86804155660993));
#45848=CARTESIAN_POINT('Ctrl Pts',(-6.99999957776511,24.7394735083832,-9.45129804718199));
#45849=CARTESIAN_POINT('Ctrl Pts',(-6.99999917318346,24.7856430653761,-9.33157249006387));
#45850=CARTESIAN_POINT('Origin',(-5.98852353411045,-11.4730434473617,4.7522901952293));
#45851=CARTESIAN_POINT('Origin',(-7.00021006962827,-11.4504589303418,4.74293534796429));
#45852=CARTESIAN_POINT('Ctrl Pts',(-6.05501399426507,24.9009999601274,-11.6468230574062));
#45853=CARTESIAN_POINT('Ctrl Pts',(-4.03667599617638,24.6398186891149,-12.1728028080739));
#45854=CARTESIAN_POINT('Ctrl Pts',(7.59696227890794E-7,24.4084883660198,
-12.7121777555246));
#45855=CARTESIAN_POINT('Ctrl Pts',(4.03667751556907,24.6398187761839,-12.1728026050588));
#45856=CARTESIAN_POINT('Ctrl Pts',(6.05501627335409,24.901000255044,-11.6468224634765));
#45857=CARTESIAN_POINT('Ctrl Pts',(-6.05501399426507,25.238607264913,-10.8985040433412));
#45858=CARTESIAN_POINT('Ctrl Pts',(-4.03667599617638,25.1429516028745,-11.0707137835862));
#45859=CARTESIAN_POINT('Ctrl Pts',(7.59696227890794E-7,25.1799930233034,
-11.3017734890235));
#45860=CARTESIAN_POINT('Ctrl Pts',(4.03667751556907,25.1429515889299,-11.0707136966136));
#45861=CARTESIAN_POINT('Ctrl Pts',(6.05501627335409,25.2386073729271,-10.8985038488906));
#45862=CARTESIAN_POINT('Ctrl Pts',(-6.05501399426507,25.5530341023971,-10.1393932511011));
#45863=CARTESIAN_POINT('Ctrl Pts',(-4.03667599617638,25.6072779226778,-9.94970177382422));
#45864=CARTESIAN_POINT('Ctrl Pts',(7.59696227453643E-7,25.7969402643708,
-9.81221417039094));
#45865=CARTESIAN_POINT('Ctrl Pts',(4.03667751556907,25.6072778512807,-9.94970182557552));
#45866=CARTESIAN_POINT('Ctrl Pts',(6.05501627335409,25.5530340411425,-10.1393934652993));
#45867=CARTESIAN_POINT('Ctrl Pts',(-6.05501399426507,25.843438717122,-9.3715228581096));
#45868=CARTESIAN_POINT('Ctrl Pts',(-4.03667599617638,26.0307827446463,-8.81463118702198));
#45869=CARTESIAN_POINT('Ctrl Pts',(7.59696227453643E-7,26.2486250668438,
-8.26934400982197));
#45870=CARTESIAN_POINT('Ctrl Pts',(4.03667751556907,26.0307826626489,-8.8146313922699));
#45871=CARTESIAN_POINT('Ctrl Pts',(6.05501627335409,25.8434385055746,-9.37152348694043));
#45872=CARTESIAN_POINT('Ctrl Pts',(-5.98852262876652,25.0410393033093,-11.3308502497276));
#45873=CARTESIAN_POINT('Ctrl Pts',(-5.94974655039506,25.0351515941518,-11.3431133877847));
#45874=CARTESIAN_POINT('Ctrl Pts',(-5.9026883960913,25.0280554837042,-11.3579202581523));
#45875=CARTESIAN_POINT('Ctrl Pts',(-5.84725019583372,25.0198456055148,-11.3751042927631));
#45876=CARTESIAN_POINT('Ctrl Pts',(-5.79793199403674,25.0125420417737,-11.3903913273834));
#45877=CARTESIAN_POINT('Ctrl Pts',(-5.74198182120236,25.0043567201721,-11.4075607859964));
#45878=CARTESIAN_POINT('Ctrl Pts',(-5.6793307029936,24.9953721442677,-11.426465064784));
#45879=CARTESIAN_POINT('Ctrl Pts',(-5.62086562486345,24.9869878736077,-11.4441062524901));
#45880=CARTESIAN_POINT('Ctrl Pts',(-5.55656513515357,24.9779073852414,-11.463258811785));
#45881=CARTESIAN_POINT('Ctrl Pts',(-5.48637318192282,24.9682159074148,-11.4837630384779));
#45882=CARTESIAN_POINT('Ctrl Pts',(-5.42062865300875,24.9591384902058,-11.5029680992096));
#45883=CARTESIAN_POINT('Ctrl Pts',(-5.34971558538561,24.9495249779784,-11.5233592082409));
#45884=CARTESIAN_POINT('Ctrl Pts',(-5.27358792079333,24.9394637661138,-11.5447632446162));
#45885=CARTESIAN_POINT('Ctrl Pts',(-5.23094195729711,24.9338275749052,-11.5567535737406));
#45886=CARTESIAN_POINT('Ctrl Pts',(-5.18665958579444,24.9280512324723,-11.5690609837086));
#45887=CARTESIAN_POINT('Ctrl Pts',(-5.1407327094781,24.9221531728174,-11.5816483787659));
#45888=CARTESIAN_POINT('Ctrl Pts',(-5.08889805502216,24.9154964195459,-11.5958549463713));
#45889=CARTESIAN_POINT('Ctrl Pts',(-5.03496462552337,24.9086806638732,-11.6104269526063));
#45890=CARTESIAN_POINT('Ctrl Pts',(-4.97891809278852,24.9017306812036,-11.6253144892783));
#45891=CARTESIAN_POINT('Ctrl Pts',(-4.97191227619667,24.9008619333698,-11.6271754313623));
#45892=CARTESIAN_POINT('Ctrl Pts',(-4.96487344236937,24.8999910880212,-11.6290413035143));
#45893=CARTESIAN_POINT('Ctrl Pts',(-4.95780155876438,24.8991182004358,-11.6309119924244));
#45894=CARTESIAN_POINT('Ctrl Pts',(-4.95072967515938,24.8982453128505,-11.6327826813344));
#45895=CARTESIAN_POINT('Ctrl Pts',(-4.94968891732262,24.8981176084339,-11.6330565258536));
#45896=CARTESIAN_POINT('Ctrl Pts',(-4.94641137045497,24.8977141068387,-11.6339214872236));
#45897=CARTESIAN_POINT('Ctrl Pts',(-4.93985627671968,24.8969071036484,-11.6356514099635));
#45898=CARTESIAN_POINT('Ctrl Pts',(-4.93317300322536,24.8960861509461,-11.6374116051909));
#45899=CARTESIAN_POINT('Ctrl Pts',(-4.92636142104071,24.8952514565616,-11.6392016654597));
#45900=CARTESIAN_POINT('Ctrl Pts',(-4.91273825667142,24.8935820677926,-11.6427817859974));
#45901=CARTESIAN_POINT('Ctrl Pts',(-4.89860185754123,24.891857712009,-11.6464813665709));
#45902=CARTESIAN_POINT('Ctrl Pts',(-4.88395129397506,24.8900798204547,-11.6502976733481));
#45903=CARTESIAN_POINT('Ctrl Pts',(-4.82889198736725,24.8833982019791,-11.6646400025022));
#45904=CARTESIAN_POINT('Ctrl Pts',(-4.76657070444679,24.8759606415624,-11.6806303902859));
#45905=CARTESIAN_POINT('Ctrl Pts',(-4.69692567007587,24.8678685078306,-11.6980688734675));
#45906=CARTESIAN_POINT('Ctrl Pts',(-4.69244416228836,24.8673477964739,-11.6991910022579));
#45907=CARTESIAN_POINT('Ctrl Pts',(-4.68793232944609,24.866824382464,-11.7003191105458));
#45908=CARTESIAN_POINT('Ctrl Pts',(-4.68339015508959,24.8662982960782,-11.7014531379833));
#45909=CARTESIAN_POINT('Ctrl Pts',(-4.61719643682191,24.8586315683679,-11.7179794724683));
#45910=CARTESIAN_POINT('Ctrl Pts',(-4.54455890139893,24.8503959953999,-11.7357657894902));
#45911=CARTESIAN_POINT('Ctrl Pts',(-4.46541859029337,24.8416948429548,-11.7546040661354));
#45912=CARTESIAN_POINT('Ctrl Pts',(-4.45473449345366,24.8405201703507,-11.7571472703401));
#45913=CARTESIAN_POINT('Ctrl Pts',(-4.44393188009192,24.8393370441802,-11.7597095757516));
#45914=CARTESIAN_POINT('Ctrl Pts',(-4.43301060514178,24.8381457490915,-11.7622904018907));
#45915=CARTESIAN_POINT('Ctrl Pts',(-4.38710138739875,24.8331379614591,-11.773139291761));
#45916=CARTESIAN_POINT('Ctrl Pts',(-4.33909521834272,24.8279855675989,-11.7843160329874));
#45917=CARTESIAN_POINT('Ctrl Pts',(-4.28898063287715,24.822710589797,-11.7957754509205));
#45918=CARTESIAN_POINT('Ctrl Pts',(-4.26392334014436,24.820073100896,-11.801505159887));
#45919=CARTESIAN_POINT('Ctrl Pts',(-4.23833894330931,24.8174049645217,-11.8073055373451));
#45920=CARTESIAN_POINT('Ctrl Pts',(-4.21222597316621,24.8147091518377,-11.8131704340925));
#45921=CARTESIAN_POINT('Ctrl Pts',(-4.19916948809466,24.8133612454958,-11.8161028824662));
#45922=CARTESIAN_POINT('Ctrl Pts',(-4.18598085969634,24.8120064199622,-11.8190514606104));
#45923=CARTESIAN_POINT('Ctrl Pts',(-4.17265990426549,24.8106450525724,-11.8220153849909));
#45924=CARTESIAN_POINT('Ctrl Pts',(-4.16599942655006,24.8099643688776,-11.8234973471811));
#45925=CARTESIAN_POINT('Ctrl Pts',(-4.15930586707652,24.8092820497102,-11.8249831459266));
#45926=CARTESIAN_POINT('Ctrl Pts',(-4.15257920279502,24.8085981430141,-11.8264726814627));
#45927=CARTESIAN_POINT('Ctrl Pts',(-4.14585253851352,24.807914236318,-11.8279622169988));
#45928=CARTESIAN_POINT('Ctrl Pts',(-4.13787834775704,24.8071059154165,-11.8297231040874));
#45929=CARTESIAN_POINT('Ctrl Pts',(-4.13229987245898,24.8065417084999,-11.8309523981142));
#45930=CARTESIAN_POINT('Ctrl Pts',(-4.01426669075566,24.7946038340917,-11.8569626388121));
#45931=CARTESIAN_POINT('Ctrl Pts',(-3.89866246854569,24.7834250122886,-11.8814033178166));
#45932=CARTESIAN_POINT('Ctrl Pts',(-3.78553934540173,24.7729414085328,-11.904385539706));
#45933=CARTESIAN_POINT('Ctrl Pts',(-3.72757714111731,24.7675698031028,-11.9161612068114));
#45934=CARTESIAN_POINT('Ctrl Pts',(-3.67026631188076,24.7623803834644,-11.9275548269377));
#45935=CARTESIAN_POINT('Ctrl Pts',(-3.613613871405,24.7573626209778,-11.9385861494722));
#45936=CARTESIAN_POINT('Ctrl Pts',(-3.53000420327667,24.7499572302704,-11.9548665640205));
#45937=CARTESIAN_POINT('Ctrl Pts',(-3.44782800787335,24.7429278580583,-11.9703532324538));
#45938=CARTESIAN_POINT('Ctrl Pts',(-3.36710459626749,24.7362465183607,-11.9850985588426));
#45939=CARTESIAN_POINT('Ctrl Pts',(-3.32674289046455,24.7329058485118,-11.992471222037));
#45940=CARTESIAN_POINT('Ctrl Pts',(-3.28674438064314,24.7296521961897,-11.9996585541475));
#45941=CARTESIAN_POINT('Ctrl Pts',(-3.2471112461582,24.7264821808726,-12.0066669927124));
#45942=CARTESIAN_POINT('Ctrl Pts',(-3.21205403780241,24.7236781662796,-12.0128662573987));
#45943=CARTESIAN_POINT('Ctrl Pts',(-3.17869660210454,24.721049366133,-12.0186825053255));
#45944=CARTESIAN_POINT('Ctrl Pts',(-3.14328848633031,24.7183020793255,-12.0247653281962));
#45945=CARTESIAN_POINT('Ctrl Pts',(-3.13866675716948,24.7179434831316,-12.0255593032278));
#45946=CARTESIAN_POINT('Ctrl Pts',(-3.13401008974949,24.717582899303,-12.0263577545565));
#45947=CARTESIAN_POINT('Ctrl Pts',(-3.12931014363493,24.7172197033507,-12.0271620661654));
#45948=CARTESIAN_POINT('Ctrl Pts',(-2.9664809447597,24.7046368131405,-12.0550273675416));
#45949=CARTESIAN_POINT('Ctrl Pts',(-2.80321460461108,24.6930123547265,-12.0808729408053));
#45950=CARTESIAN_POINT('Ctrl Pts',(-2.63956869903732,24.6823481561796,-12.1046611143612));
#45951=CARTESIAN_POINT('Ctrl Pts',(-2.55774574625044,24.6770160569062,-12.1165552011391));
#45952=CARTESIAN_POINT('Ctrl Pts',(-2.47582807006359,24.6719238730238,-12.1279352771598));
#45953=CARTESIAN_POINT('Ctrl Pts',(-2.3938232040891,24.6670715572768,-12.1387972933987));
#45954=CARTESIAN_POINT('Ctrl Pts',(-2.35282077110186,24.6646453994033,-12.1442283015181));
#45955=CARTESIAN_POINT('Ctrl Pts',(-2.31179654066698,24.6622792086921,-12.1495297947366));
#45956=CARTESIAN_POINT('Ctrl Pts',(-2.27075145561316,24.6599729795422,-12.1547012663989));
#45957=CARTESIAN_POINT('Ctrl Pts',(-2.23483700619106,24.6579550290361,-12.1592263041033));
#45958=CARTESIAN_POINT('Ctrl Pts',(-2.19890658995127,24.6559829866123,-12.1636517940586));
#45959=CARTESIAN_POINT('Ctrl Pts',(-2.16296083870178,24.6540568481957,-12.1679773965549));
#45960=CARTESIAN_POINT('Ctrl Pts',(-2.15782573138042,24.6537816855648,-12.1685953397687));
#45961=CARTESIAN_POINT('Ctrl Pts',(-2.15064935716421,24.6533988539371,-12.1694551961909));
#45962=CARTESIAN_POINT('Ctrl Pts',(-2.14755457971117,24.653234170739,-12.1698251096412));
#45963=CARTESIAN_POINT('Ctrl Pts',(-2.0717107903665,24.6491982754368,-12.1788905879287));
#45964=CARTESIAN_POINT('Ctrl Pts',(-1.98853406098885,24.6450197213633,-12.1882987669993));
#45965=CARTESIAN_POINT('Ctrl Pts',(-1.89799855360911,24.6408291651433,-12.1977613756536));
#45966=CARTESIAN_POINT('Ctrl Pts',(-1.80788627331092,24.636658198551,-12.2071797493734));
#45967=CARTESIAN_POINT('Ctrl Pts',(-1.71048385448022,24.6324753978846,-12.2166521123484));
#45968=CARTESIAN_POINT('Ctrl Pts',(-1.6057658198115,24.6284288416531,-12.2258461731663));
#45969=CARTESIAN_POINT('Ctrl Pts',(-1.54093857958377,24.6259237614752,-12.2315378918009));
#45970=CARTESIAN_POINT('Ctrl Pts',(-1.47330769454403,24.6234712769607,-12.2371219973271));
#45971=CARTESIAN_POINT('Ctrl Pts',(-1.40286712017468,24.6211100263704,-12.2425102693972));
#45972=CARTESIAN_POINT('Ctrl Pts',(-1.28740839052695,24.6172397144659,-12.2513421543411));
#45973=CARTESIAN_POINT('Ctrl Pts',(-1.16440226992658,24.6136137121762,-12.2596505485663));
#45974=CARTESIAN_POINT('Ctrl Pts',(-1.0338383390704,24.6104187896776,-12.2670000215224));
#45975=CARTESIAN_POINT('Ctrl Pts',(-0.995600257807905,24.6094830970608,
-12.2691524516942));
#45976=CARTESIAN_POINT('Ctrl Pts',(-0.956713927726055,24.6085844808045,
-12.2712223053479));
#45977=CARTESIAN_POINT('Ctrl Pts',(-0.917179087092564,24.607727867909,-12.2731978396645));
#45978=CARTESIAN_POINT('Ctrl Pts',(-0.829915808871143,24.6058371090687,
-12.2775583378465));
#45979=CARTESIAN_POINT('Ctrl Pts',(-0.739493571338707,24.6041509962435,
-12.2814596062158));
#45980=CARTESIAN_POINT('Ctrl Pts',(-0.645913648560607,24.6027251256842,
-12.2847669497706));
#45981=CARTESIAN_POINT('Ctrl Pts',(-0.599123687171559,24.6020121904045,
-12.2864206215479));
#45982=CARTESIAN_POINT('Ctrl Pts',(-0.551544304326092,24.6013642873024,
-12.2879257980049));
#45983=CARTESIAN_POINT('Ctrl Pts',(-0.503176821229749,24.6007886184522,
-12.2892646616672));
#45984=CARTESIAN_POINT('Ctrl Pts',(-0.478993079681576,24.6005007840271,
-12.2899340934983));
#45985=CARTESIAN_POINT('Ctrl Pts',(-0.454612313067827,24.600231006085,-12.2905619460855));
#45986=CARTESIAN_POINT('Ctrl Pts',(-0.430034768691489,24.599980179451,-12.2911459699869));
#45987=CARTESIAN_POINT('Ctrl Pts',(-0.417745996503321,24.5998547661339,
-12.2914379819376));
#45988=CARTESIAN_POINT('Ctrl Pts',(-0.405408029874993,24.5997340905027,
-12.2917190366455));
#45989=CARTESIAN_POINT('Ctrl Pts',(-0.393020899026227,24.5996182655297,
-12.2919888485103));
#45990=CARTESIAN_POINT('Ctrl Pts',(-0.386827333601843,24.5995603530432,
-12.2921237544427));
#45991=CARTESIAN_POINT('Ctrl Pts',(-0.380621477122377,24.5995036532121,
-12.2922558496597));
#45992=CARTESIAN_POINT('Ctrl Pts',(-0.374403333613394,24.5994481802028,
-12.2923850982298));
#45993=CARTESIAN_POINT('Ctrl Pts',(-0.36818519010441,24.5993927071935,-12.2925143467999));
#45994=CARTESIAN_POINT('Ctrl Pts',(-0.359951179428822,24.5993214491376,
-12.2926803918735));
#45995=CARTESIAN_POINT('Ctrl Pts',(-0.355712046080024,24.5992854558015,
-12.2927642679839));
#45996=CARTESIAN_POINT('Ctrl Pts',(-0.236619694947637,24.5982742748198,
-12.2951206466052));
#45997=CARTESIAN_POINT('Ctrl Pts',(-0.118036480863534,24.5977738841301,
-12.2962957273024));
#45998=CARTESIAN_POINT('Ctrl Pts',(4.36983782492462E-13,24.5977653883777,
-12.296312723946));
#45999=CARTESIAN_POINT('Ctrl Pts',(0.150862673191552,24.5977545299388,-12.2963344473919));
#46000=CARTESIAN_POINT('Ctrl Pts',(0.300832233086994,24.5985476990758,-12.294463969907));
#46001=CARTESIAN_POINT('Ctrl Pts',(0.449830184999458,24.6001291281758,-12.2907805068968));
#46002=CARTESIAN_POINT('Ctrl Pts',(0.58261791299645,24.6015385057845,-12.2874977860406));
#46003=CARTESIAN_POINT('Ctrl Pts',(0.714638276046149,24.6035753943051,-12.28277203577));
#46004=CARTESIAN_POINT('Ctrl Pts',(0.845857318554737,24.6062301793636,-12.2766505732036));
#46005=CARTESIAN_POINT('Ctrl Pts',(0.911466839809031,24.6075575718929,-12.2735898419204));
#46006=CARTESIAN_POINT('Ctrl Pts',(0.97687603055194,24.6090394082341,-12.2701801674416));
#46007=CARTESIAN_POINT('Ctrl Pts',(1.04208087787506,24.6106743255165,-12.2664273684045));
#46008=CARTESIAN_POINT('Ctrl Pts',(1.07468330153662,24.6114917841576,-12.2645509688859));
#46009=CARTESIAN_POINT('Ctrl Pts',(1.10723463932392,24.6123475114073,-12.2625887874429));
#46010=CARTESIAN_POINT('Ctrl Pts',(1.1397343959841,24.6132413277545,-12.2605415464827));
#46011=CARTESIAN_POINT('Ctrl Pts',(1.15598427431419,24.6136882359282,-12.2595179260026));
#46012=CARTESIAN_POINT('Ctrl Pts',(1.17222125736142,24.6141446662819,-12.2584730405988));
#46013=CARTESIAN_POINT('Ctrl Pts',(1.18844528400384,24.6146105958455,-12.257406980262));
#46014=CARTESIAN_POINT('Ctrl Pts',(1.19655729732504,24.6148435606272,-12.2568739500935));
#46015=CARTESIAN_POINT('Ctrl Pts',(1.20466607154499,24.6150789002057,-12.2563356261892));
#46016=CARTESIAN_POINT('Ctrl Pts',(1.21277159907198,24.6153166116882,-12.2557920197572));
#46017=CARTESIAN_POINT('Ctrl Pts',(1.21682436283548,24.6154354674294,-12.2555202165412));
#46018=CARTESIAN_POINT('Ctrl Pts',(1.22087631492573,24.6155549161463,-12.2552470926931));
#46019=CARTESIAN_POINT('Ctrl Pts',(1.22492745439972,24.6156749574131,-12.2549726497381));
#46020=CARTESIAN_POINT('Ctrl Pts',(1.22695302413672,24.6157349780466,-12.2548354282606));
#46021=CARTESIAN_POINT('Ctrl Pts',(1.22897839071965,24.6157951468175,-12.2546978770064));
#46022=CARTESIAN_POINT('Ctrl Pts',(1.2310035540316,24.6158554636566,-12.2545599961983));
#46023=CARTESIAN_POINT('Ctrl Pts',(1.23302871734353,24.6159157804956,-12.2544221153902));
#46024=CARTESIAN_POINT('Ctrl Pts',(1.23643078757501,24.6160174704414,-12.2541896791548));
#46025=CARTESIAN_POINT('Ctrl Pts',(1.23707843403692,24.6160368583227,-12.2541453653075));
#46026=CARTESIAN_POINT('Ctrl Pts',(1.27880639131658,24.6172860223795,-12.2512902175771));
#46027=CARTESIAN_POINT('Ctrl Pts',(1.3294741638359,24.618853278113,-12.2477083113246));
#46028=CARTESIAN_POINT('Ctrl Pts',(1.38903584785586,24.6208543134989,-12.2431466992377));
#46029=CARTESIAN_POINT('Ctrl Pts',(1.45025678814527,24.6229110932877,-12.2384580107665));
#46030=CARTESIAN_POINT('Ctrl Pts',(1.52087407136146,24.6254261982142,-12.2327340521914));
#46031=CARTESIAN_POINT('Ctrl Pts',(1.60083784957267,24.6285488023689,-12.2256478324131));
#46032=CARTESIAN_POINT('Ctrl Pts',(1.68763009550311,24.6319380597778,-12.2179564883637));
#46033=CARTESIAN_POINT('Ctrl Pts',(1.7854332718843,24.6360429187669,-12.2086601522125));
#46034=CARTESIAN_POINT('Ctrl Pts',(1.89418363901753,24.6410822169797,-12.1972817179609));
#46035=CARTESIAN_POINT('Ctrl Pts',(1.97507214192233,24.6448304460558,-12.1888184406749));
#46036=CARTESIAN_POINT('Ctrl Pts',(2.06201704854094,24.6490962947508,-12.1792018218676));
#46037=CARTESIAN_POINT('Ctrl Pts',(2.15499213008654,24.6539785207663,-12.168219356019));
#46038=CARTESIAN_POINT('Ctrl Pts',(2.28380963126724,24.6607428725159,-12.1530030874888));
#46039=CARTESIAN_POINT('Ctrl Pts',(2.42418371072383,24.6687031512469,-12.1351384975467));
#46040=CARTESIAN_POINT('Ctrl Pts',(2.57592898429611,24.6782383673289,-12.1138309581078));
#46041=CARTESIAN_POINT('Ctrl Pts',(2.68639476604679,24.6851797044386,-12.0983197402234));
#46042=CARTESIAN_POINT('Ctrl Pts',(2.8028865775025,24.6929558858114,-12.0809834737766));
#46043=CARTESIAN_POINT('Ctrl Pts',(2.92533290147752,24.7017077540705,-12.0615333397425));
#46044=CARTESIAN_POINT('Ctrl Pts',(3.04038690825321,24.7099312554162,-12.0432574472511));
#46045=CARTESIAN_POINT('Ctrl Pts',(3.16069310575817,24.7190216168601,-12.0231039149372));
#46046=CARTESIAN_POINT('Ctrl Pts',(3.28616259950354,24.7291241165009,-12.0007808188169));
#46047=CARTESIAN_POINT('Ctrl Pts',(3.31917344125611,24.731782069498,-11.9949076446177));
#46048=CARTESIAN_POINT('Ctrl Pts',(3.3525416907452,24.7345099845977,-11.9888845436361));
#46049=CARTESIAN_POINT('Ctrl Pts',(3.38626572903287,24.737310278026,-11.9827067940583));
#46050=CARTESIAN_POINT('Ctrl Pts',(3.4672178741226,24.744032182383,-11.967877547457));
#46051=CARTESIAN_POINT('Ctrl Pts',(3.5502193955923,24.7511726072005,-11.9521539542066));
#46052=CARTESIAN_POINT('Ctrl Pts',(3.63524342703742,24.758770261966,-11.9354607867723));
#46053=CARTESIAN_POINT('Ctrl Pts',(3.67775544275998,24.7625690893488,-11.9271142030551));
#46054=CARTESIAN_POINT('Ctrl Pts',(3.72077308600985,24.7664822359632,-11.9185252313042));
#46055=CARTESIAN_POINT('Ctrl Pts',(3.76429261860533,24.7705147554021,-11.9096842161446));
#46056=CARTESIAN_POINT('Ctrl Pts',(3.78605238490307,24.7725310151215,-11.9052637085649));
#46057=CARTESIAN_POINT('Ctrl Pts',(3.80793762353956,24.7745771189329,-11.9007801905478));
#46058=CARTESIAN_POINT('Ctrl Pts',(3.82994785495516,24.7766537073945,-11.896232451032));
#46059=CARTESIAN_POINT('Ctrl Pts',(3.84095297066295,24.7776920016253,-11.8939585812741));
#46060=CARTESIAN_POINT('Ctrl Pts',(3.85198933456561,24.7787379170807,-11.8916686561703));
#46061=CARTESIAN_POINT('Ctrl Pts',(3.86305688536165,24.7797915346484,-11.8893625235876));
#46062=CARTESIAN_POINT('Ctrl Pts',(3.86859066075967,24.7803183434323,-11.8882094572963));
#46063=CARTESIAN_POINT('Ctrl Pts',(3.87413223288104,24.7808470777483,-11.8870523391372));
#46064=CARTESIAN_POINT('Ctrl Pts',(3.87968159397177,24.7813777477599,-11.885891150046));
#46065=CARTESIAN_POINT('Ctrl Pts',(3.88523095506251,24.7819084177716,-11.8847299609548));
#46066=CARTESIAN_POINT('Ctrl Pts',(3.89297592965654,24.7826511797274,-11.8831049768951));
#46067=CARTESIAN_POINT('Ctrl Pts',(3.89635303637021,24.7829755750705,-11.8823953509024));
#46068=CARTESIAN_POINT('Ctrl Pts',(4.05455253139167,24.7981717722322,-11.8491531458965));
#46069=CARTESIAN_POINT('Ctrl Pts',(4.20702419525135,24.8137844834955,-11.8151348605723));
#46070=CARTESIAN_POINT('Ctrl Pts',(4.35383993702875,24.8296204514967,-11.7807734023157));
#46071=CARTESIAN_POINT('Ctrl Pts',(4.49776638929034,24.8451447724241,-11.7470881671935));
#46072=CARTESIAN_POINT('Ctrl Pts',(4.63625734266588,24.8608835998161,-11.7130732733762));
#46073=CARTESIAN_POINT('Ctrl Pts',(4.76938054378893,24.8766740884016,-11.6790902601868));
#46074=CARTESIAN_POINT('Ctrl Pts',(4.90003539201982,24.8921717918239,-11.6457373555599));
#46075=CARTESIAN_POINT('Ctrl Pts',(5.02551969887325,24.9077192645111,-11.6124152200153));
#46076=CARTESIAN_POINT('Ctrl Pts',(5.14589751197744,24.923181544606,-11.5794191457888));
#46077=CARTESIAN_POINT('Ctrl Pts',(5.26549537339328,24.9385436415263,-11.5466368596611));
#46078=CARTESIAN_POINT('Ctrl Pts',(5.38005269865761,24.9538216475631,-11.5141765080823));
#46079=CARTESIAN_POINT('Ctrl Pts',(5.4896322985156,24.9689021151162,-11.4822801409863));
#46080=CARTESIAN_POINT('Ctrl Pts',(5.59870632316951,24.9839130048422,-11.4505309364309));
#46081=CARTESIAN_POINT('Ctrl Pts',(5.70284844862924,24.9987281898052,-11.4193405622832));
#46082=CARTESIAN_POINT('Ctrl Pts',(5.8021206202617,25.0132544553156,-11.3888995459745));
#46083=CARTESIAN_POINT('Ctrl Pts',(5.86628458488748,25.0226434187182,-11.3692241801446));
#46084=CARTESIAN_POINT('Ctrl Pts',(5.92841407534379,25.0319120614579,-11.3498608839104));
#46085=CARTESIAN_POINT('Ctrl Pts',(5.98852581792881,25.0410393365977,-11.3308502649318));
#46086=CARTESIAN_POINT('Ctrl Pts',(-6.39567215432545,24.265774903146,-11.8440001019888));
#46087=CARTESIAN_POINT('Ctrl Pts',(-6.35564925509037,24.2594187557205,-11.8565901638456));
#46088=CARTESIAN_POINT('Ctrl Pts',(-5.98524856741148,24.2012636643636,-11.9719912725476));
#46089=CARTESIAN_POINT('Ctrl Pts',(-5.25616414804593,24.0987563586202,-12.1789682214255));
#46090=CARTESIAN_POINT('Ctrl Pts',(-4.17575802164877,23.9769542776332,-12.4300252137512));
#46091=CARTESIAN_POINT('Ctrl Pts',(-3.01936659820269,23.8792986630108,-12.635041294384));
#46092=CARTESIAN_POINT('Ctrl Pts',(-1.83578627600257,23.8136687543955,-12.7756187500438));
#46093=CARTESIAN_POINT('Ctrl Pts',(-0.697926096906866,23.7825583234657,
-12.8441380550359));
#46094=CARTESIAN_POINT('Ctrl Pts',(0.331404301616038,23.779455773439,-12.8512035366654));
#46095=CARTESIAN_POINT('Ctrl Pts',(1.24580220726389,23.7959565232568,-12.8144576038436));
#46096=CARTESIAN_POINT('Ctrl Pts',(2.07029186514626,23.8272315262671,-12.7465820496497));
#46097=CARTESIAN_POINT('Ctrl Pts',(2.81705936611203,23.869392282327,-12.6564409209412));
#46098=CARTESIAN_POINT('Ctrl Pts',(3.49017608620424,23.9189803910815,-12.5517050127182));
#46099=CARTESIAN_POINT('Ctrl Pts',(4.09496422292832,23.972993995276,-12.4387800495708));
#46100=CARTESIAN_POINT('Ctrl Pts',(4.65004649527303,24.0305536768163,-12.3195545718887));
#46101=CARTESIAN_POINT('Ctrl Pts',(5.18049690603252,24.0928845644996,-12.1916416689504));
#46102=CARTESIAN_POINT('Ctrl Pts',(5.70541816523766,24.1618784673525,-12.051497359207));
#46103=CARTESIAN_POINT('Ctrl Pts',(6.1097803153111,24.2209469472287,-11.9329737822134));
#46104=CARTESIAN_POINT('Ctrl Pts',(6.34031508757241,24.2569835443928,-11.8614131544149));
#46105=CARTESIAN_POINT('Ctrl Pts',(6.39541677055505,24.2657356792402,-11.8440802204204));
#46106=CARTESIAN_POINT('Ctrl Pts',(-6.33011139869697,24.6389171751212,-11.8152694738916));
#46107=CARTESIAN_POINT('Ctrl Pts',(-6.2905632136143,24.6326417224546,-11.827825040408));
#46108=CARTESIAN_POINT('Ctrl Pts',(-5.92452857340538,24.5752212779463,-11.9429199004965));
#46109=CARTESIAN_POINT('Ctrl Pts',(-5.20357284607826,24.4739472076042,-12.149509367077));
#46110=CARTESIAN_POINT('Ctrl Pts',(-4.13461175671286,24.3535549525084,-12.4002991475077));
#46111=CARTESIAN_POINT('Ctrl Pts',(-2.99009397874043,24.2570037555148,-12.6052161854276));
#46112=CARTESIAN_POINT('Ctrl Pts',(-1.81832922056056,24.1921007647318,-12.7457865099649));
#46113=CARTESIAN_POINT('Ctrl Pts',(-0.691521468902351,24.1613240343279,
-12.814324153161));
#46114=CARTESIAN_POINT('Ctrl Pts',(0.328402059320489,24.1582532792487,-12.821393159439));
#46115=CARTESIAN_POINT('Ctrl Pts',(1.23408499152528,24.1745795912403,-12.7846344259474));
#46116=CARTESIAN_POINT('Ctrl Pts',(2.0504931373738,24.2055131843259,-12.7167509212318));
#46117=CARTESIAN_POINT('Ctrl Pts',(2.78979399227695,24.2472061242734,-12.6266188073296));
#46118=CARTESIAN_POINT('Ctrl Pts',(3.45606870618063,24.2962368704784,-12.5219191994195));
#46119=CARTESIAN_POINT('Ctrl Pts',(4.05461471151914,24.3496364162726,-12.4090636434254));
#46120=CARTESIAN_POINT('Ctrl Pts',(4.60387478749737,24.4065338746757,-12.2899461861913));
#46121=CARTESIAN_POINT('Ctrl Pts',(5.12865373502468,24.4681372375982,-12.1621914677793));
#46122=CARTESIAN_POINT('Ctrl Pts',(5.64781964673563,24.5363100389222,-12.022276439811));
#46123=CARTESIAN_POINT('Ctrl Pts',(6.04758703724719,24.5946551774785,-11.9040078838942));
#46124=CARTESIAN_POINT('Ctrl Pts',(6.27541106315239,24.6302374636023,-11.832634783351));
#46125=CARTESIAN_POINT('Ctrl Pts',(6.3298587211672,24.6388783655307,-11.8153494295136));
#46126=CARTESIAN_POINT('Ctrl Pts',(-6.21909462167523,24.9345658565175,-11.6041618753865));
#46127=CARTESIAN_POINT('Ctrl Pts',(-6.18025122001806,24.9284618793619,-11.616587032151));
#46128=CARTESIAN_POINT('Ctrl Pts',(-5.82072605398916,24.8726105239354,-11.7304922022284));
#46129=CARTESIAN_POINT('Ctrl Pts',(-5.11236921312775,24.7741073881107,-11.9350365015387));
#46130=CARTESIAN_POINT('Ctrl Pts',(-4.06204085349769,24.6570764218307,-12.1834178932697));
#46131=CARTESIAN_POINT('Ctrl Pts',(-2.9376206588192,24.563286303404,-12.386392728577));
#46132=CARTESIAN_POINT('Ctrl Pts',(-1.78654233000432,24.5002752909014,-12.5256393828724));
#46133=CARTESIAN_POINT('Ctrl Pts',(-0.679604906695004,24.4704003046752,
-12.5935378394357));
#46134=CARTESIAN_POINT('Ctrl Pts',(0.322775234820087,24.4674185850898,-12.6005420435692));
#46135=CARTESIAN_POINT('Ctrl Pts',(1.21259995881462,24.48326794551,-12.5641242474114));
#46136=CARTESIAN_POINT('Ctrl Pts',(2.01460907294657,24.5132960752993,-12.4968773610704));
#46137=CARTESIAN_POINT('Ctrl Pts',(2.74086259778098,24.5537768690484,-12.4075943492003));
#46138=CARTESIAN_POINT('Ctrl Pts',(3.39541033297856,24.6013967849816,-12.3038851096544));
#46139=CARTESIAN_POINT('Ctrl Pts',(3.98346188181152,24.6532777843204,-12.1921022704338));
#46140=CARTESIAN_POINT('Ctrl Pts',(4.52312475590325,24.7085761466578,-12.0741247427906));
#46141=CARTESIAN_POINT('Ctrl Pts',(5.03875163209351,24.7684672518194,-11.9476048546621));
#46142=CARTESIAN_POINT('Ctrl Pts',(5.54885320696534,24.8347635054044,-11.8090629842029));
#46143=CARTESIAN_POINT('Ctrl Pts',(5.94159338064799,24.8915133781883,-11.6919835098928));
#46144=CARTESIAN_POINT('Ctrl Pts',(6.16536922582763,24.9261233518869,-11.6213467860975));
#46145=CARTESIAN_POINT('Ctrl Pts',(6.2188461543419,24.9345280272955,-11.6042410555399));
#46146=CARTESIAN_POINT('Ctrl Pts',(-6.0944235252482,25.0682520215298,-11.2712582249933));
#46147=CARTESIAN_POINT('Ctrl Pts',(-6.05631315053343,25.0623611570049,-11.2834944621479));
#46148=CARTESIAN_POINT('Ctrl Pts',(-5.703576774987,25.0084636391483,-11.3956677411211));
#46149=CARTESIAN_POINT('Ctrl Pts',(-5.00868072692008,24.9134749280578,-11.5970959616219));
#46150=CARTESIAN_POINT('Ctrl Pts',(-3.97883577950606,24.8007932001164,-11.8416189837205));
#46151=CARTESIAN_POINT('Ctrl Pts',(-2.87697998756759,24.7106292980149,-12.0413659895638));
#46152=CARTESIAN_POINT('Ctrl Pts',(-1.74953270102815,24.6501329141197,-12.1783524777748));
#46153=CARTESIAN_POINT('Ctrl Pts',(-0.665590719009689,24.6214691809497,
-12.2451377662104));
#46154=CARTESIAN_POINT('Ctrl Pts',(0.316136038753768,24.6186082091784,-12.252027451311));
#46155=CARTESIAN_POINT('Ctrl Pts',(1.18750276604363,24.6338148510926,-12.2162064264699));
#46156=CARTESIAN_POINT('Ctrl Pts',(1.9729205261056,24.662633058189,-12.1500579331026));
#46157=CARTESIAN_POINT('Ctrl Pts',(2.68428382255306,24.7015048827846,-12.0622203269822));
#46158=CARTESIAN_POINT('Ctrl Pts',(3.32557899278067,24.7472649536685,-11.9601712105928));
#46159=CARTESIAN_POINT('Ctrl Pts',(3.90188993653852,24.7971582354132,-11.8501564777456));
#46160=CARTESIAN_POINT('Ctrl Pts',(4.43092963053168,24.8503790191096,-11.7340236139045));
#46161=CARTESIAN_POINT('Ctrl Pts',(4.93654521767705,24.9080639417193,-11.6094608352251));
#46162=CARTESIAN_POINT('Ctrl Pts',(5.43686957263232,24.9719660756905,-11.473041994514));
#46163=CARTESIAN_POINT('Ctrl Pts',(5.82216258062342,25.0267059804824,-11.3577445394207));
#46164=CARTESIAN_POINT('Ctrl Pts',(6.04171208841225,25.0601043017063,-11.2881818237279));
#46165=CARTESIAN_POINT('Ctrl Pts',(6.09417956626521,25.0682154577126,-11.2713362394887));
#46166=CARTESIAN_POINT('',(6.27159454871108,24.2690137147111,-11.8794923468356));
#46167=CARTESIAN_POINT('Origin',(5.999999949017,24.12594200518,-10.9277802669376));
#46168=CARTESIAN_POINT('Ctrl Pts',(-6.27159387328068,24.2690123753745,-11.8794984953319));
#46169=CARTESIAN_POINT('Ctrl Pts',(-6.13239664937028,24.2474082730374,-11.9224692187189));
#46170=CARTESIAN_POINT('Ctrl Pts',(-5.98564492666201,24.2255025436533,-11.9663158733557));
#46171=CARTESIAN_POINT('Ctrl Pts',(-5.83132864861891,24.2035349808948,-12.0105538996301));
#46172=CARTESIAN_POINT('Ctrl Pts',(-5.679074110429,24.1818609153628,-12.0542008845514));
#46173=CARTESIAN_POINT('Ctrl Pts',(-5.51945550383331,24.1601268866317,-12.0982288854611));
#46174=CARTESIAN_POINT('Ctrl Pts',(-5.35247247395099,24.1385689974971,-12.1421228435869));
#46175=CARTESIAN_POINT('Ctrl Pts',(-5.32566610845767,24.1351082347129,-12.1491692930692));
#46176=CARTESIAN_POINT('Ctrl Pts',(-5.29866997954998,24.1316520193249,-12.1562121822653));
#46177=CARTESIAN_POINT('Ctrl Pts',(-5.27148411637172,24.1282013361865,-12.1632492579947));
#46178=CARTESIAN_POINT('Ctrl Pts',(-5.14595239291341,24.1122676798361,-12.1957432140862));
#46179=CARTESIAN_POINT('Ctrl Pts',(-5.01637482818976,24.096451644679,-12.2281144526996));
#46180=CARTESIAN_POINT('Ctrl Pts',(-4.88275739366669,24.080862396749,-12.2601325356358));
#46181=CARTESIAN_POINT('Ctrl Pts',(-4.7110640926815,24.0608308084571,-12.3012745495516));
#46182=CARTESIAN_POINT('Ctrl Pts',(-4.53269553658461,24.0411729421543,-12.341836233405));
#46183=CARTESIAN_POINT('Ctrl Pts',(-4.34764553875065,24.0221340594359,-12.3812950680686));
#46184=CARTESIAN_POINT('Ctrl Pts',(-4.29583923524703,24.0168039640669,-12.3923419007539));
#46185=CARTESIAN_POINT('Ctrl Pts',(-4.243509363582,24.0115224543185,-12.4033020094073));
#46186=CARTESIAN_POINT('Ctrl Pts',(-4.19065603668429,24.0062950769768,-12.4141632529344));
#46187=CARTESIAN_POINT('Ctrl Pts',(-4.14338231788257,24.0016195422276,-12.423877899154));
#46188=CARTESIAN_POINT('Ctrl Pts',(-4.09568982943223,23.9969873138978,-12.4335134474914));
#46189=CARTESIAN_POINT('Ctrl Pts',(-4.04757899984503,23.9924025362211,-12.4430611407423));
#46190=CARTESIAN_POINT('Ctrl Pts',(-3.90056248222818,23.9783924255274,-12.472236871551));
#46191=CARTESIAN_POINT('Ctrl Pts',(-3.74963598148268,23.964824956328,-12.5005941095896));
#46192=CARTESIAN_POINT('Ctrl Pts',(-3.59479967323274,23.9518214674941,-12.5278747701407));
#46193=CARTESIAN_POINT('Ctrl Pts',(-3.51738151910778,23.9453197230771,-12.5415151004163));
#46194=CARTESIAN_POINT('Ctrl Pts',(-3.43898590449499,23.9389590693787,-12.5548860361321));
#46195=CARTESIAN_POINT('Ctrl Pts',(-3.35961280203394,23.9327552491476,-12.5679537419326));
#46196=CARTESIAN_POINT('Ctrl Pts',(-3.31992625080342,23.929653339032,-12.5744875948328));
#46197=CARTESIAN_POINT('Ctrl Pts',(-3.27999532521964,23.9265906354718,-12.5809456244407));
#46198=CARTESIAN_POINT('Ctrl Pts',(-3.23982002131168,23.9235691510685,-12.5873234953188));
#46199=CARTESIAN_POINT('Ctrl Pts',(-3.2197323693577,23.9220584088669,-12.5905124307578));
#46200=CARTESIAN_POINT('Ctrl Pts',(-3.19958362267288,23.920557971337,-12.5936813254797));
#46201=CARTESIAN_POINT('Ctrl Pts',(-3.17937378026934,23.9190680909098,-12.5968296310125));
#46202=CARTESIAN_POINT('Ctrl Pts',(-3.16169016816624,23.9177644455359,-12.5995843983537));
#46203=CARTESIAN_POINT('Ctrl Pts',(-3.14395977964478,23.9164688829369,-12.6023234020356));
#46204=CARTESIAN_POINT('Ctrl Pts',(-3.12618261394994,23.9151815729868,-12.6050462717683));
#46205=CARTESIAN_POINT('Ctrl Pts',(-3.12364301885068,23.9149976715654,-12.6054352531587));
#46206=CARTESIAN_POINT('Ctrl Pts',(-3.11986204396182,23.9147243469594,-12.606013432432));
#46207=CARTESIAN_POINT('Ctrl Pts',(-3.11856096474608,23.9146303745096,-12.6062122270458));
#46208=CARTESIAN_POINT('Ctrl Pts',(-3.09161192130301,23.9126839383508,-12.6103298277411));
#46209=CARTESIAN_POINT('Ctrl Pts',(-3.06343761612503,23.9106765413445,-12.6145811111119));
#46210=CARTESIAN_POINT('Ctrl Pts',(-3.03403807604731,23.9086154043005,-12.6189508233468));
#46211=CARTESIAN_POINT('Ctrl Pts',(-2.96197172541788,23.9035629910819,-12.6296621886687));
#46212=CARTESIAN_POINT('Ctrl Pts',(-2.88254328538339,23.898186158627,-12.6410884371183));
#46213=CARTESIAN_POINT('Ctrl Pts',(-2.79575239027412,23.8926064649136,-12.6529724277651));
#46214=CARTESIAN_POINT('Ctrl Pts',(-2.7092917509017,23.8870480029879,-12.6648111975845));
#46215=CARTESIAN_POINT('Ctrl Pts',(-2.61552433421982,23.8812882565591,-12.6771042612895));
#46216=CARTESIAN_POINT('Ctrl Pts',(-2.51445087260997,23.8754687341903,-12.6895502780204));
#46217=CARTESIAN_POINT('Ctrl Pts',(-2.50259165346356,23.874785914091,-12.6910106023979));
#46218=CARTESIAN_POINT('Ctrl Pts',(-2.49063185611826,23.8741022949286,-12.6924729786301));
#46219=CARTESIAN_POINT('Ctrl Pts',(-2.4785714853039,23.8734181242808,-12.693936876879));
#46220=CARTESIAN_POINT('Ctrl Pts',(-2.37688564609167,23.8676496062509,-12.7062795920612));
#46221=CARTESIAN_POINT('Ctrl Pts',(-2.2680498179562,23.8618405756023,-12.7187343126261));
#46222=CARTESIAN_POINT('Ctrl Pts',(-2.15206279422411,23.8561524998458,-12.7309579520322));
#46223=CARTESIAN_POINT('Ctrl Pts',(-2.11969736791119,23.8545652792169,-12.7343688792872));
#46224=CARTESIAN_POINT('Ctrl Pts',(-2.08677515745332,23.8529875972799,-12.7377615303618));
#46225=CARTESIAN_POINT('Ctrl Pts',(-2.05329625680072,23.8514232415302,-12.7411277890785));
#46226=CARTESIAN_POINT('Ctrl Pts',(-1.97656813203254,23.8478379958737,-12.7488426994781));
#46227=CARTESIAN_POINT('Ctrl Pts',(-1.89691553063701,23.8443225615171,-12.7564195711127));
#46228=CARTESIAN_POINT('Ctrl Pts',(-1.81433840739538,23.8409252166606,-12.7637550190458));
#46229=CARTESIAN_POINT('Ctrl Pts',(-1.81240132437288,23.840845522203,-12.7639270929943));
#46230=CARTESIAN_POINT('Ctrl Pts',(-1.81046263209235,23.8407658927029,-12.7640990337383));
#46231=CARTESIAN_POINT('Ctrl Pts',(-1.80852233053468,23.8406863288454,-12.7642708398867));
#46232=CARTESIAN_POINT('Ctrl Pts',(-1.76910546799746,23.8390700039906,-12.7677610495955));
#46233=CARTESIAN_POINT('Ctrl Pts',(-1.7290244576289,23.8374807582071,-12.7711957460505));
#46234=CARTESIAN_POINT('Ctrl Pts',(-1.68827932271826,23.8359241927331,-12.7745632603602));
#46235=CARTESIAN_POINT('Ctrl Pts',(-1.66690391227081,23.8351075989,-12.7763299007387));
#46236=CARTESIAN_POINT('Ctrl Pts',(-1.64534572150314,23.8342999983825,-12.7780780453442));
#46237=CARTESIAN_POINT('Ctrl Pts',(-1.6236047512744,23.8335022086739,-12.7798059672955));
#46238=CARTESIAN_POINT('Ctrl Pts',(-1.61273426616003,23.8331033138196,-12.7806699282712));
#46239=CARTESIAN_POINT('Ctrl Pts',(-1.60181808614543,23.8327068716212,-12.7815288331432));
#46240=CARTESIAN_POINT('Ctrl Pts',(-1.59085621133314,23.8323129856253,-12.7823824632121));
#46241=CARTESIAN_POINT('Ctrl Pts',(-1.585375273927,23.8321160426274,-12.7828092782465));
#46242=CARTESIAN_POINT('Ctrl Pts',(-1.57988291281928,23.8319197386772,-12.7832347745525));
#46243=CARTESIAN_POINT('Ctrl Pts',(-1.57437912802292,23.8317240868079,-12.7836589246136));
#46244=CARTESIAN_POINT('Ctrl Pts',(-1.56887534322656,23.8315284349386,-12.7840830746747));
#46245=CARTESIAN_POINT('Ctrl Pts',(-1.56205961728679,23.8312877046499,-12.7846050486512));
#46246=CARTESIAN_POINT('Ctrl Pts',(-1.55783350257619,23.8311391004969,-12.7849273084309));
#46247=CARTESIAN_POINT('Ctrl Pts',(-1.33210044392375,23.8232015805096,-12.8021404440734));
#46248=CARTESIAN_POINT('Ctrl Pts',(-1.11005401698134,23.8171220430774,-12.8153351438866));
#46249=CARTESIAN_POINT('Ctrl Pts',(-0.89169728020786,23.8127291140289,-12.8248709020606));
#46250=CARTESIAN_POINT('Ctrl Pts',(-0.848420918716724,23.8118584745958,
-12.8267608044466));
#46251=CARTESIAN_POINT('Ctrl Pts',(-0.805289381652995,23.8110541639786,
-12.8285068870435));
#46252=CARTESIAN_POINT('Ctrl Pts',(-0.762302540745554,23.8103149636894,
-12.8301118046048));
#46253=CARTESIAN_POINT('Ctrl Pts',(-0.724717058268129,23.8096686449804,
-12.8315150619647));
#46254=CARTESIAN_POINT('Ctrl Pts',(-0.687242178941791,23.8090720699838,
-12.8328104033074));
#46255=CARTESIAN_POINT('Ctrl Pts',(-0.649878100570094,23.8085243069343,
-12.8339995799136));
#46256=CARTESIAN_POINT('Ctrl Pts',(-0.558066241026871,23.8071783311641,
-12.836921651601));
#46257=CARTESIAN_POINT('Ctrl Pts',(-0.466923437756322,23.806127042761,-12.8392027737831));
#46258=CARTESIAN_POINT('Ctrl Pts',(-0.376448925310672,23.8053581696707,
-12.8408704275147));
#46259=CARTESIAN_POINT('Ctrl Pts',(-0.31280175564922,23.8048172814723,-12.8420435915045));
#46260=CARTESIAN_POINT('Ctrl Pts',(-0.24948547424537,23.8044160901311,-12.8429131420936));
#46261=CARTESIAN_POINT('Ctrl Pts',(-0.186500081418701,23.8041502793706,
-12.8434883990749));
#46262=CARTESIAN_POINT('Ctrl Pts',(-0.155007385005365,23.8040173739904,
-12.8437760275656));
#46263=CARTESIAN_POINT('Ctrl Pts',(-0.123597410613271,23.8039183134464,
-12.8439900796137));
#46264=CARTESIAN_POINT('Ctrl Pts',(-0.0922701578635517,23.8038525592422,
-12.8441317020657));
#46265=CARTESIAN_POINT('Ctrl Pts',(-0.0647193108532514,23.8037947315087,
-12.8442562523587));
#46266=CARTESIAN_POINT('Ctrl Pts',(-0.0383382413166024,23.8037631765259,
-12.8443236937014));
#46267=CARTESIAN_POINT('Ctrl Pts',(-0.01020945845667,23.8037560879699,-12.8443378683129));
#46268=CARTESIAN_POINT('Ctrl Pts',(-0.00635383481666235,23.8037551163386,
-12.8443398112326));
#46269=CARTESIAN_POINT('Ctrl Pts',(-0.0024653745155048,23.8037546371122,
-12.8443406807256));
#46270=CARTESIAN_POINT('Ctrl Pts',(0.00146343591164922,23.8037546775758,
-12.8443404157537));
#46271=CARTESIAN_POINT('Ctrl Pts',(0.123996040178889,23.803755939565,-12.844332151754));
#46272=CARTESIAN_POINT('Ctrl Pts',(0.246525247851222,23.8042791850219,-12.8432200505871));
#46273=CARTESIAN_POINT('Ctrl Pts',(0.369056161642459,23.8053127715422,-12.8410041049826));
#46274=CARTESIAN_POINT('Ctrl Pts',(0.644870892073421,23.8076393549214,-12.8360160540438));
#46275=CARTESIAN_POINT('Ctrl Pts',(0.920694080264234,23.8125502518664,-12.8254380362402));
#46276=CARTESIAN_POINT('Ctrl Pts',(1.19651513906033,23.8200735682843,-12.8092727889426));
#46277=CARTESIAN_POINT('Ctrl Pts',(1.22211216178672,23.8207717546452,-12.8077726054386));
#46278=CARTESIAN_POINT('Ctrl Pts',(1.2477091679562,23.8214924566863,-12.8062242693096));
#46279=CARTESIAN_POINT('Ctrl Pts',(1.27330614987264,23.8222357071553,-12.8046277624084));
#46280=CARTESIAN_POINT('Ctrl Pts',(1.37082342232289,23.8250672815464,-12.7985455219725));
#46281=CARTESIAN_POINT('Ctrl Pts',(1.4683403440741,23.8282260948037,-12.7917641881055));
#46282=CARTESIAN_POINT('Ctrl Pts',(1.56585686826745,23.8317101405147,-12.7842847836682));
#46283=CARTESIAN_POINT('Ctrl Pts',(1.74017752235782,23.8379382247521,-12.7709145914417));
#46284=CARTESIAN_POINT('Ctrl Pts',(1.91449856143439,23.8452069077848,-12.7553138369756));
#46285=CARTESIAN_POINT('Ctrl Pts',(2.0888191476779,23.8535159164419,-12.7374817690434));
#46286=CARTESIAN_POINT('Ctrl Pts',(2.17523066093796,23.8576347301014,-12.7286423312708));
#46287=CARTESIAN_POINT('Ctrl Pts',(2.26164204571388,23.8620092342545,-12.7192544966263));
#46288=CARTESIAN_POINT('Ctrl Pts',(2.34805359307956,23.8666392625227,-12.7093187482457));
#46289=CARTESIAN_POINT('Ctrl Pts',(2.47841969428531,23.8736244254112,-12.6943290296443));
#46290=CARTESIAN_POINT('Ctrl Pts',(2.60878583461951,23.8811913884393,-12.6780923254294));
#46291=CARTESIAN_POINT('Ctrl Pts',(2.73915198676214,23.889339995395,-12.6606086882267));
#46292=CARTESIAN_POINT('Ctrl Pts',(2.77254322428871,23.8914271327838,-12.6561305298008));
#46293=CARTESIAN_POINT('Ctrl Pts',(2.8059344685154,23.8935524189645,-12.6515705566779));
#46294=CARTESIAN_POINT('Ctrl Pts',(2.83932570101241,23.8957158662664,-12.6469287491679));
#46295=CARTESIAN_POINT('Ctrl Pts',(2.87111753476851,23.8977756871181,-12.642509278497));
#46296=CARTESIAN_POINT('Ctrl Pts',(2.90290935786543,23.8998701009498,-12.6380156251359));
#46297=CARTESIAN_POINT('Ctrl Pts',(2.93470118631675,23.901999091517,-12.6334478145499));
#46298=CARTESIAN_POINT('Ctrl Pts',(2.98358847784925,23.9052729070727,-12.6264237489751));
#46299=CARTESIAN_POINT('Ctrl Pts',(3.03247576591333,23.9086285032369,-12.6192243315775));
#46300=CARTESIAN_POINT('Ctrl Pts',(3.08136305640405,23.912065877191,-12.6118496258009));
#46301=CARTESIAN_POINT('Ctrl Pts',(3.09765881990095,23.913211668509,-12.6093913905421));
#46302=CARTESIAN_POINT('Ctrl Pts',(3.1120376099665,23.9142296217841,-12.6072074384278));
#46303=CARTESIAN_POINT('Ctrl Pts',(3.13025034772233,23.9155305100753,-12.6044164911794));
#46304=CARTESIAN_POINT('Ctrl Pts',(3.2587697411143,23.924710314688,-12.5847219865885));
#46305=CARTESIAN_POINT('Ctrl Pts',(3.38586955228427,23.9344222653021,-12.5640260906196));
#46306=CARTESIAN_POINT('Ctrl Pts',(3.51153601864268,23.9446273099282,-12.5424100887366));
#46307=CARTESIAN_POINT('Ctrl Pts',(3.71379593266574,23.9610523078492,-12.5076191790446));
#46308=CARTESIAN_POINT('Ctrl Pts',(3.91234201511289,23.9787543899613,-12.4704458493914));
#46309=CARTESIAN_POINT('Ctrl Pts',(4.10714050344062,23.9975745994538,-12.431221102725));
#46310=CARTESIAN_POINT('Ctrl Pts',(4.29249186451379,24.015482086699,-12.3938986355705));
#46311=CARTESIAN_POINT('Ctrl Pts',(4.47445059197192,24.0344019634126,-12.3547187661609));
#46312=CARTESIAN_POINT('Ctrl Pts',(4.65300686531934,24.0542044882689,-12.3139537130224));
#46313=CARTESIAN_POINT('Ctrl Pts',(4.83064737904963,24.0739054521314,-12.2733977311686));
#46314=CARTESIAN_POINT('Ctrl Pts',(5.00492039832214,24.0944801390872,-12.2312727514534));
#46315=CARTESIAN_POINT('Ctrl Pts',(5.17583188150985,24.1158107736013,-12.1878325206193));
#46316=CARTESIAN_POINT('Ctrl Pts',(5.35320454393151,24.137947796605,-12.1427500647448));
#46317=CARTESIAN_POINT('Ctrl Pts',(5.52695678608636,24.1608991837852,-12.096251090736));
#46318=CARTESIAN_POINT('Ctrl Pts',(5.6971101511077,24.1845478230226,-12.0486012589137));
#46319=CARTESIAN_POINT('Ctrl Pts',(5.87744252616867,24.2096111844207,-11.9981008921257));
#46320=CARTESIAN_POINT('Ctrl Pts',(6.05373257798032,24.2354580859825,-11.9463079576679));
#46321=CARTESIAN_POINT('Ctrl Pts',(6.22601914496659,24.2619708293824,-11.8935153712287));
#46322=CARTESIAN_POINT('Ctrl Pts',(6.24124268414525,24.2643135412661,-11.8888505269401));
#46323=CARTESIAN_POINT('Ctrl Pts',(6.25643497109608,24.2666614495617,-11.884177863846));
#46324=CARTESIAN_POINT('Ctrl Pts',(6.27159604014383,24.2690144967095,-11.8794975712513));
#46325=CARTESIAN_POINT('Origin',(5.999999999061,24.1259421376201,-10.9277802195584));
#46326=CARTESIAN_POINT('Origin',(5.99996968668368,24.1259230380857,-10.9277552850324));
#46327=CARTESIAN_POINT('Ctrl Pts',(6.25613331744712,13.9489619820917,-8.4284867777746));
#46328=CARTESIAN_POINT('Ctrl Pts',(6.30398162206973,13.9460624564194,-8.4074766351842));
#46329=CARTESIAN_POINT('Ctrl Pts',(6.44264536447383,13.9427640734649,-8.33682408595486));
#46330=CARTESIAN_POINT('Ctrl Pts',(6.65740687788328,13.9634937286633,-8.17768320800854));
#46331=CARTESIAN_POINT('Ctrl Pts',(6.87093031596624,14.0289047773005,-7.9319975038466));
#46332=CARTESIAN_POINT('Ctrl Pts',(7.02371352601407,14.1310161098413,-7.64667378240476));
#46333=CARTESIAN_POINT('Ctrl Pts',(7.09387171678717,14.2445990542294,-7.38242484159179));
#46334=CARTESIAN_POINT('Ctrl Pts',(7.10431447968315,14.32188980161,-7.22230334652378));
#46335=CARTESIAN_POINT('Ctrl Pts',(7.10368173933534,14.3516768211256,-7.16309324424638));
#46336=CARTESIAN_POINT('Ctrl Pts',(6.05827718003039,13.4862137568793,-8.02727938977323));
#46337=CARTESIAN_POINT('Ctrl Pts',(6.10075122454661,13.4833941800054,-8.00882735698102));
#46338=CARTESIAN_POINT('Ctrl Pts',(6.22408246292093,13.479581942238,-7.94671825031444));
#46339=CARTESIAN_POINT('Ctrl Pts',(6.41612732474395,13.4959994652657,-7.80631939831103));
#46340=CARTESIAN_POINT('Ctrl Pts',(6.6081082855051,13.5516701956529,-7.5886512718711));
#46341=CARTESIAN_POINT('Ctrl Pts',(6.74599089454977,13.6405012639782,-7.3352289873818));
#46342=CARTESIAN_POINT('Ctrl Pts',(6.80936980898649,13.7404476399642,-7.10053992025847));
#46343=CARTESIAN_POINT('Ctrl Pts',(6.81876823331771,13.8087304568116,-6.95878686654306));
#46344=CARTESIAN_POINT('Ctrl Pts',(6.81819968063314,13.8350481205052,-6.90649028682641));
#46345=CARTESIAN_POINT('Ctrl Pts',(6.04955572358106,12.8455322123978,-8.08627330790688));
#46346=CARTESIAN_POINT('Ctrl Pts',(6.1079900662572,12.8418918206761,-8.06126216610187));
#46347=CARTESIAN_POINT('Ctrl Pts',(6.27656937354435,12.8375323202349,-7.97762604596949));
#46348=CARTESIAN_POINT('Ctrl Pts',(6.53441767608495,12.861417377942,-7.79202339799651));
#46349=CARTESIAN_POINT('Ctrl Pts',(6.78749235738749,12.9366218552611,-7.50985856325181));
#46350=CARTESIAN_POINT('Ctrl Pts',(6.96695694214048,13.0529645859862,-7.18551418269103));
#46351=CARTESIAN_POINT('Ctrl Pts',(7.04916843852754,13.1817527221056,-6.8862940990644));
#46352=CARTESIAN_POINT('Ctrl Pts',(7.06151642465278,13.2696410515648,-6.70425305611641));
#46353=CARTESIAN_POINT('Ctrl Pts',(7.06076537745517,13.30363561243,-6.63667727119217));
#46354=CARTESIAN_POINT('Ctrl Pts',(6.23560916772017,12.4584536559934,-8.56519010373521));
#46355=CARTESIAN_POINT('Ctrl Pts',(6.32056751352294,12.4536453748849,-8.52892949502008));
#46356=CARTESIAN_POINT('Ctrl Pts',(6.56443955501225,12.4490736721987,-8.40822505546004));
#46357=CARTESIAN_POINT('Ctrl Pts',(6.93220306534565,12.4871642464157,-8.14398300609675));
#46358=CARTESIAN_POINT('Ctrl Pts',(7.28777720473864,12.5979902636432,-7.74834066871077));
#46359=CARTESIAN_POINT('Ctrl Pts',(7.5372435266576,12.7640653483726,-7.29812244537945));
#46360=CARTESIAN_POINT('Ctrl Pts',(7.65118970568607,12.944704829802,-6.88383897116639));
#46361=CARTESIAN_POINT('Ctrl Pts',(7.66849057114655,13.0675783364571,-6.63004784546159));
#46362=CARTESIAN_POINT('Ctrl Pts',(7.66743350755391,13.1152141901136,-6.53531350553332));
#46363=CARTESIAN_POINT('',(7.,13.9487330738339,-6.97709941346537));
#46364=CARTESIAN_POINT('',(7.00000024171084,12.5220639668164,-8.04447769320174));
#46365=CARTESIAN_POINT('Ctrl Pts',(7.,13.9487330738339,-6.97709941346537));
#46366=CARTESIAN_POINT('Ctrl Pts',(7.,13.8474233649361,-7.02089621734514));
#46367=CARTESIAN_POINT('Ctrl Pts',(7.,13.7572507680496,-7.06228070002983));
#46368=CARTESIAN_POINT('Ctrl Pts',(7.,13.6796219035787,-7.10036238057953));
#46369=CARTESIAN_POINT('Ctrl Pts',(7.,13.6408074713433,-7.11940322085437));
#46370=CARTESIAN_POINT('Ctrl Pts',(7.,13.6051028921232,-7.13758106048456));
#46371=CARTESIAN_POINT('Ctrl Pts',(7.,13.5725576246799,-7.15462107918448));
#46372=CARTESIAN_POINT('Ctrl Pts',(7.,13.5562849909583,-7.16314108853445));
#46373=CARTESIAN_POINT('Ctrl Pts',(7.,13.5408011417253,-7.17137543826938));
#46374=CARTESIAN_POINT('Ctrl Pts',(7.,13.5261067530512,-7.17928526244922));
#46375=CARTESIAN_POINT('Ctrl Pts',(7.,13.5187595587141,-7.18324017453914));
#46376=CARTESIAN_POINT('Ctrl Pts',(7.,13.5116097295168,-7.18711395524029));
#46377=CARTESIAN_POINT('Ctrl Pts',(7.,13.5046570157243,-7.19090164180328));
#46378=CARTESIAN_POINT('Ctrl Pts',(7.,13.501180658828,-7.19279548508479));
#46379=CARTESIAN_POINT('Ctrl Pts',(7.,13.497753580783,-7.19466780483175));
#46380=CARTESIAN_POINT('Ctrl Pts',(7.,13.4943757443323,-7.19651798759228));
#46381=CARTESIAN_POINT('Ctrl Pts',(7.,13.4909979078817,-7.19836817035281));
#46382=CARTESIAN_POINT('Ctrl Pts',(7.,13.4891097481019,-7.19940326285153));
#46383=CARTESIAN_POINT('Ctrl Pts',(7.,13.4843899179469,-7.20200151208179));
#46384=CARTESIAN_POINT('Ctrl Pts',(7.,13.4088726354676,-7.24357349976597));
#46385=CARTESIAN_POINT('Ctrl Pts',(7.,13.3376342766462,-7.28583253383395));
#46386=CARTESIAN_POINT('Ctrl Pts',(7.,13.2711782420073,-7.32838772409819));
#46387=CARTESIAN_POINT('Ctrl Pts',(7.,13.2047222073684,-7.37094291436244));
#46388=CARTESIAN_POINT('Ctrl Pts',(7.,13.1443064441612,-7.41284332621996));
#46389=CARTESIAN_POINT('Ctrl Pts',(7.,13.086335335477,-7.45600227764588));
#46390=CARTESIAN_POINT('Ctrl Pts',(7.,12.9703931181087,-7.54232018049772));
#46391=CARTESIAN_POINT('Ctrl Pts',(7.,12.8624564072214,-7.63587433767221));
#46392=CARTESIAN_POINT('Ctrl Pts',(7.,12.7671922400942,-7.73522621634518));
#46393=CARTESIAN_POINT('Ctrl Pts',(7.,12.6719280729671,-7.83457809501815));
#46394=CARTESIAN_POINT('Ctrl Pts',(7.,12.5894712830982,-7.93954794161539));
#46395=CARTESIAN_POINT('Ctrl Pts',(7.,12.5220642584494,-8.04447694179117));
#46396=CARTESIAN_POINT('',(6.24994426646177,12.4626501726359,-8.55169607210683));
#46397=CARTESIAN_POINT('Ctrl Pts',(6.24994458182163,12.4626510719251,-8.55169668917956));
#46398=CARTESIAN_POINT('Ctrl Pts',(6.29730962523071,12.4601998637428,-8.53106267340422));
#46399=CARTESIAN_POINT('Ctrl Pts',(6.34378299838276,12.4587800143928,-8.50904133309007));
#46400=CARTESIAN_POINT('Ctrl Pts',(6.38941189043019,12.4583505508832,-8.48566684378005));
#46401=CARTESIAN_POINT('Ctrl Pts',(6.42007369520999,12.4580619590349,-8.4699596022519));
#46402=CARTESIAN_POINT('Ctrl Pts',(6.45035395481478,12.45822117737,-8.45364039584658));
#46403=CARTESIAN_POINT('Ctrl Pts',(6.48026258827735,12.4588227609006,-8.4367093262394));
#46404=CARTESIAN_POINT('Ctrl Pts',(6.49376528155068,12.4590943546497,-8.42906554538992));
#46405=CARTESIAN_POINT('Ctrl Pts',(6.50719217244104,12.4594561861776,-8.42129694892268));
#46406=CARTESIAN_POINT('Ctrl Pts',(6.5205447379029,12.459907641538,-8.41340334926298));
#46407=CARTESIAN_POINT('Ctrl Pts',(6.58762875903047,12.4621757780263,-8.3737454716921));
#46408=CARTESIAN_POINT('Ctrl Pts',(6.65283225450676,12.4666941319735,-8.3309532994621));
#46409=CARTESIAN_POINT('Ctrl Pts',(6.71587879633085,12.4733990844445,-8.28522333652232));
#46410=CARTESIAN_POINT('Ctrl Pts',(6.73454150082755,12.4753838490804,-8.2716865942951));
#46411=CARTESIAN_POINT('Ctrl Pts',(6.75301492419843,12.4775603607654,-8.25789228705324));
#46412=CARTESIAN_POINT('Ctrl Pts',(6.77129115402012,12.4799273256629,-8.24384519251942));
#46413=CARTESIAN_POINT('Ctrl Pts',(6.81296395481405,12.4853243937466,-8.21181551364404));
#46414=CARTESIAN_POINT('Ctrl Pts',(6.85361150889779,12.4917143765242,-8.17846837699809));
#46415=CARTESIAN_POINT('Ctrl Pts',(6.89323596425004,12.4991044430277,-8.14376490312572));
#46416=CARTESIAN_POINT('Ctrl Pts',(6.89902702850173,12.5001844919411,-8.13869303412045));
#46417=CARTESIAN_POINT('Ctrl Pts',(6.90479617496775,12.5012859442648,-8.13359214701145));
#46418=CARTESIAN_POINT('Ctrl Pts',(6.91054334136795,12.5024088652269,-8.12846207329433));
#46419=CARTESIAN_POINT('Ctrl Pts',(6.94097886456702,12.5083555674127,-8.10129451509989));
#46420=CARTESIAN_POINT('Ctrl Pts',(6.97079915829075,12.5149037297071,-8.0733090443511));
#46421=CARTESIAN_POINT('Ctrl Pts',(7.00000072349027,12.5220628111649,-8.04447789421037));
#46422=CARTESIAN_POINT('',(6.26385803707234,13.9442711326918,-8.42072576609336));
#46423=CARTESIAN_POINT('Origin',(6.52771738877616,13.2547577723573,-9.09520568086109));
#46424=CARTESIAN_POINT('Ctrl Pts',(6.26385550478166,13.9442777501869,-8.42071929290311));
#46425=CARTESIAN_POINT('Ctrl Pts',(6.30452443286976,13.9338444255139,-8.39414427067733));
#46426=CARTESIAN_POINT('Ctrl Pts',(6.34473782035942,13.9244595648097,-8.36476023937334));
#46427=CARTESIAN_POINT('Ctrl Pts',(6.38412017358082,13.9161889610762,-8.33259129990798));
#46428=CARTESIAN_POINT('Ctrl Pts',(6.43028376898849,13.9064942431809,-8.29488319501582));
#46429=CARTESIAN_POINT('Ctrl Pts',(6.47530622992681,13.8983305918767,-8.25334743496533));
#46430=CARTESIAN_POINT('Ctrl Pts',(6.51863204392152,13.8917172362002,-8.20816366664338));
#46431=CARTESIAN_POINT('Ctrl Pts',(6.53236556036768,13.8896209194649,-8.19384121154941));
#46432=CARTESIAN_POINT('Ctrl Pts',(6.54592825180032,13.8876804846815,-8.17915231926784));
#46433=CARTESIAN_POINT('Ctrl Pts',(6.55930139429603,13.8858969140951,-8.16410295969278));
#46434=CARTESIAN_POINT('Ctrl Pts',(6.57612915295727,13.883652602753,-8.14516597528418));
#46435=CARTESIAN_POINT('Ctrl Pts',(6.59265686365932,13.8816566547036,-8.12565821603501));
#46436=CARTESIAN_POINT('Ctrl Pts',(6.60884596028903,13.8799115789078,-8.10559172049823));
#46437=CARTESIAN_POINT('Ctrl Pts',(6.63669630747203,13.8769094986876,-8.07107102547566));
#46438=CARTESIAN_POINT('Ctrl Pts',(6.66354508932836,13.874649698669,-8.03489647221724));
#46439=CARTESIAN_POINT('Ctrl Pts',(6.6892266606921,13.8731171640556,-7.99716821313463));
#46440=CARTESIAN_POINT('Ctrl Pts',(6.7095316520745,13.8719054740979,-7.96733857519326));
#46441=CARTESIAN_POINT('Ctrl Pts',(6.72910683801557,13.8711484558773,-7.93653778302505));
#46442=CARTESIAN_POINT('Ctrl Pts',(6.74786474749874,13.8708408971235,-7.90481678065775));
#46443=CARTESIAN_POINT('Ctrl Pts',(6.75724370224032,13.8706871177466,-7.8889562794741));
#46444=CARTESIAN_POINT('Ctrl Pts',(6.7664182828091,13.8706457384359,-7.87286569376261));
#46445=CARTESIAN_POINT('Ctrl Pts',(6.77537696952256,13.8707163362684,-7.85655154099461));
#46446=CARTESIAN_POINT('Ctrl Pts',(6.7798563128793,13.8707516351847,-7.84839446461061));
#46447=CARTESIAN_POINT('Ctrl Pts',(6.78428167880814,13.8708149310595,-7.8401814940248));
#46448=CARTESIAN_POINT('Ctrl Pts',(6.78865159456431,13.8709061873141,-7.83191343984588));
#46449=CARTESIAN_POINT('Ctrl Pts',(6.78982459935173,13.8709306829861,-7.82969406819763));
#46450=CARTESIAN_POINT('Ctrl Pts',(6.79099360851041,13.8709571933607,-7.82747072784429));
#46451=CARTESIAN_POINT('Ctrl Pts',(6.79215859333577,13.8709857178622,-7.82524343428559));
#46452=CARTESIAN_POINT('Ctrl Pts',(6.79316362759247,13.871010325995,-7.82332194459967));
#46453=CARTESIAN_POINT('Ctrl Pts',(6.79416566671888,13.8710364331518,-7.82139751272386));
#46454=CARTESIAN_POINT('Ctrl Pts',(6.79516469713977,13.8710640359232,-7.81947015226407));
#46455=CARTESIAN_POINT('Ctrl Pts',(6.79696105904224,13.8711136686128,-7.8160045551912));
#46456=CARTESIAN_POINT('Ctrl Pts',(6.79910519164567,13.8711796554962,-7.81182991997246));
#46457=CARTESIAN_POINT('Ctrl Pts',(6.80070351406485,13.8712333795176,-7.80869388659622));
#46458=CARTESIAN_POINT('Ctrl Pts',(6.80102444344323,13.8712441668384,-7.80806419809912));
#46459=CARTESIAN_POINT('Ctrl Pts',(6.80132350624074,13.871254386852,-7.80747646908176));
#46460=CARTESIAN_POINT('Ctrl Pts',(6.80159364688567,13.8712637147728,-7.80694495668783));
#46461=CARTESIAN_POINT('Ctrl Pts',(6.81852791122845,13.8718484526873,-7.77362612240944));
#46462=CARTESIAN_POINT('Ctrl Pts',(6.8351307337105,13.8728723168352,-7.73832342759663));
#46463=CARTESIAN_POINT('Ctrl Pts',(6.85111676556959,13.8744191424824,-7.7010006024349));
#46464=CARTESIAN_POINT('Ctrl Pts',(6.86624053184969,13.8758825343843,-7.66569092148123));
#46465=CARTESIAN_POINT('Ctrl Pts',(6.88081240248914,13.8778139223046,-7.62857313319346));
#46466=CARTESIAN_POINT('Ctrl Pts',(6.894553421665,13.8802837333051,-7.58964285657535));
#46467=CARTESIAN_POINT('Ctrl Pts',(6.90444958100783,13.8820624691393,-7.56160561888994));
#46468=CARTESIAN_POINT('Ctrl Pts',(6.91391408924983,13.8841204526936,-7.5326288089318));
#46469=CARTESIAN_POINT('Ctrl Pts',(6.92282868318488,13.886484152877,-7.50272017513952));
#46470=CARTESIAN_POINT('Ctrl Pts',(6.92839424746096,13.8879598594987,-7.48404760014695));
#46471=CARTESIAN_POINT('Ctrl Pts',(6.93374517006024,13.8895547576781,-7.46501194873757));
#46472=CARTESIAN_POINT('Ctrl Pts',(6.93885429742972,13.8912731958799,-7.44561960630978));
#46473=CARTESIAN_POINT('Ctrl Pts',(6.94955798596152,13.8948733463444,-7.4049923957828));
#46474=CARTESIAN_POINT('Ctrl Pts',(6.95920279168186,13.8990160099639,-7.36279719266331));
#46475=CARTESIAN_POINT('Ctrl Pts',(6.96751456368846,13.9037380721181,-7.31911914123901));
#46476=CARTESIAN_POINT('Ctrl Pts',(6.97543732765642,13.9082391320437,-7.27748531252707));
#46477=CARTESIAN_POINT('Ctrl Pts',(6.98214922820788,13.9132665333231,-7.23450421686683));
#46478=CARTESIAN_POINT('Ctrl Pts',(6.98737818945742,13.9188495108828,-7.19028269317926));
#46479=CARTESIAN_POINT('Ctrl Pts',(6.9882530277002,13.9197835782902,-7.18288415296647));
#46480=CARTESIAN_POINT('Ctrl Pts',(6.98908626773821,13.9207331924292,-7.17545096943005));
#46481=CARTESIAN_POINT('Ctrl Pts',(6.98987652405541,13.9216984850986,-7.16798373863768));
#46482=CARTESIAN_POINT('Ctrl Pts',(6.9944022584873,13.9272266386557,-7.12521950787827));
#46483=CARTESIAN_POINT('Ctrl Pts',(6.99752057952379,13.9332694552473,-7.08133542937894));
#46484=CARTESIAN_POINT('Ctrl Pts',(6.99900427208156,13.9398281691519,-7.0364929204224));
#46485=CARTESIAN_POINT('Ctrl Pts',(6.99965344019274,13.9426978390811,-7.01687273247491));
#46486=CARTESIAN_POINT('Ctrl Pts',(6.99998929454039,13.9456662025399,-6.99706957208411));
#46487=CARTESIAN_POINT('Ctrl Pts',(6.99999076617782,13.9487330740186,-6.97709941303822));
#46488=CARTESIAN_POINT('Ctrl Pts',(6.99990203904237,13.888165173065,-6.87914443466826));
#46489=CARTESIAN_POINT('Ctrl Pts',(6.99990203904237,14.0922362660489,-7.13651751059625));
#46490=CARTESIAN_POINT('Ctrl Pts',(6.99990203904237,14.6760299602152,-7.80837580698534));
#46491=CARTESIAN_POINT('Ctrl Pts',(6.99990203904237,15.7555631911401,-8.78348152161194));
#46492=CARTESIAN_POINT('Ctrl Pts',(6.99990203904237,17.1681328395499,-9.70998929655117));
#46493=CARTESIAN_POINT('Ctrl Pts',(6.99990203904237,18.707836621519,-10.4111877922339));
#46494=CARTESIAN_POINT('Ctrl Pts',(6.99990203904237,20.3372593085727,-10.8675483426642));
#46495=CARTESIAN_POINT('Ctrl Pts',(6.99990203904237,22.0150966880212,-11.0696763778178));
#46496=CARTESIAN_POINT('Ctrl Pts',(6.99990203904237,23.3220446342241,-11.0250212390944));
#46497=CARTESIAN_POINT('Ctrl Pts',(6.99990203904237,24.0577248833002,-10.9251639976814));
#46498=CARTESIAN_POINT('Ctrl Pts',(6.99990203904237,24.2367456444932,-10.8963436960955));
#46499=CARTESIAN_POINT('Ctrl Pts',(7.00657991031323,13.5143482295687,-7.17552474229237));
#46500=CARTESIAN_POINT('Ctrl Pts',(7.00657991031323,13.7273208138437,-7.44412675674585));
#46501=CARTESIAN_POINT('Ctrl Pts',(7.00657991031323,14.3364361714447,-8.14510512450419));
#46502=CARTESIAN_POINT('Ctrl Pts',(7.00657991031323,15.4627111247065,-9.16244330636057));
#46503=CARTESIAN_POINT('Ctrl Pts',(7.00657991031323,16.9369683207059,-10.1294536145601));
#46504=CARTESIAN_POINT('Ctrl Pts',(7.00657991031323,18.5435357472038,-10.8610425695369));
#46505=CARTESIAN_POINT('Ctrl Pts',(7.00657991031323,20.2436295715865,-11.3372508338949));
#46506=CARTESIAN_POINT('Ctrl Pts',(7.00657991031323,21.9947633032354,-11.5481745874969));
#46507=CARTESIAN_POINT('Ctrl Pts',(7.00657991031323,23.3582294831803,-11.5015779615709));
#46508=CARTESIAN_POINT('Ctrl Pts',(7.00657991031323,24.1257769274139,-11.3974033892945));
#46509=CARTESIAN_POINT('Ctrl Pts',(7.00657991031323,24.3125682645583,-11.3673328815837));
#46510=CARTESIAN_POINT('Ctrl Pts',(6.71852921530218,13.2161068334526,-7.41198506936298));
#46511=CARTESIAN_POINT('Ctrl Pts',(6.71852921530218,13.4361812712895,-7.68954583852755));
#46512=CARTESIAN_POINT('Ctrl Pts',(6.71852921530218,14.0654989455187,-8.41375699680662));
#46513=CARTESIAN_POINT('Ctrl Pts',(6.71852921530218,15.2290657250872,-9.46478939774906));
#46514=CARTESIAN_POINT('Ctrl Pts',(6.71852921530218,16.752538936138,-10.4641137363018));
#46515=CARTESIAN_POINT('Ctrl Pts',(6.71852921530218,18.4124520095801,-11.2199490320946));
#46516=CARTESIAN_POINT('Ctrl Pts',(6.71852921530218,20.1689292029679,-11.7119923462326));
#46517=CARTESIAN_POINT('Ctrl Pts',(6.71852921530218,21.978540771934,-11.929933564917));
#46518=CARTESIAN_POINT('Ctrl Pts',(6.71852921530218,23.3870987467495,-11.8817879673256));
#46519=CARTESIAN_POINT('Ctrl Pts',(6.71852921530218,24.180070712107,-11.7741689102501));
#46520=CARTESIAN_POINT('Ctrl Pts',(6.71852921530218,24.3730616275822,-11.7431009538378));
#46521=CARTESIAN_POINT('Ctrl Pts',(6.25703473519962,13.1199246148395,-7.48824302405876));
#46522=CARTESIAN_POINT('Ctrl Pts',(6.25703473519962,13.3422893854061,-7.7686929726366));
#46523=CARTESIAN_POINT('Ctrl Pts',(6.25703473519962,13.978122263964,-8.50039665665675));
#46524=CARTESIAN_POINT('Ctrl Pts',(6.25703473519962,15.153715578534,-9.56229537189375));
#46525=CARTESIAN_POINT('Ctrl Pts',(6.25703473519962,16.6930608502105,-10.5720409168031));
#46526=CARTESIAN_POINT('Ctrl Pts',(6.25703473519962,18.3701777818156,-11.3356956061556));
#46527=CARTESIAN_POINT('Ctrl Pts',(6.25703473519962,20.1448384922945,-11.8328456903125));
#46528=CARTESIAN_POINT('Ctrl Pts',(6.25703473519962,21.973309039948,-12.0530500266267));
#46529=CARTESIAN_POINT('Ctrl Pts',(6.25703473519962,23.3964090231084,-12.0044048889509));
#46530=CARTESIAN_POINT('Ctrl Pts',(6.25703473519962,24.197580342684,-11.895674992817));
#46531=CARTESIAN_POINT('Ctrl Pts',(6.25703473519962,24.3925706090388,-11.8642853613214));
#46532=CARTESIAN_POINT('Ctrl Pts',(6.99999999999956,13.9487330738349,-6.97709941346457));
#46533=CARTESIAN_POINT('Ctrl Pts',(6.99999999999956,14.053386251496,-7.10629498286879));
#46534=CARTESIAN_POINT('Ctrl Pts',(6.99999999999324,14.1606435018721,-7.23273587370856));
#46535=CARTESIAN_POINT('Ctrl Pts',(6.99999999940879,14.2705233076618,-7.35652129864407));
#46536=CARTESIAN_POINT('Ctrl Pts',(6.999999998967,14.3535805484897,-7.45008968253378));
#46537=CARTESIAN_POINT('Ctrl Pts',(6.99999999822953,14.4381371927886,-7.54214022916443));
#46538=CARTESIAN_POINT('Ctrl Pts',(6.99999999797983,14.5242162277568,-7.63270296562204));
#46539=CARTESIAN_POINT('Ctrl Pts',(6.99999999764853,14.6384202201537,-7.75285563775258));
#46540=CARTESIAN_POINT('Ctrl Pts',(6.99999999919476,14.7553029036892,-7.87039100103324));
#46541=CARTESIAN_POINT('Ctrl Pts',(6.99999999987613,14.8749736388849,-7.98536856617627));
#46542=CARTESIAN_POINT('Ctrl Pts',(6.99999999995181,14.8882664665725,-7.99814008428295));
#46543=CARTESIAN_POINT('Ctrl Pts',(6.99999999999965,14.9015937278416,-8.0108800022357));
#46544=CARTESIAN_POINT('Ctrl Pts',(6.99999999999965,14.9149555972393,-8.02358837040624));
#46545=CARTESIAN_POINT('Ctrl Pts',(6.99999999999965,15.0622915543763,-8.16371843247603));
#46546=CARTESIAN_POINT('Ctrl Pts',(6.99999999555913,15.2137650538499,-8.3000557814469));
#46547=CARTESIAN_POINT('Ctrl Pts',(6.99999999493045,15.3690240498991,-8.43218410937023));
#46548=CARTESIAN_POINT('Ctrl Pts',(6.99999999439676,15.50082389845,-8.54434826122432));
#46549=CARTESIAN_POINT('Ctrl Pts',(6.9999999961049,15.6353509161497,-8.65347965096803));
#46550=CARTESIAN_POINT('Ctrl Pts',(6.99999999794295,15.7723688449927,-8.75934441784532));
#46551=CARTESIAN_POINT('Ctrl Pts',(6.99999999899899,15.8510917690786,-8.82016845800282));
#46552=CARTESIAN_POINT('Ctrl Pts',(6.99999999999965,15.9306366045598,-8.87991455028249));
#46553=CARTESIAN_POINT('Ctrl Pts',(6.99999999999965,16.0109493844193,-8.9385489450054));
#46554=CARTESIAN_POINT('Ctrl Pts',(6.99999999999965,16.2224433271297,-9.09295549574484));
#46555=CARTESIAN_POINT('Ctrl Pts',(6.99999999747041,16.4393240289556,-9.23958606259355));
#46556=CARTESIAN_POINT('Ctrl Pts',(6.99999999839021,16.661113395121,-9.37826165929473));
#46557=CARTESIAN_POINT('Ctrl Pts',(6.99999999909794,16.8317700681298,-9.48496612565262));
#46558=CARTESIAN_POINT('Ctrl Pts',(6.99999999994318,17.0053339299189,-9.58696026447865));
#46559=CARTESIAN_POINT('Ctrl Pts',(6.9999999999948,17.1816030196623,-9.6841487567417));
#46560=CARTESIAN_POINT('Ctrl Pts',(6.99999999999814,17.1930137959965,-9.69044025202934));
#46561=CARTESIAN_POINT('Ctrl Pts',(6.99999999999965,17.2044359132746,-9.69671160410671));
#46562=CARTESIAN_POINT('Ctrl Pts',(6.99999999999965,17.2158693153257,-9.70296278908558));
#46563=CARTESIAN_POINT('Ctrl Pts',(6.99999999999964,17.5300710084143,-9.87475180650998));
#46564=CARTESIAN_POINT('Ctrl Pts',(7.00000000000802,17.8527744443978,-10.0313270806561));
#46565=CARTESIAN_POINT('Ctrl Pts',(6.99999999997833,18.1824069034162,-10.1717696536148));
#46566=CARTESIAN_POINT('Ctrl Pts',(6.99999999996856,18.2908723305482,-10.2179822253646));
#46567=CARTESIAN_POINT('Ctrl Pts',(6.99999999999964,18.4000875899428,-10.2624481862356));
#46568=CARTESIAN_POINT('Ctrl Pts',(6.99999999999964,18.5099955100176,-10.3051352656413));
#46569=CARTESIAN_POINT('Ctrl Pts',(6.99999999999964,18.5790288315156,-10.3319470811539));
#46570=CARTESIAN_POINT('Ctrl Pts',(6.99999999997185,18.6483347586902,-10.3580596457169));
#46571=CARTESIAN_POINT('Ctrl Pts',(6.99999999993251,18.7178989046704,-10.3834658744547));
#46572=CARTESIAN_POINT('Ctrl Pts',(6.99999999971885,19.0956724624964,-10.5214363948426));
#46573=CARTESIAN_POINT('Ctrl Pts',(6.99999999999965,19.481061546552,-10.6385715529277));
#46574=CARTESIAN_POINT('Ctrl Pts',(6.99999999999965,19.8715517335095,-10.73431644707));
#46575=CARTESIAN_POINT('Ctrl Pts',(6.99999999999965,20.0280805593397,-10.772695992472));
#46576=CARTESIAN_POINT('Ctrl Pts',(6.99999999962334,20.1854297801842,-10.8076370879262));
#46577=CARTESIAN_POINT('Ctrl Pts',(6.99999999912728,20.3434768183341,-10.8391033410566));
#46578=CARTESIAN_POINT('Ctrl Pts',(6.99999999825512,20.6213539562873,-10.8944270754608));
#46579=CARTESIAN_POINT('Ctrl Pts',(6.99999999886831,20.9013888478931,-10.9390121158806));
#46580=CARTESIAN_POINT('Ctrl Pts',(6.99999999982003,21.1829146752606,-10.9726760530095));
#46581=CARTESIAN_POINT('Ctrl Pts',(6.99999999992606,21.2142778778935,-10.9764263621426));
#46582=CARTESIAN_POINT('Ctrl Pts',(6.99999999999964,21.2456595741147,-10.9800410779504));
#46583=CARTESIAN_POINT('Ctrl Pts',(6.99999999999964,21.2770588331736,-10.9835199089928));
#46584=CARTESIAN_POINT('Ctrl Pts',(6.99999999999964,21.4969229007099,-11.0078793991896));
#46585=CARTESIAN_POINT('Ctrl Pts',(6.99999999634621,21.7176500295301,-11.0256227319415));
#46586=CARTESIAN_POINT('Ctrl Pts',(6.99999999542167,21.9386318391872,-11.036675632778));
#46587=CARTESIAN_POINT('Ctrl Pts',(6.99999999531138,21.9649927459056,-11.0379941326508));
#46588=CARTESIAN_POINT('Ctrl Pts',(6.99999999523597,21.9913572760442,-11.0392174880406));
#46589=CARTESIAN_POINT('Ctrl Pts',(6.99999999520045,22.0177243973286,-11.0403456225131));
#46590=CARTESIAN_POINT('Ctrl Pts',(6.99999999489241,22.246398142798,-11.0501295777824));
#46591=CARTESIAN_POINT('Ctrl Pts',(6.99999999999965,22.4752661616617,-11.0527466161651));
#46592=CARTESIAN_POINT('Ctrl Pts',(6.99999999999965,22.703659797635,-11.048298338829));
#46593=CARTESIAN_POINT('Ctrl Pts',(6.99999999999965,22.873857685662,-11.0449835029986));
#46594=CARTESIAN_POINT('Ctrl Pts',(6.99999999741394,23.0437838324152,-11.0376888894721));
#46595=CARTESIAN_POINT('Ctrl Pts',(6.99999999745697,23.2135387084807,-11.0264498585388));
#46596=CARTESIAN_POINT('Ctrl Pts',(6.99999999749804,23.3755780199356,-11.0157216551667));
#46597=CARTESIAN_POINT('Ctrl Pts',(6.99999999865098,23.537461613108,-11.0013990881958));
#46598=CARTESIAN_POINT('Ctrl Pts',(6.99999999924031,23.6992764926518,-10.9834686168323));
#46599=CARTESIAN_POINT('Ctrl Pts',(6.99999999975841,23.8415378782003,-10.9677048396884));
#46600=CARTESIAN_POINT('Ctrl Pts',(6.99999999990827,23.9837463384243,-10.9491517994266));
#46601=CARTESIAN_POINT('Ctrl Pts',(6.99999999989361,24.1259362011698,-10.9277733096369));
#46602=CARTESIAN_POINT('Ctrl Pts',(6.26386081918706,13.9442638622873,-8.42073287772094));
#46603=CARTESIAN_POINT('Ctrl Pts',(6.26460715582258,14.1256644813049,-8.60589482522455));
#46604=CARTESIAN_POINT('Ctrl Pts',(6.26531568264654,14.3114848731865,-8.78358359448678));
#46605=CARTESIAN_POINT('Ctrl Pts',(6.26598638276582,14.5010844523376,-8.95374253421015));
#46606=CARTESIAN_POINT('Ctrl Pts',(6.26666473223493,14.6928464189228,-9.1258421404408));
#46607=CARTESIAN_POINT('Ctrl Pts',(6.26730438727457,14.8884742964778,-9.29023923288897));
#46608=CARTESIAN_POINT('Ctrl Pts',(6.26790533375421,15.087347270408,-9.44690789015415));
#46609=CARTESIAN_POINT('Ctrl Pts',(6.2680017616388,15.1192584319309,-9.47204694614937));
#46610=CARTESIAN_POINT('Ctrl Pts',(6.26809719288439,15.1512532324775,-9.49698708152831));
#46611=CARTESIAN_POINT('Ctrl Pts',(6.26819162743985,15.1833292053893,-9.52172826496564));
#46612=CARTESIAN_POINT('Ctrl Pts',(6.26876871395664,15.3793444393205,-9.67292083744168));
#46613=CARTESIAN_POINT('Ctrl Pts',(6.26930857994914,15.5783869659425,-9.81668210430068));
#46614=CARTESIAN_POINT('Ctrl Pts',(6.26981121523602,15.7798024932585,-9.95308866259111));
#46615=CARTESIAN_POINT('Ctrl Pts',(6.27017912285584,15.9272300797869,-10.0529324529055));
#46616=CARTESIAN_POINT('Ctrl Pts',(6.27052708374744,16.0759300700406,-10.1488363157099));
#46617=CARTESIAN_POINT('Ctrl Pts',(6.27085509470647,16.22566217413,-10.2408371004955));
#46618=CARTESIAN_POINT('Ctrl Pts',(6.27121137913853,16.3883006964033,-10.3407680523546));
#46619=CARTESIAN_POINT('Ctrl Pts',(6.27154412491034,16.5521567025934,-10.4360939682438));
#46620=CARTESIAN_POINT('Ctrl Pts',(6.27185332794175,16.716940010019,-10.5268693882174));
#46621=CARTESIAN_POINT('Ctrl Pts',(6.27227096943169,16.939513332523,-10.6494800284631));
#46622=CARTESIAN_POINT('Ctrl Pts',(6.2726456594972,17.1637763762107,-10.7637884182362));
#46623=CARTESIAN_POINT('Ctrl Pts',(6.27297739020537,17.3890721242152,-10.8699988364842));
#46624=CARTESIAN_POINT('Ctrl Pts',(6.27330912091355,17.6143678722197,-10.9762092547322));
#46625=CARTESIAN_POINT('Ctrl Pts',(6.27359789228358,17.8406965014528,-11.0743217864376));
#46626=CARTESIAN_POINT('Ctrl Pts',(6.27384369852514,18.0674570588809,-11.1645574428798));
#46627=CARTESIAN_POINT('Ctrl Pts',(6.27395596459215,18.1710244694238,-11.2057704006462));
#46628=CARTESIAN_POINT('Ctrl Pts',(6.27405926826201,18.2746827342572,-11.2453404763723));
#46629=CARTESIAN_POINT('Ctrl Pts',(6.27415361615965,18.378378353274,-11.2832898174722));
#46630=CARTESIAN_POINT('Ctrl Pts',(6.27415651998732,18.3815698839283,-11.2844578174955));
#46631=CARTESIAN_POINT('Ctrl Pts',(6.27415941527061,18.3847614500127,-11.2856242822539));
#46632=CARTESIAN_POINT('Ctrl Pts',(6.27416230201534,18.3879530500141,-11.2867892124062));
#46633=CARTESIAN_POINT('Ctrl Pts',(6.2742063116997,18.4366103860962,-11.3045490814075));
#46634=CARTESIAN_POINT('Ctrl Pts',(6.27424833682322,18.4852755954915,-11.3219522716654));
#46635=CARTESIAN_POINT('Ctrl Pts',(6.27428839799666,18.5339430794972,-11.3390020011574));
#46636=CARTESIAN_POINT('Ctrl Pts',(6.27431785037792,18.5697226927903,-11.3515367097095));
#46637=CARTESIAN_POINT('Ctrl Pts',(6.27434670195756,18.6061342225264,-11.3640966709816));
#46638=CARTESIAN_POINT('Ctrl Pts',(6.27437398859951,18.6418706456722,-11.3762337368752));
#46639=CARTESIAN_POINT('Ctrl Pts',(6.27438625180983,18.6579313714314,-11.3816883982454));
#46640=CARTESIAN_POINT('Ctrl Pts',(6.27439819893397,18.6738555054533,-11.3870583204017));
#46641=CARTESIAN_POINT('Ctrl Pts',(6.2744097424524,18.6895233175027,-11.3923060605731));
#46642=CARTESIAN_POINT('Ctrl Pts',(6.2745606466654,18.8943429191852,-11.4609078569345));
#46643=CARTESIAN_POINT('Ctrl Pts',(6.27467736471317,19.1037515567848,-11.5248695127819));
#46644=CARTESIAN_POINT('Ctrl Pts',(6.27475989485597,19.317573690524,-11.5836612029585));
#46645=CARTESIAN_POINT('Ctrl Pts',(6.2748410715206,19.5278891831466,-11.6414887209304));
#46646=CARTESIAN_POINT('Ctrl Pts',(6.27488917244077,19.7424746815811,-11.6943144438987));
#46647=CARTESIAN_POINT('Ctrl Pts',(6.27490419693318,19.9611183014331,-11.7416108905639));
#46648=CARTESIAN_POINT('Ctrl Pts',(6.27490863072152,20.0256409159614,-11.7555682628339));
#46649=CARTESIAN_POINT('Ctrl Pts',(6.27491018400937,20.0905166317593,-11.7690439544347));
#46650=CARTESIAN_POINT('Ctrl Pts',(6.27490885679481,20.1557392228451,-11.7820240144788));
#46651=CARTESIAN_POINT('Ctrl Pts',(6.27490450834956,20.369432529316,-11.8245514869826));
#46652=CARTESIAN_POINT('Ctrl Pts',(6.27486923880992,20.5868530263642,-11.861759892537));
#46653=CARTESIAN_POINT('Ctrl Pts',(6.27480304864361,20.807724782831,-11.8931692264645));
#46654=CARTESIAN_POINT('Ctrl Pts',(6.27475277000862,20.9755009200281,-11.917028033958));
#46655=CARTESIAN_POINT('Ctrl Pts',(6.27468465001575,21.1452675351015,-11.9375403860185));
#46656=CARTESIAN_POINT('Ctrl Pts',(6.27459868919133,21.3168848037213,-11.9544888514541));
#46657=CARTESIAN_POINT('Ctrl Pts',(6.27448994471055,21.5339887099896,-11.975929456359));
#46658=CARTESIAN_POINT('Ctrl Pts',(6.27435264765825,21.7540558527808,-11.9916671410961));
#46659=CARTESIAN_POINT('Ctrl Pts',(6.27418680051457,21.9767636838208,-12.0012474184625));
#46660=CARTESIAN_POINT('Ctrl Pts',(6.27401315051287,22.2099495824815,-12.0112784334326));
#46661=CARTESIAN_POINT('Ctrl Pts',(6.27380820073295,22.4460306168683,-12.0145579480249));
#46662=CARTESIAN_POINT('Ctrl Pts',(6.27357195495289,22.6846268922175,-12.0106606315315));
#46663=CARTESIAN_POINT('Ctrl Pts',(6.27333930220717,22.9195943848128,-12.0068225888672));
#46664=CARTESIAN_POINT('Ctrl Pts',(6.2730762981723,23.1570012478186,-11.996024327057));
#46665=CARTESIAN_POINT('Ctrl Pts',(6.27278294744759,23.3964344665696,-11.9778551667814));
#46666=CARTESIAN_POINT('Ctrl Pts',(6.27261681610617,23.5320310697448,-11.9675655485371));
#46667=CARTESIAN_POINT('Ctrl Pts',(6.27244095193068,23.6682766505981,-11.9549118418849));
#46668=CARTESIAN_POINT('Ctrl Pts',(6.27225535591025,23.8050887673702,-11.9398188606727));
#46669=CARTESIAN_POINT('Ctrl Pts',(6.27204648314437,23.9590593383348,-11.9228329752875));
#46670=CARTESIAN_POINT('Ctrl Pts',(6.27182528439318,24.1137477394466,-11.9027576366664));
#46671=CARTESIAN_POINT('Ctrl Pts',(6.27159176124975,24.2690119676725,-11.8794807215117));
#46672=CARTESIAN_POINT('Ctrl Pts',(-6.390310997178,13.7249660550952,-8.13937950338793));
#46673=CARTESIAN_POINT('Ctrl Pts',(-4.260207331452,13.8221738588746,-9.11426650158688));
#46674=CARTESIAN_POINT('Ctrl Pts',(0.0001535202327188,13.918298461743,-10.0902631574918));
#46675=CARTESIAN_POINT('Ctrl Pts',(4.260514371917,13.8221669310088,-9.11419615982883));
#46676=CARTESIAN_POINT('Ctrl Pts',(6.390771557876,13.7249450365303,-8.13916871045812));
#46677=CARTESIAN_POINT('Ctrl Pts',(-6.390310997178,14.2543287817271,-8.71309690459039));
#46678=CARTESIAN_POINT('Ctrl Pts',(-4.260207331452,14.3567676707027,-9.62713419180366));
#46679=CARTESIAN_POINT('Ctrl Pts',(0.0001535202327188,14.4578350530778,
-10.5425537312138));
#46680=CARTESIAN_POINT('Ctrl Pts',(4.260514371917,14.3567603866034,-9.62706821594453));
#46681=CARTESIAN_POINT('Ctrl Pts',(6.390771557876,14.2543066320775,-8.71289926876272));
#46682=CARTESIAN_POINT('Ctrl Pts',(-6.390310997178,15.6641218054918,-9.96973300997693));
#46683=CARTESIAN_POINT('Ctrl Pts',(-4.260207331452,15.7526919792829,-10.7489906364333));
#46684=CARTESIAN_POINT('Ctrl Pts',(0.0001535202327188,15.8421753984554,
-11.5273040839069));
#46685=CARTESIAN_POINT('Ctrl Pts',(4.260514371917,15.752685530061,-10.7489345420424));
#46686=CARTESIAN_POINT('Ctrl Pts',(6.390771557876,15.6641026545996,-9.96956451659077));
#46687=CARTESIAN_POINT('Ctrl Pts',(-6.390310997178,18.3168609125034,-11.3879809585253));
#46688=CARTESIAN_POINT('Ctrl Pts',(-4.260207331452,18.305065900394,-12.0191857141961));
#46689=CARTESIAN_POINT('Ctrl Pts',(0.0001535202327188,18.2929947853426,
-12.6510838649568));
#46690=CARTESIAN_POINT('Ctrl Pts',(4.260514371917,18.3050667703745,-12.0191401722118));
#46691=CARTESIAN_POINT('Ctrl Pts',(6.390771557876,18.3168634628528,-11.3878444775859));
#46692=CARTESIAN_POINT('Ctrl Pts',(-6.390310997178,21.4528914163287,-12.0713618431433));
#46693=CARTESIAN_POINT('Ctrl Pts',(-4.260207331452,21.2792389757137,-12.6592425324047));
#46694=CARTESIAN_POINT('Ctrl Pts',(0.0001535202327188,21.1056340488841,
-13.2456889758127));
#46695=CARTESIAN_POINT('Ctrl Pts',(4.260514371917,21.2792514877189,-12.6592002662047));
#46696=CARTESIAN_POINT('Ctrl Pts',(6.390771557876,21.4529289639727,-12.071234729827));
#46697=CARTESIAN_POINT('Ctrl Pts',(-6.390310997178,23.5458951845797,-11.9720502124699));
#46698=CARTESIAN_POINT('Ctrl Pts',(-4.260207331452,23.2652553028773,-12.6077625569466));
#46699=CARTESIAN_POINT('Ctrl Pts',(0.0001535202327188,22.9846380445226,
-13.2461450660854));
#46700=CARTESIAN_POINT('Ctrl Pts',(4.260514371917,23.265275527447,-12.607716547628));
#46701=CARTESIAN_POINT('Ctrl Pts',(6.390771557876,23.5459558653553,-11.9719127568894));
#46702=CARTESIAN_POINT('Ctrl Pts',(-6.390310997178,24.5118462831574,-11.8061936876057));
#46703=CARTESIAN_POINT('Ctrl Pts',(-4.260207331452,24.1870546128076,-12.4817978962268));
#46704=CARTESIAN_POINT('Ctrl Pts',(0.0001535202327188,23.8622603664262,
-13.1582606881552));
#46705=CARTESIAN_POINT('Ctrl Pts',(4.260514371917,24.1870780212844,-12.4817491423853));
#46706=CARTESIAN_POINT('Ctrl Pts',(6.390771557876,24.5119165105666,-11.8060476064867));
#46707=CARTESIAN_POINT('Ctrl Pts',(-6.26386059966982,13.9442583573344,-8.42071137120996));
#46708=CARTESIAN_POINT('Ctrl Pts',(-5.97465264562961,13.9555888069264,-8.54542713090756));
#46709=CARTESIAN_POINT('Ctrl Pts',(-5.68350292691887,13.9652820825191,-8.66149310003109));
#46710=CARTESIAN_POINT('Ctrl Pts',(-5.3909022605167,13.9735953815832,-8.76876193425704));
#46711=CARTESIAN_POINT('Ctrl Pts',(-5.11637639590315,13.981395143769,-8.86940445781674));
#46712=CARTESIAN_POINT('Ctrl Pts',(-4.84057330552681,13.9879803358116,-8.96230247036302));
#46713=CARTESIAN_POINT('Ctrl Pts',(-4.56389835177543,13.9935747005038,-9.04737600273165));
#46714=CARTESIAN_POINT('Ctrl Pts',(-4.30687417419982,13.9987717267058,-9.12640720665533));
#46715=CARTESIAN_POINT('Ctrl Pts',(-4.04909758291724,14.0031137981319,-9.19868567286897));
#46716=CARTESIAN_POINT('Ctrl Pts',(-3.79089355733771,14.0067883134942,-9.26419037750946));
#46717=CARTESIAN_POINT('Ctrl Pts',(-3.57421217307386,14.0098719179168,-9.31916105445936));
#46718=CARTESIAN_POINT('Ctrl Pts',(-3.35722977490934,14.0124855440924,-9.36936192851386));
#46719=CARTESIAN_POINT('Ctrl Pts',(-3.14013842049977,14.0147440106155,-9.41480879995396));
#46720=CARTESIAN_POINT('Ctrl Pts',(-2.90223992213209,14.0172189401027,-9.46461153162198));
#46721=CARTESIAN_POINT('Ctrl Pts',(-2.66419710898026,14.0192828053626,-9.50872061924435));
#46722=CARTESIAN_POINT('Ctrl Pts',(-2.42625893543512,14.0209898784393,-9.54710744779563));
#46723=CARTESIAN_POINT('Ctrl Pts',(-2.19167929327942,14.0226728559351,-9.58495244076538));
#46724=CARTESIAN_POINT('Ctrl Pts',(-1.95720135757247,14.0240090622126,-9.61723553947319));
#46725=CARTESIAN_POINT('Ctrl Pts',(-1.72306368872734,14.0250552895158,-9.6439797497153));
#46726=CARTESIAN_POINT('Ctrl Pts',(-1.49041851325521,14.0260948477199,-9.67055348095356));
#46727=CARTESIAN_POINT('Ctrl Pts',(-1.25810928045884,14.0268481255946,-9.69165864347421));
#46728=CARTESIAN_POINT('Ctrl Pts',(-1.02637001771251,14.027375357038,-9.70736883014928));
#46729=CARTESIAN_POINT('Ctrl Pts',(-0.796211217154453,14.0278989927621,
-9.722971873323));
#46730=CARTESIAN_POINT('Ctrl Pts',(-0.566614638763602,14.0281996676435,
-9.73325324451101));
#46731=CARTESIAN_POINT('Ctrl Pts',(-0.337809554294219,14.028340667515,-9.73833628894296));
#46732=CARTESIAN_POINT('Ctrl Pts',(-0.225004826403271,14.0284101828064,
-9.74084231473926));
#46733=CARTESIAN_POINT('Ctrl Pts',(-0.112392483352252,14.0284409511869,
-9.74208559867157));
#46734=CARTESIAN_POINT('Ctrl Pts',(1.4050982599656E-12,14.0284409294389,
-9.74208557976265));
#46735=CARTESIAN_POINT('Ctrl Pts',(7.81016580919136E-6,14.0284409294374,
-9.74208557976133));
#46736=CARTESIAN_POINT('Ctrl Pts',(1.56203291527005E-5,14.0284409294358,
-9.74208557975401));
#46737=CARTESIAN_POINT('Ctrl Pts',(2.34304914347674E-5,14.028440929434,
-9.7420855797407));
#46738=CARTESIAN_POINT('Ctrl Pts',(0.230478574994379,14.0284408760724,-9.74208518673622));
#46739=CARTESIAN_POINT('Ctrl Pts',(0.461829118783569,14.0283110143972,-9.73685417253584));
#46740=CARTESIAN_POINT('Ctrl Pts',(0.693851093705858,14.0279842381151,-9.72624199356124));
#46741=CARTESIAN_POINT('Ctrl Pts',(0.927871388852005,14.0276546474287,-9.71553841577896));
#46742=CARTESIAN_POINT('Ctrl Pts',(1.16257473051679,14.0271247222249,-9.69936059187738));
#46743=CARTESIAN_POINT('Ctrl Pts',(1.39773131369698,14.0263298736297,-9.67760707303488));
#46744=CARTESIAN_POINT('Ctrl Pts',(1.63446134054756,14.0255297066655,-9.65570800038278));
#46745=CARTESIAN_POINT('Ctrl Pts',(1.87165069452548,14.0244610452605,-9.62815843071653));
#46746=CARTESIAN_POINT('Ctrl Pts',(2.1090649267855,14.0230625066786,-9.59490779642856));
#46747=CARTESIAN_POINT('Ctrl Pts',(2.34947150989978,14.0216463410233,-9.56123807368507));
#46748=CARTESIAN_POINT('Ctrl Pts',(2.59010867571746,14.0198919107936,-9.52172271517559));
#46749=CARTESIAN_POINT('Ctrl Pts',(2.830732998265,14.0177403552189,-9.47636256609525));
#46750=CARTESIAN_POINT('Ctrl Pts',(2.93369717152342,14.0168196954177,-9.45695276496006));
#46751=CARTESIAN_POINT('Ctrl Pts',(3.03665899315264,14.0158263831013,-9.43647342566048));
#46752=CARTESIAN_POINT('Ctrl Pts',(3.1395993906909,14.0147560870973,-9.41492750001361));
#46753=CARTESIAN_POINT('Ctrl Pts',(3.402364148134,14.0120240588886,-9.35992955885661));
#46754=CARTESIAN_POINT('Ctrl Pts',(3.66498146129631,14.0087716270681,-9.29796291359547));
#46755=CARTESIAN_POINT('Ctrl Pts',(3.92711006179015,14.0047954811542,-9.22900273258147));
#46756=CARTESIAN_POINT('Ctrl Pts',(4.19749553574368,14.0006940893358,-9.1578703525502));
#46757=CARTESIAN_POINT('Ctrl Pts',(4.46736102388801,13.9958226091972,-9.07929746709712));
#46758=CARTESIAN_POINT('Ctrl Pts',(4.73633198217297,13.9899668452079,-8.99331689554591));
#46759=CARTESIAN_POINT('Ctrl Pts',(5.03090948501449,13.9835536013982,-8.89915081076881));
#46760=CARTESIAN_POINT('Ctrl Pts',(5.32441402864121,13.9759595147058,-8.79609975055995));
#46761=CARTESIAN_POINT('Ctrl Pts',(5.61635358998981,13.9669161746218,-8.68427180594349));
#46762=CARTESIAN_POINT('Ctrl Pts',(5.83311830245842,13.9602015073668,-8.60123971481899));
#46763=CARTESIAN_POINT('Ctrl Pts',(6.04902023369438,13.9526881277119,-8.51337040698944));
#46764=CARTESIAN_POINT('Ctrl Pts',(6.26385797771861,13.9442712878222,-8.42072561445923));
#46765=CARTESIAN_POINT('Ctrl Pts',(-6.38374306817848,13.9414234665096,-8.37048976079463));
#46766=CARTESIAN_POINT('Ctrl Pts',(-5.82059584927031,13.9721064314624,-8.62634823145341));
#46767=CARTESIAN_POINT('Ctrl Pts',(-4.49614362021116,14.0259437405025,-9.14100802794636));
#46768=CARTESIAN_POINT('Ctrl Pts',(-2.35438543985914,14.0657479998801,-9.65806327216457));
#46769=CARTESIAN_POINT('Ctrl Pts',(0.000944862534166641,14.0770613980891,
-9.84571566180163));
#46770=CARTESIAN_POINT('Ctrl Pts',(2.35625308012023,14.0657286201865,-9.65776341049157));
#46771=CARTESIAN_POINT('Ctrl Pts',(4.49734856102933,14.0259052114703,-9.14058936099707));
#46772=CARTESIAN_POINT('Ctrl Pts',(5.82117757776206,13.9720747788879,-8.62608431902301));
#46773=CARTESIAN_POINT('Ctrl Pts',(6.38374993440966,13.9414230799749,-8.37048666385961));
#46774=CARTESIAN_POINT('Ctrl Pts',(-6.1773119863258,13.4690909032843,-7.96436356123403));
#46775=CARTESIAN_POINT('Ctrl Pts',(-5.63207697424702,13.500338411862,-8.21046045032616));
#46776=CARTESIAN_POINT('Ctrl Pts',(-4.34991588258102,13.5555619320176,-8.70553669287808));
#46777=CARTESIAN_POINT('Ctrl Pts',(-2.2774119989541,13.5972251815216,-9.20285462796731));
#46778=CARTESIAN_POINT('Ctrl Pts',(0.00091390089760303,13.609319564241,
-9.38330152096535));
#46779=CARTESIAN_POINT('Ctrl Pts',(2.27921883855988,13.5972045992365,-9.20256625844348));
#46780=CARTESIAN_POINT('Ctrl Pts',(4.35108223317131,13.5555221053603,-8.70513395156023));
#46781=CARTESIAN_POINT('Ctrl Pts',(5.63264019878497,13.5003061784947,-8.21020660346642));
#46782=CARTESIAN_POINT('Ctrl Pts',(6.17731863567807,13.4690905112704,-7.96436057927722));
#46783=CARTESIAN_POINT('Ctrl Pts',(-6.17551155032075,12.8181924090209,-8.03300126784152));
#46784=CARTESIAN_POINT('Ctrl Pts',(-5.63170106673364,12.8491198316558,-8.27611256190061));
#46785=CARTESIAN_POINT('Ctrl Pts',(-4.35219500761121,12.903814214672,-8.76567194552832));
#46786=CARTESIAN_POINT('Ctrl Pts',(-2.28031100801065,12.9451038841067,-9.25865895634552));
#46787=CARTESIAN_POINT('Ctrl Pts',(0.000915364060213764,12.9570860883808,
-9.43787048445677));
#46788=CARTESIAN_POINT('Ctrl Pts',(2.28211904695125,12.9450834869878,-9.2583727115523));
#46789=CARTESIAN_POINT('Ctrl Pts',(4.35335943163024,12.9037747559201,-8.76527331312379));
#46790=CARTESIAN_POINT('Ctrl Pts',(5.63226282281907,12.8490879200421,-8.27586179676238));
#46791=CARTESIAN_POINT('Ctrl Pts',(6.17551817586046,12.8181920167498,-8.03299832752118));
#46792=CARTESIAN_POINT('Ctrl Pts',(-6.37708413694345,12.4375777136251,-8.52351639529135));
#46793=CARTESIAN_POINT('Ctrl Pts',(-5.81743381263044,12.467530855356,-8.77238436612168));
#46794=CARTESIAN_POINT('Ctrl Pts',(-4.49960759980687,12.5201672053427,-9.2741081038561));
#46795=CARTESIAN_POINT('Ctrl Pts',(-2.36011990204123,12.5591342919587,-9.78095493227011));
#46796=CARTESIAN_POINT('Ctrl Pts',(0.000947852883720792,12.5701990184725,
-9.9656762487021));
#46797=CARTESIAN_POINT('Ctrl Pts',(2.36198956188397,12.5591153237873,-9.78066010083845));
#46798=CARTESIAN_POINT('Ctrl Pts',(4.50080763630646,12.5201295072611,-9.27369908790463));
#46799=CARTESIAN_POINT('Ctrl Pts',(5.81801193592241,12.4674999362466,-8.77212766913687));
#46800=CARTESIAN_POINT('Ctrl Pts',(6.37709094572465,12.4375773264369,-8.5235133956001));
#46801=CARTESIAN_POINT('Ctrl Pts',(-6.24994498501116,12.4626511593801,-8.55169008625593));
#46802=CARTESIAN_POINT('Ctrl Pts',(-5.93338368633412,12.4790326845279,-8.68959465523929));
#46803=CARTESIAN_POINT('Ctrl Pts',(-5.61265410177717,12.4932118124037,-8.81761728472444));
#46804=CARTESIAN_POINT('Ctrl Pts',(-5.28814114363494,12.5055419053853,-8.93533874511386));
#46805=CARTESIAN_POINT('Ctrl Pts',(-5.1109010599461,12.5122762642363,-8.99963498034231));
#46806=CARTESIAN_POINT('Ctrl Pts',(-4.93253192895896,12.5184587937767,-9.06085758779078));
#46807=CARTESIAN_POINT('Ctrl Pts',(-4.75309372274156,12.524145498013,-9.11893249178345));
#46808=CARTESIAN_POINT('Ctrl Pts',(-4.7187542017193,12.5252337762776,-9.13004642581435));
#46809=CARTESIAN_POINT('Ctrl Pts',(-4.68437576021377,12.5263036996257,-9.14104524604668));
#46810=CARTESIAN_POINT('Ctrl Pts',(-4.64995872620909,12.5273556136019,-9.15192850758437));
#46811=CARTESIAN_POINT('Ctrl Pts',(-4.42981456654124,12.5340840469209,-9.22154189917806));
#46812=CARTESIAN_POINT('Ctrl Pts',(-4.20809199462032,12.5400758465265,-9.28642855434412));
#46813=CARTESIAN_POINT('Ctrl Pts',(-3.98492302615565,12.5454105664597,-9.34648339944226));
#46814=CARTESIAN_POINT('Ctrl Pts',(-3.85589357770526,12.548494937801,-9.3812052677786));
#46815=CARTESIAN_POINT('Ctrl Pts',(-3.72638058446272,12.5513591804004,-9.41431224523432));
#46816=CARTESIAN_POINT('Ctrl Pts',(-3.59641035002401,12.5540151891641,-9.44578546448643));
#46817=CARTESIAN_POINT('Ctrl Pts',(-3.52576868899392,12.5554587879357,-9.46289184654025));
#46818=CARTESIAN_POINT('Ctrl Pts',(-3.45554254859571,12.5568302224045,-9.47938649079335));
#46819=CARTESIAN_POINT('Ctrl Pts',(-3.38483967534512,12.5581489342279,-9.49548180717088));
#46820=CARTESIAN_POINT('Ctrl Pts',(-3.325459692702,12.5592564576084,-9.50899949836493));
#46821=CARTESIAN_POINT('Ctrl Pts',(-3.26574318462488,12.560326673833,-9.52223473200989));
#46822=CARTESIAN_POINT('Ctrl Pts',(-3.2051550313525,12.5613679886932,-9.5352858943859));
#46823=CARTESIAN_POINT('Ctrl Pts',(-2.91383358558888,12.566374864364,-9.59803881367665));
#46824=CARTESIAN_POINT('Ctrl Pts',(-2.62163059281673,12.5704045423175,-9.6523014102567));
#46825=CARTESIAN_POINT('Ctrl Pts',(-2.32883742188271,12.5736768622578,-9.69794699246654));
#46826=CARTESIAN_POINT('Ctrl Pts',(-2.02607568806039,12.5770605930176,-9.74514664390341));
#46827=CARTESIAN_POINT('Ctrl Pts',(-1.72268277929252,12.5796341126242,-9.78313345602961));
#46828=CARTESIAN_POINT('Ctrl Pts',(-1.41906580927046,12.58151618669,-9.81191700308478));
#46829=CARTESIAN_POINT('Ctrl Pts',(-1.11206495483235,12.5834192369255,-9.84102134971946));
#46830=CARTESIAN_POINT('Ctrl Pts',(-0.804834430918333,12.5846152787206,
-9.86071627118328));
#46831=CARTESIAN_POINT('Ctrl Pts',(-0.49777905948838,12.585220668062,-9.87096135196521));
#46832=CARTESIAN_POINT('Ctrl Pts',(-0.33177214009757,12.5855479667479,-9.87650026923474));
#46833=CARTESIAN_POINT('Ctrl Pts',(-0.165816194680363,12.5857025170598,
-9.87927618530277));
#46834=CARTESIAN_POINT('Ctrl Pts',(2.58171329915067E-5,12.5857020423694,
-9.87927649675614));
#46835=CARTESIAN_POINT('Ctrl Pts',(0.000327485249286301,12.5857020415059,
-9.87927649732267));
#46836=CARTESIAN_POINT('Ctrl Pts',(0.000629153722568615,12.5857020401084,
-9.87927648873088));
#46837=CARTESIAN_POINT('Ctrl Pts',(0.00093082255248277,12.5857020381768,
-9.87927647098056));
#46838=CARTESIAN_POINT('Ctrl Pts',(0.29883321452666,12.5857001307359,-9.879258942275));
#46839=CARTESIAN_POINT('Ctrl Pts',(0.597084493922628,12.5851778676453,-9.87031429001266));
#46840=CARTESIAN_POINT('Ctrl Pts',(0.895336025094607,12.5840597930142,-9.85247090002633));
#46841=CARTESIAN_POINT('Ctrl Pts',(1.13208149249359,12.5831722901064,-9.83830721179413));
#46842=CARTESIAN_POINT('Ctrl Pts',(1.36882702253841,12.5819093075633,-9.81853557990205));
#46843=CARTESIAN_POINT('Ctrl Pts',(1.60539033451399,12.5802306826658,-9.79314830718627));
#46844=CARTESIAN_POINT('Ctrl Pts',(1.84741516945489,12.5785133034562,-9.76717492003117));
#46845=CARTESIAN_POINT('Ctrl Pts',(2.08925199887728,12.5763522816075,-9.73533445771998));
#46846=CARTESIAN_POINT('Ctrl Pts',(2.33070782969548,12.5736597148678,-9.69765040163421));
#46847=CARTESIAN_POINT('Ctrl Pts',(2.35606681193083,12.5733769271136,-9.69369262059576));
#46848=CARTESIAN_POINT('Ctrl Pts',(2.38142158883918,12.5730882736115,-9.68967036268841));
#46849=CARTESIAN_POINT('Ctrl Pts',(2.40677199762222,12.5727935830512,-9.68558375444369));
#46850=CARTESIAN_POINT('Ctrl Pts',(2.54013430131214,12.5712432880506,-9.66408510744125));
#46851=CARTESIAN_POINT('Ctrl Pts',(2.67337439519718,12.5695272160787,-9.64080421635102));
#46852=CARTESIAN_POINT('Ctrl Pts',(2.80646029870055,12.5676287808786,-9.61574910601489));
#46853=CARTESIAN_POINT('Ctrl Pts',(2.87846051899447,12.5666017167868,-9.60219415078521));
#46854=CARTESIAN_POINT('Ctrl Pts',(2.9509727355371,12.5655128307827,-9.58801061068387));
#46855=CARTESIAN_POINT('Ctrl Pts',(3.02308661174239,12.5643722825228,-9.57337240027714));
#46856=CARTESIAN_POINT('Ctrl Pts',(3.0842687217262,12.5634046303489,-9.56095320100236));
#46857=CARTESIAN_POINT('Ctrl Pts',(3.14516423945337,12.5623998611268,-9.54820765663932));
#46858=CARTESIAN_POINT('Ctrl Pts',(3.20522363885174,12.5613672627394,-9.53527055144678));
#46859=CARTESIAN_POINT('Ctrl Pts',(3.52196512413216,12.5559215415006,-9.46704279767362));
#46860=CARTESIAN_POINT('Ctrl Pts',(3.8362022023586,12.5493532214616,-9.3890832650296));
#46861=CARTESIAN_POINT('Ctrl Pts',(4.14754504429288,12.541448947496,-9.30172845627976));
#46862=CARTESIAN_POINT('Ctrl Pts',(4.31648149642719,12.5371600420817,-9.25432922469509));
#46863=CARTESIAN_POINT('Ctrl Pts',(4.48456554909833,12.5324777247987,-9.20416294759299));
#46864=CARTESIAN_POINT('Ctrl Pts',(4.65173253716364,12.5273671479188,-9.15127749971604));
#46865=CARTESIAN_POINT('Ctrl Pts',(4.9647529062626,12.5177975870876,-9.05224944037253));
#46866=CARTESIAN_POINT('Ctrl Pts',(5.27455949898563,12.5067271099657,-8.94368979231894));
#46867=CARTESIAN_POINT('Ctrl Pts',(5.58085220748431,12.4938926574309,-8.82593410453551));
#46868=CARTESIAN_POINT('Ctrl Pts',(5.80582191344839,12.4844658479352,-8.73944343165569));
#46869=CARTESIAN_POINT('Ctrl Pts',(6.02889546083625,12.4740872407875,-8.64799069239423));
#46870=CARTESIAN_POINT('Ctrl Pts',(6.24994363575164,12.4626483740505,-8.5516948379668));
#46871=CARTESIAN_POINT('Ctrl Pts',(7.10529336472858,7.16048923499633,-14.3567206907318));
#46872=CARTESIAN_POINT('Ctrl Pts',(7.1064275368113,7.24034649935247,-14.3164705260865));
#46873=CARTESIAN_POINT('Ctrl Pts',(7.09037559920597,7.42259570938419,-14.2296084470487));
#46874=CARTESIAN_POINT('Ctrl Pts',(7.00203596961012,7.70267882729892,-14.1129068657706));
#46875=CARTESIAN_POINT('Ctrl Pts',(6.84111528275874,7.97637671077655,-14.0188435983679));
#46876=CARTESIAN_POINT('Ctrl Pts',(6.62715076555215,8.20731154449834,-13.9610638995495));
#46877=CARTESIAN_POINT('Ctrl Pts',(6.42119926597592,8.35211939072247,-13.9452161478941));
#46878=CARTESIAN_POINT('Ctrl Pts',(6.29197222530054,8.41580527600954,-13.9494152732194));
#46879=CARTESIAN_POINT('Ctrl Pts',(6.25107867181893,8.43351433517937,-13.9520220265804));
#46880=CARTESIAN_POINT('Ctrl Pts',(6.81695434203023,6.90423125129657,-13.8395073332205));
#46881=CARTESIAN_POINT('Ctrl Pts',(6.81797118283742,6.97460530088759,-13.8040212512093));
#46882=CARTESIAN_POINT('Ctrl Pts',(6.80354599269152,7.13572701890584,-13.7274488397656));
#46883=CARTESIAN_POINT('Ctrl Pts',(6.72389639326869,7.38404253596884,-13.6251523381992));
#46884=CARTESIAN_POINT('Ctrl Pts',(6.57905010989704,7.62656630202561,-13.5437450468964));
#46885=CARTESIAN_POINT('Ctrl Pts',(6.38723329244376,7.83061781411381,-13.4949402802546));
#46886=CARTESIAN_POINT('Ctrl Pts',(6.20363484828439,7.95800648462909,-13.4827503106996));
#46887=CARTESIAN_POINT('Ctrl Pts',(6.08903468842784,8.01384149509141,-13.4872621068598));
#46888=CARTESIAN_POINT('Ctrl Pts',(6.05283226078958,8.02935410316426,-13.489777394369));
#46889=CARTESIAN_POINT('Ctrl Pts',(7.05875964334239,6.63234584950194,-13.3065825231142));
#46890=CARTESIAN_POINT('Ctrl Pts',(7.06010346820671,6.72332482551982,-13.260728454359));
#46891=CARTESIAN_POINT('Ctrl Pts',(7.04118734267824,6.92988246936252,-13.1622551946321));
#46892=CARTESIAN_POINT('Ctrl Pts',(6.93788435052611,7.24649106248276,-13.0301399355402));
#46893=CARTESIAN_POINT('Ctrl Pts',(6.74896177210885,7.55747236941287,-12.9230480356511));
#46894=CARTESIAN_POINT('Ctrl Pts',(6.49540659457737,7.8226841502203,-12.8567005545142));
#46895=CARTESIAN_POINT('Ctrl Pts',(6.24819682300408,7.99157414700557,-12.8385724942454));
#46896=CARTESIAN_POINT('Ctrl Pts',(6.09125158425211,8.06689842540132,-12.8439943442258));
#46897=CARTESIAN_POINT('Ctrl Pts',(6.04139644311579,8.08794686373372,-12.8472574438417));
#46898=CARTESIAN_POINT('Ctrl Pts',(7.66735121800432,6.52877730330966,-13.1185037491408));
#46899=CARTESIAN_POINT('Ctrl Pts',(7.66924531506772,6.65652225417889,-13.0541574622128));
#46900=CARTESIAN_POINT('Ctrl Pts',(7.64275624394143,6.9443687062556,-12.9163957628901));
#46901=CARTESIAN_POINT('Ctrl Pts',(7.49944502218963,7.38317117659575,-12.7303924191653));
#46902=CARTESIAN_POINT('Ctrl Pts',(7.23608901619539,7.81597033812076,-12.5766354500427));
#46903=CARTESIAN_POINT('Ctrl Pts',(6.87864190335745,8.18904651334705,-12.4780845072667));
#46904=CARTESIAN_POINT('Ctrl Pts',(6.52485516459777,8.43030637575862,-12.4484356813334));
#46905=CARTESIAN_POINT('Ctrl Pts',(6.29721660236423,8.53928654730601,-12.4547495191759));
#46906=CARTESIAN_POINT('Ctrl Pts',(6.22459365164253,8.56986120938434,-12.4590941392797));
#46907=CARTESIAN_POINT('',(6.26385989003177,8.42071839535226,-13.9442649557177));
#46908=CARTESIAN_POINT('',(6.24994593946664,8.55169414006259,-12.4626532547806));
#46909=CARTESIAN_POINT('Ctrl Pts',(6.26385687510184,8.42071068624793,-13.9442728359392));
#46910=CARTESIAN_POINT('Ctrl Pts',(6.25434589570407,8.4015288148462,-13.9218689631775));
#46911=CARTESIAN_POINT('Ctrl Pts',(6.24501143579651,8.38292246516115,-13.8980040452737));
#46912=CARTESIAN_POINT('Ctrl Pts',(6.23595649835892,8.36511937125287,-13.8726943205492));
#46913=CARTESIAN_POINT('Ctrl Pts',(6.22712817822746,8.34776183417036,-13.8480180205917));
#46914=CARTESIAN_POINT('Ctrl Pts',(6.21856585461717,8.33116854811689,-13.8219680644561));
#46915=CARTESIAN_POINT('Ctrl Pts',(6.21037090452425,8.31555920420894,-13.7946076666852));
#46916=CARTESIAN_POINT('Ctrl Pts',(6.20230230129337,8.30019051968255,-13.7676691019167));
#46917=CARTESIAN_POINT('Ctrl Pts',(6.19459015268015,8.28577642744152,-13.7394600730491));
#46918=CARTESIAN_POINT('Ctrl Pts',(6.18733252944957,8.27252438528487,-13.7100911322866));
#46919=CARTESIAN_POINT('Ctrl Pts',(6.18020247023623,8.25950526838217,-13.6812383963404));
#46920=CARTESIAN_POINT('Ctrl Pts',(6.17351143247687,8.24760846707906,-13.651266308102));
#46921=CARTESIAN_POINT('Ctrl Pts',(6.16734883482834,8.23701734476728,-13.6203283182696));
#46922=CARTESIAN_POINT('Ctrl Pts',(6.16655150095895,8.23564703617086,-13.6163254758725));
#46923=CARTESIAN_POINT('Ctrl Pts',(6.16576300405729,8.2342985566984,-13.6123065298336));
#46924=CARTESIAN_POINT('Ctrl Pts',(6.16498352875401,8.23297227653974,-13.6082718703713));
#46925=CARTESIAN_POINT('Ctrl Pts',(6.15905115567951,8.222878321453,-13.5775651820919));
#46926=CARTESIAN_POINT('Ctrl Pts',(6.15364235588507,8.21407261921391,-13.5459450166987));
#46927=CARTESIAN_POINT('Ctrl Pts',(6.14883171670341,8.20670298643533,-13.513607214262));
#46928=CARTESIAN_POINT('Ctrl Pts',(6.14408270715969,8.19942776684858,-13.4816836950382));
#46929=CARTESIAN_POINT('Ctrl Pts',(6.1399169029108,8.19355261195391,-13.4490613933326));
#46930=CARTESIAN_POINT('Ctrl Pts',(6.13639279479276,8.18918575798983,-13.4159640037694));
#46931=CARTESIAN_POINT('Ctrl Pts',(6.13288938116379,8.18484454733992,-13.3830609707763));
#46932=CARTESIAN_POINT('Ctrl Pts',(6.13002036913961,8.18199439530407,-13.3496891324172));
#46933=CARTESIAN_POINT('Ctrl Pts',(6.12782632623896,8.18070050838779,-13.3160936799609));
#46934=CARTESIAN_POINT('Ctrl Pts',(6.12563972821355,8.17941101191741,-13.282612224342));
#46935=CARTESIAN_POINT('Ctrl Pts',(6.12412366519578,8.17966746091332,-13.2489094999238));
#46936=CARTESIAN_POINT('Ctrl Pts',(6.12329875486801,8.18148856024423,-13.2152419051193));
#46937=CARTESIAN_POINT('Ctrl Pts',(6.122474587247,8.18330801995111,-13.1816046228829));
#46938=CARTESIAN_POINT('Ctrl Pts',(6.12234037294115,8.18668931913289,-13.1480032828271));
#46939=CARTESIAN_POINT('Ctrl Pts',(6.12289574278324,8.19160351827314,-13.1146944380087));
#46940=CARTESIAN_POINT('Ctrl Pts',(6.12345381872746,8.19654166240232,-13.0812232920913));
#46941=CARTESIAN_POINT('Ctrl Pts',(6.12470817202044,8.20302748811596,-13.0480483652075));
#46942=CARTESIAN_POINT('Ctrl Pts',(6.12663723832506,8.21098489540582,-13.0154176313383));
#46943=CARTESIAN_POINT('Ctrl Pts',(6.12857376793279,8.218973088855,-12.9826606534633));
#46944=CARTESIAN_POINT('Ctrl Pts',(6.13119008983231,8.22844384478804,-12.9504528531314));
#46945=CARTESIAN_POINT('Ctrl Pts',(6.13444456932835,8.239277915888,-12.9190202913252));
#46946=CARTESIAN_POINT('Ctrl Pts',(6.1377364432029,8.25023647182683,-12.8872265654326));
#46947=CARTESIAN_POINT('Ctrl Pts',(6.14168100076899,8.26258927480383,-12.8562266434431));
#46948=CARTESIAN_POINT('Ctrl Pts',(6.14621773612586,8.27617735011607,-12.8262182957706));
#46949=CARTESIAN_POINT('Ctrl Pts',(6.14952201341343,8.28607406330389,-12.8043620723299));
#46950=CARTESIAN_POINT('Ctrl Pts',(6.15314003900114,8.29662526281776,-12.7830310876382));
#46951=CARTESIAN_POINT('Ctrl Pts',(6.15704389852412,8.30776080160357,-12.7622874067421));
#46952=CARTESIAN_POINT('Ctrl Pts',(6.16249948673207,8.32332255881625,-12.7332984074658));
#46953=CARTESIAN_POINT('Ctrl Pts',(6.1685132782615,8.34002577189179,-12.7054585112995));
#46954=CARTESIAN_POINT('Ctrl Pts',(6.17499976480806,8.35766462314905,-12.6788945748029));
#46955=CARTESIAN_POINT('Ctrl Pts',(6.18163464544893,8.37570700586176,-12.6517229239035));
#46956=CARTESIAN_POINT('Ctrl Pts',(6.18876374432969,8.3947275157599,-12.6258863743513));
#46957=CARTESIAN_POINT('Ctrl Pts',(6.19628989507741,8.41449938873199,-12.6014667977307));
#46958=CARTESIAN_POINT('Ctrl Pts',(6.20392753003438,8.43456414071986,-12.5766854960689));
#46959=CARTESIAN_POINT('Ctrl Pts',(6.21197371279697,8.45540190412297,-12.5533632206732));
#46960=CARTESIAN_POINT('Ctrl Pts',(6.22032660104379,8.47678133667707,-12.5315318672047));
#46961=CARTESIAN_POINT('Ctrl Pts',(6.22887982626834,8.49867353688436,-12.5091769071411));
#46962=CARTESIAN_POINT('Ctrl Pts',(6.23775431758807,8.52113300253076,-12.4883848497663));
#46963=CARTESIAN_POINT('Ctrl Pts',(6.24684570637579,8.54392866164999,-12.46913883099));
#46964=CARTESIAN_POINT('Ctrl Pts',(6.24787632883521,8.54651283430105,-12.4669570544024));
#46965=CARTESIAN_POINT('Ctrl Pts',(6.24890974675756,8.54910135151727,-12.464795097349));
#46966=CARTESIAN_POINT('Ctrl Pts',(6.24994581473478,8.55169389599726,-12.4626528990853));
#46967=CARTESIAN_POINT('',(7.0000000055496,8.04447578018918,-12.5220651288373));
#46968=CARTESIAN_POINT('Ctrl Pts',(7.00000001330434,8.0444754912143,-12.5220639333861));
#46969=CARTESIAN_POINT('Ctrl Pts',(6.96230391367629,8.08169105625708,-12.5128233328542));
#46970=CARTESIAN_POINT('Ctrl Pts',(6.92358275821775,8.11749582950849,-12.5046001520993));
#46971=CARTESIAN_POINT('Ctrl Pts',(6.88384360033652,8.15194944871618,-12.4973741501251));
#46972=CARTESIAN_POINT('Ctrl Pts',(6.87536872889752,8.1592971130594,-12.4958331150098));
#46973=CARTESIAN_POINT('Ctrl Pts',(6.86684740727857,8.16658324491893,-12.494337512666));
#46974=CARTESIAN_POINT('Ctrl Pts',(6.85827946666746,8.17380828443588,-12.4928872796855));
#46975=CARTESIAN_POINT('Ctrl Pts',(6.82975275306883,8.19786384718938,-12.4880587703898));
#46976=CARTESIAN_POINT('Ctrl Pts',(6.80070995695535,8.22124272875811,-12.4837327177821));
#46977=CARTESIAN_POINT('Ctrl Pts',(6.77114945909981,8.24395849804649,-12.4799068065204));
#46978=CARTESIAN_POINT('Ctrl Pts',(6.70392153480423,8.29561980718607,-12.4712057327456));
#46979=CARTESIAN_POINT('Ctrl Pts',(6.63401832348786,8.343863738285,-12.4650822521963));
#46980=CARTESIAN_POINT('Ctrl Pts',(6.56187334522743,8.38842090408476,-12.4616052237448));
#46981=CARTESIAN_POINT('Ctrl Pts',(6.54809121393698,8.39693282998439,-12.4609409936934));
#46982=CARTESIAN_POINT('Ctrl Pts',(6.53422713052313,8.40531018090756,-12.4603733932308));
#46983=CARTESIAN_POINT('Ctrl Pts',(6.52028392429325,8.41355102861473,-12.4599029761146));
#46984=CARTESIAN_POINT('Ctrl Pts',(6.4919859927506,8.43027594399118,-12.4589482580154));
#46985=CARTESIAN_POINT('Ctrl Pts',(6.46336436275962,8.44643567541406,-12.4583951007039));
#46986=CARTESIAN_POINT('Ctrl Pts',(6.43440475968353,8.4620318338438,-12.4582494770983));
#46987=CARTESIAN_POINT('Ctrl Pts',(6.38955372914157,8.48618630088645,-12.4580239433172));
#46988=CARTESIAN_POINT('Ctrl Pts',(6.34389273458103,8.50899103300897,-12.4587745664364));
#46989=CARTESIAN_POINT('Ctrl Pts',(6.29738181090352,8.53043175235834,-12.4605287526016));
#46990=CARTESIAN_POINT('Ctrl Pts',(6.28166761543794,8.53767572061652,-12.4611214224972));
#46991=CARTESIAN_POINT('Ctrl Pts',(6.26585625737833,8.54476364661387,-12.4618288799934));
#46992=CARTESIAN_POINT('Ctrl Pts',(6.24994581473509,8.55169389599713,-12.4626528990853));
#46993=CARTESIAN_POINT('',(7.,6.97709641029578,-13.9487350316508));
#46994=CARTESIAN_POINT('Ctrl Pts',(7.,6.97709641029578,-13.9487350316508));
#46995=CARTESIAN_POINT('Ctrl Pts',(7.,7.03293718041427,-13.8193396715212));
#46996=CARTESIAN_POINT('Ctrl Pts',(7.,7.08905635229391,-13.6999263902358));
#46997=CARTESIAN_POINT('Ctrl Pts',(7.,7.14545392593474,-13.5904951877945));
#46998=CARTESIAN_POINT('Ctrl Pts',(7.,7.16425311714834,-13.554018120314));
#46999=CARTESIAN_POINT('Ctrl Pts',(7.,7.18201591735578,-13.5205888384398));
#47000=CARTESIAN_POINT('Ctrl Pts',(7.,7.20194430016261,-13.4843913449679));
#47001=CARTESIAN_POINT('Ctrl Pts',(7.,7.28165783138991,-13.3396013710801));
#47002=CARTESIAN_POINT('Ctrl Pts',(7.,7.36741849085433,-13.2055562149066));
#47003=CARTESIAN_POINT('Ctrl Pts',(7.,7.45610471591587,-13.0864482193812));
#47004=CARTESIAN_POINT('Ctrl Pts',(7.,7.63347716603895,-12.8482322283304));
#47005=CARTESIAN_POINT('Ctrl Pts',(7.,7.82960075808121,-12.6601046255877));
#47006=CARTESIAN_POINT('Ctrl Pts',(7.,8.04447549204264,-12.5220654111529));
#47007=CARTESIAN_POINT('Ctrl Pts',(6.99999409973866,6.97709640977505,-13.9487350319038));
#47008=CARTESIAN_POINT('Ctrl Pts',(6.99998773340224,7.02238008649688,-13.9417617463364));
#47009=CARTESIAN_POINT('Ctrl Pts',(6.99825780681655,7.0667383458091,-13.9353109212988));
#47010=CARTESIAN_POINT('Ctrl Pts',(6.99506629168637,7.1100004802052,-13.929375924186));
#47011=CARTESIAN_POINT('Ctrl Pts',(6.99192032954138,7.15264512751851,-13.9235256381978));
#47012=CARTESIAN_POINT('Ctrl Pts',(6.98735349753255,7.19422506924278,-13.9181766158872));
#47013=CARTESIAN_POINT('Ctrl Pts',(6.98158514077008,7.23461460637864,-13.9133177410806));
#47014=CARTESIAN_POINT('Ctrl Pts',(6.97530695511168,7.27857392152467,-13.9080294207871));
#47015=CARTESIAN_POINT('Ctrl Pts',(6.9676065761953,7.32112357876287,-13.9033213294894));
#47016=CARTESIAN_POINT('Ctrl Pts',(6.95878220379846,7.36217508309488,-13.8991509038545));
#47017=CARTESIAN_POINT('Ctrl Pts',(6.95175715564054,7.39485602423362,-13.8958308444094));
#47018=CARTESIAN_POINT('Ctrl Pts',(6.94401872090156,7.42658826306636,-13.8928515284589));
#47019=CARTESIAN_POINT('Ctrl Pts',(6.93569970011813,7.45734250331633,-13.8901905229079));
#47020=CARTESIAN_POINT('Ctrl Pts',(6.92545249237511,7.49522497735077,-13.8869127481077));
#47021=CARTESIAN_POINT('Ctrl Pts',(6.91432486971307,7.53162294634188,-13.8841180209678));
#47022=CARTESIAN_POINT('Ctrl Pts',(6.90253856527727,7.56650707684142,-13.8817619962387));
#47023=CARTESIAN_POINT('Ctrl Pts',(6.88931061744749,7.60565806440064,-13.8791177940316));
#47024=CARTESIAN_POINT('Ctrl Pts',(6.87525432449622,7.64290263392926,-13.8770257005009));
#47025=CARTESIAN_POINT('Ctrl Pts',(6.86067610400931,7.67825570504179,-13.8754032193005));
#47026=CARTESIAN_POINT('Ctrl Pts',(6.85201223617144,7.69926611135696,-13.8744389752282));
#47027=CARTESIAN_POINT('Ctrl Pts',(6.84316308205284,7.71960899951211,-13.8736406359784));
#47028=CARTESIAN_POINT('Ctrl Pts',(6.83418557292495,7.73929185965251,-13.8729911263498));
#47029=CARTESIAN_POINT('Ctrl Pts',(6.82792838530364,7.75301051446733,-13.8725384279956));
#47030=CARTESIAN_POINT('Ctrl Pts',(6.82160873308596,7.76640860216193,-13.8721580324725));
#47031=CARTESIAN_POINT('Ctrl Pts',(6.81524449342781,7.77948949420881,-13.8718441865394));
#47032=CARTESIAN_POINT('Ctrl Pts',(6.81206237359873,7.78602994023225,-13.8716872635729));
#47033=CARTESIAN_POINT('Ctrl Pts',(6.80886909868809,7.7924910834006,-13.871546982403));
#47034=CARTESIAN_POINT('Ctrl Pts',(6.8056667930717,7.79887342071668,-13.8714226207036));
#47035=CARTESIAN_POINT('Ctrl Pts',(6.80406564026351,7.80206458937472,-13.8713604398539));
#47036=CARTESIAN_POINT('Ctrl Pts',(6.80246222927231,7.80523605633618,-13.871302239133));
#47037=CARTESIAN_POINT('Ctrl Pts',(6.80085682107126,7.80838788492505,-13.8712479289958));
#47038=CARTESIAN_POINT('Ctrl Pts',(6.7994724279675,7.8111058041183,-13.8712010956861));
#47039=CARTESIAN_POINT('Ctrl Pts',(6.79847729449419,7.81305026698218,-13.8711691335029));
#47040=CARTESIAN_POINT('Ctrl Pts',(6.79686095399513,7.81618460023036,-13.8711208812908));
#47041=CARTESIAN_POINT('Ctrl Pts',(6.79660290904266,7.81668498914875,-13.8711131779388));
#47042=CARTESIAN_POINT('Ctrl Pts',(6.79632895166726,7.81721565513594,-13.8711051012948));
#47043=CARTESIAN_POINT('Ctrl Pts',(6.7960348629784,7.8177845195718,-13.8710965813229));
#47044=CARTESIAN_POINT('Ctrl Pts',(6.78633377486737,7.83654962079648,-13.8708155334567));
#47045=CARTESIAN_POINT('Ctrl Pts',(6.77635283842971,7.85503260700263,-13.8706755538496));
#47046=CARTESIAN_POINT('Ctrl Pts',(6.76610585975263,7.87322195488204,-13.8706790001011));
#47047=CARTESIAN_POINT('Ctrl Pts',(6.73511960207716,7.92822546743936,-13.870689421362));
#47048=CARTESIAN_POINT('Ctrl Pts',(6.70170471002237,7.98054310553255,-13.8720098209944));
#47049=CARTESIAN_POINT('Ctrl Pts',(6.66632523798378,8.02995177089685,-13.8746434658222));
#47050=CARTESIAN_POINT('Ctrl Pts',(6.63916138333988,8.0678870403277,-13.8766655408042));
#47051=CARTESIAN_POINT('Ctrl Pts',(6.61083810974908,8.1041076340751,-13.8794623048069));
#47052=CARTESIAN_POINT('Ctrl Pts',(6.58154671953346,8.13851818864679,-13.8830415512864));
#47053=CARTESIAN_POINT('Ctrl Pts',(6.54179775503399,8.18521395494564,-13.8878986557189));
#47054=CARTESIAN_POINT('Ctrl Pts',(6.5002682591157,8.22857660783537,-13.8941957405529));
#47055=CARTESIAN_POINT('Ctrl Pts',(6.45749341303235,8.26847853134568,-13.9018834005547));
#47056=CARTESIAN_POINT('Ctrl Pts',(6.42567623290322,8.29815874773624,-13.9076017066492));
#47057=CARTESIAN_POINT('Ctrl Pts',(6.39316882688615,8.32592430382819,-13.9140899065749));
#47058=CARTESIAN_POINT('Ctrl Pts',(6.36017433818513,8.35172762350273,-13.9213326680527));
#47059=CARTESIAN_POINT('Ctrl Pts',(6.3284535697521,8.37653483102203,-13.9282958297412));
#47060=CARTESIAN_POINT('Ctrl Pts',(6.29628264519726,8.39952869941061,-13.9359562792266));
#47061=CARTESIAN_POINT('Ctrl Pts',(6.2638568752866,8.42071068616162,-13.9442728359254));
#47062=CARTESIAN_POINT('Ctrl Pts',(6.99927529182611,10.8726415770594,-24.2327789237978));
#47063=CARTESIAN_POINT('Ctrl Pts',(6.99927529182611,10.8786673784413,-24.195315187381));
#47064=CARTESIAN_POINT('Ctrl Pts',(6.99927529182611,10.9735995203797,-23.5849660827267));
#47065=CARTESIAN_POINT('Ctrl Pts',(6.99927529182611,11.0582112387948,-22.3847865482758));
#47066=CARTESIAN_POINT('Ctrl Pts',(6.99927529182611,10.903047790836,-20.6453395628878));
#47067=CARTESIAN_POINT('Ctrl Pts',(6.99927529182611,10.4741299264985,-18.9496408568389));
#47068=CARTESIAN_POINT('Ctrl Pts',(6.99927529182611,9.78081713300028,-17.3432623946008));
#47069=CARTESIAN_POINT('Ctrl Pts',(6.99927529182611,8.84300079934772,-15.8679928669231));
#47070=CARTESIAN_POINT('Ctrl Pts',(6.99927529182611,7.83768636590236,-14.7356908281778));
#47071=CARTESIAN_POINT('Ctrl Pts',(6.99927529182611,7.13749347049657,-14.123730174869));
#47072=CARTESIAN_POINT('Ctrl Pts',(6.99927529182611,6.86420636501945,-13.9070393690543));
#47073=CARTESIAN_POINT('Ctrl Pts',(7.017832597561,11.3536240592414,-24.3101961947595));
#47074=CARTESIAN_POINT('Ctrl Pts',(7.017832597561,11.3599171239206,-24.2710685142874));
#47075=CARTESIAN_POINT('Ctrl Pts',(7.017832597561,11.4590599350526,-23.6336238827185));
#47076=CARTESIAN_POINT('Ctrl Pts',(7.017832597561,11.5474272379709,-22.3805204832481));
#47077=CARTESIAN_POINT('Ctrl Pts',(7.017832597561,11.3853285909672,-20.5631123377262));
#47078=CARTESIAN_POINT('Ctrl Pts',(7.017832597561,10.9373786509483,-18.7923604165634));
#47079=CARTESIAN_POINT('Ctrl Pts',(7.017832597561,10.2132342895059,-17.1143873744336));
#47080=CARTESIAN_POINT('Ctrl Pts',(7.017832597561,9.23354352116467,-15.5733329492476));
#47081=CARTESIAN_POINT('Ctrl Pts',(7.017832597561,8.18359794548622,-14.390762581988));
#47082=CARTESIAN_POINT('Ctrl Pts',(7.017832597561,7.45236474088215,-13.751653467176));
#47083=CARTESIAN_POINT('Ctrl Pts',(7.017832597561,7.1668757223976,-13.5252911594398));
#47084=CARTESIAN_POINT('Ctrl Pts',(6.72802461549766,11.741859342275,-24.3726851984411));
#47085=CARTESIAN_POINT('Ctrl Pts',(6.72802461549766,11.7483681342363,-24.3322144299968));
#47086=CARTESIAN_POINT('Ctrl Pts',(6.72802461549766,11.8509096769365,-23.6728990651836));
#47087=CARTESIAN_POINT('Ctrl Pts',(6.72802461549766,11.9423083800943,-22.377077037741));
#47088=CARTESIAN_POINT('Ctrl Pts',(6.72802461549766,11.7746118390656,-20.4967408767737));
#47089=CARTESIAN_POINT('Ctrl Pts',(6.72802461549766,11.3112997526846,-18.6654081500895));
#47090=CARTESIAN_POINT('Ctrl Pts',(6.72802461549766,10.5622690326939,-16.9296460137264));
#47091=CARTESIAN_POINT('Ctrl Pts',(6.72802461549766,9.54877842006116,-15.3354919035144));
#47092=CARTESIAN_POINT('Ctrl Pts',(6.72802461549766,8.46280786472511,-14.1123463812967));
#47093=CARTESIAN_POINT('Ctrl Pts',(6.72802461549766,7.70651981161201,-13.4513238059636));
#47094=CARTESIAN_POINT('Ctrl Pts',(6.72802461549766,7.41118175844214,-13.2171549388937));
#47095=CARTESIAN_POINT('Ctrl Pts',(6.2547269417983,11.8649496891146,-24.3924973934525));
#47096=CARTESIAN_POINT('Ctrl Pts',(6.2547269417983,11.8715268776038,-24.3516007977501));
#47097=CARTESIAN_POINT('Ctrl Pts',(6.2547269417983,11.9751459912159,-23.6853512972297));
#47098=CARTESIAN_POINT('Ctrl Pts',(6.2547269417983,12.0675058025525,-22.375985290233));
#47099=CARTESIAN_POINT('Ctrl Pts',(6.2547269417983,11.8980344441738,-20.4756977451863));
#47100=CARTESIAN_POINT('Ctrl Pts',(6.2547269417983,11.429851775427,-18.6251578194452));
#47101=CARTESIAN_POINT('Ctrl Pts',(6.2547269417983,10.6729308129992,-16.8710735986019));
#47102=CARTESIAN_POINT('Ctrl Pts',(6.2547269417983,9.64872392923276,-15.2600841853353));
#47103=CARTESIAN_POINT('Ctrl Pts',(6.2547269417983,8.55133162158488,-14.024074273618));
#47104=CARTESIAN_POINT('Ctrl Pts',(6.2547269417983,7.78709990614218,-13.3561040158518));
#47105=CARTESIAN_POINT('Ctrl Pts',(6.2547269417983,7.48863920763838,-13.1194600721039));
#47106=CARTESIAN_POINT('',(7.00000000000001,10.9277801898197,-24.1259420764688));
#47107=CARTESIAN_POINT('Ctrl Pts',(7.00000000000005,10.9277802009506,-24.1259420781411));
#47108=CARTESIAN_POINT('Ctrl Pts',(7.00000000000005,10.9521693515102,-23.9636096893172));
#47109=CARTESIAN_POINT('Ctrl Pts',(7.00000000006095,10.9728901444114,-23.801252032564));
#47110=CARTESIAN_POINT('Ctrl Pts',(6.99999999867112,10.9899908760259,-23.6387724641683));
#47111=CARTESIAN_POINT('Ctrl Pts',(6.99999999727843,11.0071267182727,-23.4759592983278));
#47112=CARTESIAN_POINT('Ctrl Pts',(6.99999999421914,11.0206276373359,-23.3130232621382));
#47113=CARTESIAN_POINT('Ctrl Pts',(6.99999999313357,11.0304902733626,-23.149860765446));
#47114=CARTESIAN_POINT('Ctrl Pts',(6.99999999205182,11.0403181946778,-22.9872725715058));
#47115=CARTESIAN_POINT('Ctrl Pts',(6.99999999470457,11.0465333999261,-22.8244590565224));
#47116=CARTESIAN_POINT('Ctrl Pts',(6.99999999802627,11.0490809628184,-22.6613182277958));
#47117=CARTESIAN_POINT('Ctrl Pts',(6.99999999906757,11.04987958869,-22.6101758254147));
#47118=CARTESIAN_POINT('Ctrl Pts',(7.00000000000005,11.0503173996174,-22.5590012875906));
#47119=CARTESIAN_POINT('Ctrl Pts',(7.00000000000005,11.0503916515239,-22.507791591419));
#47120=CARTESIAN_POINT('Ctrl Pts',(7.00000000000005,11.0504508814845,-22.4669421583217));
#47121=CARTESIAN_POINT('Ctrl Pts',(6.99999999938506,11.0502838028415,-22.426069923528));
#47122=CARTESIAN_POINT('Ctrl Pts',(6.99999999847366,11.0498891594648,-22.3851800824517));
#47123=CARTESIAN_POINT('Ctrl Pts',(6.99999999415778,11.0480203461542,-22.1915483537147));
#47124=CARTESIAN_POINT('Ctrl Pts',(6.99999998570413,11.0410443720245,-21.9975213270894));
#47125=CARTESIAN_POINT('Ctrl Pts',(6.99999998494295,11.0289325037734,-21.8035929264893));
#47126=CARTESIAN_POINT('Ctrl Pts',(6.99999998418016,11.016795034324,-21.6092546139492));
#47127=CARTESIAN_POINT('Ctrl Pts',(6.99999998976666,10.9994999282979,-21.4150157630175));
#47128=CARTESIAN_POINT('Ctrl Pts',(6.99999999468265,10.9770705166507,-21.2213760732062));
#47129=CARTESIAN_POINT('Ctrl Pts',(6.99999999757253,10.9638852767666,-21.1075440297526));
#47130=CARTESIAN_POINT('Ctrl Pts',(7.00000000000005,10.9489267433494,-20.9939190591194));
#47131=CARTESIAN_POINT('Ctrl Pts',(7.00000000000005,10.932208049831,-20.8806022008953));
#47132=CARTESIAN_POINT('Ctrl Pts',(7.00000000000005,10.9207197174214,-20.8027359649097));
#47133=CARTESIAN_POINT('Ctrl Pts',(6.99999999889749,10.9083941647938,-20.7250167855243));
#47134=CARTESIAN_POINT('Ctrl Pts',(6.99999999756676,10.8952339987249,-20.647455114461));
#47135=CARTESIAN_POINT('Ctrl Pts',(6.99999999341047,10.8541305337291,-20.4052048711987));
#47136=CARTESIAN_POINT('Ctrl Pts',(6.99999998911108,10.8048891706622,-20.1644906605692));
#47137=CARTESIAN_POINT('Ctrl Pts',(6.99999999137289,10.7476171238347,-19.9256794472572));
#47138=CARTESIAN_POINT('Ctrl Pts',(6.99999999340022,10.6962822476428,-19.711624864826));
#47139=CARTESIAN_POINT('Ctrl Pts',(7.00000000000005,10.6384946505734,-19.499098911231));
#47140=CARTESIAN_POINT('Ctrl Pts',(7.00000000000005,10.5742967747319,-19.2883734681814));
#47141=CARTESIAN_POINT('Ctrl Pts',(7.00000000000005,10.5400974275295,-19.176116286822));
#47142=CARTESIAN_POINT('Ctrl Pts',(6.99999999798936,10.504093508003,-19.0643633763299));
#47143=CARTESIAN_POINT('Ctrl Pts',(6.99999999626517,10.4662999237067,-18.9531935123782));
#47144=CARTESIAN_POINT('Ctrl Pts',(6.99999999250277,10.3838292711404,-18.7106060098555));
#47145=CARTESIAN_POINT('Ctrl Pts',(6.99999999167269,10.2928334595614,-18.4707958679957));
#47146=CARTESIAN_POINT('Ctrl Pts',(6.99999999476598,10.1936291084844,-18.234499293281));
#47147=CARTESIAN_POINT('Ctrl Pts',(6.99999999683537,10.1272621312739,-18.0764186323145));
#47148=CARTESIAN_POINT('Ctrl Pts',(7.00000000000005,10.0572224760596,-17.9199102275781));
#47149=CARTESIAN_POINT('Ctrl Pts',(7.00000000000005,9.98361708049291,-17.765189800066));
#47150=CARTESIAN_POINT('Ctrl Pts',(7.00000000000005,9.91648607953027,-17.6240787159086));
#47151=CARTESIAN_POINT('Ctrl Pts',(6.99999999705136,9.84637810930485,-17.4844629690789));
#47152=CARTESIAN_POINT('Ctrl Pts',(6.99999999409833,9.77333028856548,-17.3464250463554));
#47153=CARTESIAN_POINT('Ctrl Pts',(6.99999998947413,9.65894344405889,-17.1302690783503));
#47154=CARTESIAN_POINT('Ctrl Pts',(6.99999998692745,9.53734971276868,-16.9179803553399));
#47155=CARTESIAN_POINT('Ctrl Pts',(6.99999999182225,9.40869665247457,-16.7098917675291));
#47156=CARTESIAN_POINT('Ctrl Pts',(6.99999999469974,9.33306577083223,-16.5875633649255));
#47157=CARTESIAN_POINT('Ctrl Pts',(7.00000000000005,9.25499448752809,-16.4666870596751));
#47158=CARTESIAN_POINT('Ctrl Pts',(7.00000000000005,9.17450657072659,-16.3473361667542));
#47159=CARTESIAN_POINT('Ctrl Pts',(7.00000000000005,9.06569816815992,-16.1859904577374));
#47160=CARTESIAN_POINT('Ctrl Pts',(6.99999998960196,8.95252125830182,-16.027385824795));
#47161=CARTESIAN_POINT('Ctrl Pts',(6.99999998461871,8.83522853413698,-15.8719380527288));
#47162=CARTESIAN_POINT('Ctrl Pts',(6.99999997943771,8.71328140858451,-15.7103218134268));
#47163=CARTESIAN_POINT('Ctrl Pts',(6.99999998080586,8.58688537844239,-15.5521184867226));
#47164=CARTESIAN_POINT('Ctrl Pts',(6.99999998755719,8.45642472370038,-15.3977016699108));
#47165=CARTESIAN_POINT('Ctrl Pts',(6.99999999250482,8.36081825447468,-15.284539225083));
#47166=CARTESIAN_POINT('Ctrl Pts',(7.00000000000005,8.26302974978129,-15.1734096595939));
#47167=CARTESIAN_POINT('Ctrl Pts',(7.00000000000005,8.16322280872337,-15.0644472405567));
#47168=CARTESIAN_POINT('Ctrl Pts',(7.00000000000005,8.05103332172495,-14.9419664014054));
#47169=CARTESIAN_POINT('Ctrl Pts',(6.99999999328023,7.93625106258992,-14.8222864757151));
#47170=CARTESIAN_POINT('Ctrl Pts',(6.99999999271608,7.81883217509785,-14.7052852661705));
#47171=CARTESIAN_POINT('Ctrl Pts',(6.9999999924934,7.77248661607701,-14.6591045657885));
#47172=CARTESIAN_POINT('Ctrl Pts',(6.99999999280614,7.72572983592215,-14.6133415237277));
#47173=CARTESIAN_POINT('Ctrl Pts',(6.99999999341965,7.6785573913367,-14.5679900171479));
#47174=CARTESIAN_POINT('Ctrl Pts',(6.99999999496859,7.55946070981941,-14.4534906736664));
#47175=CARTESIAN_POINT('Ctrl Pts',(6.99999999795298,7.43771702120765,-14.3416119007437));
#47176=CARTESIAN_POINT('Ctrl Pts',(6.99999999909583,7.3132546940743,-14.2323043265284));
#47177=CARTESIAN_POINT('Ctrl Pts',(7.00000000010504,7.20334631839466,-14.1357785889161));
#47178=CARTESIAN_POINT('Ctrl Pts',(6.99999999999947,7.09131727001927,-14.0412582116215));
#47179=CARTESIAN_POINT('Ctrl Pts',(6.99999999999947,6.97709641029447,-13.9487350316524));
#47180=CARTESIAN_POINT('',(6.27159471697239,11.8794981306056,-24.2690139179354));
#47181=CARTESIAN_POINT('Origin',(5.999999877385,10.9277801432447,-24.1259420367213));
#47182=CARTESIAN_POINT('Ctrl Pts',(6.27159470456933,11.8794980693479,-24.2690136413586));
#47183=CARTESIAN_POINT('Ctrl Pts',(6.27193966899897,11.91387827254,-24.0395181149413));
#47184=CARTESIAN_POINT('Ctrl Pts',(6.2722578256641,11.9412741933855,-23.8113319282651));
#47185=CARTESIAN_POINT('Ctrl Pts',(6.27254917027625,11.9620370246289,-23.5849163959185));
#47186=CARTESIAN_POINT('Ctrl Pts',(6.27284515817359,11.9831307621011,-23.3548923812278));
#47187=CARTESIAN_POINT('Ctrl Pts',(6.27311347258153,11.9973783276931,-23.1266958622964));
#47188=CARTESIAN_POINT('Ctrl Pts',(6.27335410993762,12.0051465928033,-22.9007563434725));
#47189=CARTESIAN_POINT('Ctrl Pts',(6.27354178808869,12.0112052266602,-22.7245413457914));
#47190=CARTESIAN_POINT('Ctrl Pts',(6.27371263094733,12.0133226280565,-22.5496981157126));
#47191=CARTESIAN_POINT('Ctrl Pts',(6.27386663718285,12.0116720903008,-22.3764084710348));
#47192=CARTESIAN_POINT('Ctrl Pts',(6.27406868749932,12.0095066476175,-22.1490590560667));
#47193=CARTESIAN_POINT('Ctrl Pts',(6.27424175785168,12.0008569236811,-21.9243852895248));
#47194=CARTESIAN_POINT('Ctrl Pts',(6.27438584598699,11.9862082353842,-21.7027333745298));
#47195=CARTESIAN_POINT('Ctrl Pts',(6.27447251908356,11.9773966342575,-21.5694034664637));
#47196=CARTESIAN_POINT('Ctrl Pts',(6.27454870537683,11.9664140727742,-21.4371659889583));
#47197=CARTESIAN_POINT('Ctrl Pts',(6.27461440451541,11.9533633512297,-21.3060877049261));
#47198=CARTESIAN_POINT('Ctrl Pts',(6.27472591355225,11.9312127809046,-21.0836127453143));
#47199=CARTESIAN_POINT('Ctrl Pts',(6.27480721201525,11.9031053535267,-20.8644797536233));
#47200=CARTESIAN_POINT('Ctrl Pts',(6.27485829884291,11.8695299317154,-20.6489747555412));
#47201=CARTESIAN_POINT('Ctrl Pts',(6.27487121254234,11.8610427555617,-20.5944995238963));
#47202=CARTESIAN_POINT('Ctrl Pts',(6.27488219579953,11.8522061030633,-20.5402558654031));
#47203=CARTESIAN_POINT('Ctrl Pts',(6.27489124860539,11.8430276976174,-20.4862479066156));
#47204=CARTESIAN_POINT('Ctrl Pts',(6.27492812667111,11.8056379817079,-20.2662377700162));
#47205=CARTESIAN_POINT('Ctrl Pts',(6.27493296937425,11.7625789016338,-20.0501427398753));
#47206=CARTESIAN_POINT('Ctrl Pts',(6.27490577664845,11.7143943118651,-19.8381869763113));
#47207=CARTESIAN_POINT('Ctrl Pts',(6.27488257757199,11.6732863335747,-19.6573600154728));
#47208=CARTESIAN_POINT('Ctrl Pts',(6.27483606184378,11.6284473802591,-19.4795448890848));
#47209=CARTESIAN_POINT('Ctrl Pts',(6.27476622992978,11.5802014285004,-19.3048541862108));
#47210=CARTESIAN_POINT('Ctrl Pts',(6.27472435194866,11.551268481639,-19.200092716301));
#47211=CARTESIAN_POINT('Ctrl Pts',(6.2746740886978,11.5211100139789,-19.0964544409574));
#47212=CARTESIAN_POINT('Ctrl Pts',(6.27461544169057,11.489793764837,-18.9939596243062));
#47213=CARTESIAN_POINT('Ctrl Pts',(6.27458611818695,11.474135640266,-18.9427122159807));
#47214=CARTESIAN_POINT('Ctrl Pts',(6.27455469611227,11.458188061523,-18.8917506750642));
#47215=CARTESIAN_POINT('Ctrl Pts',(6.2745211789115,11.4419593308387,-18.8410772071659));
#47216=CARTESIAN_POINT('Ctrl Pts',(6.27450442031112,11.4338449654966,-18.8157404732167));
#47217=CARTESIAN_POINT('Ctrl Pts',(6.27448713775144,11.4256603115726,-18.7904757576991));
#47218=CARTESIAN_POINT('Ctrl Pts',(6.27446933123306,11.4174064002052,-18.7652833275414));
#47219=CARTESIAN_POINT('Ctrl Pts',(6.27445391940419,11.4102625067896,-18.7434788729119));
#47220=CARTESIAN_POINT('Ctrl Pts',(6.27443872975055,11.403338950616,-18.7225457109356));
#47221=CARTESIAN_POINT('Ctrl Pts',(6.27442216602411,11.395929825651,-18.7003621758541));
#47222=CARTESIAN_POINT('Ctrl Pts',(6.27441959235278,11.3947785960287,-18.6969152988161));
#47223=CARTESIAN_POINT('Ctrl Pts',(6.27441698550732,11.3936155468417,-18.6934382660929));
#47224=CARTESIAN_POINT('Ctrl Pts',(6.27441433949973,11.3924379209365,-18.689923155043));
#47225=CARTESIAN_POINT('Ctrl Pts',(6.27440279752698,11.3873010777388,-18.6745901242335));
#47226=CARTESIAN_POINT('Ctrl Pts',(6.27439106572956,11.3821298476611,-18.6592579804075));
#47227=CARTESIAN_POINT('Ctrl Pts',(6.27437914410846,11.3769241436459,-18.643926888831));
#47228=CARTESIAN_POINT('Ctrl Pts',(6.27420011134086,11.2987475610068,-18.4136924490583));
#47229=CARTESIAN_POINT('Ctrl Pts',(6.27397826846476,11.2127950847352,-18.1836912011832));
#47230=CARTESIAN_POINT('Ctrl Pts',(6.27371361975783,11.1188688560928,-17.9544927346738));
#47231=CARTESIAN_POINT('Ctrl Pts',(6.27345239300995,11.0261571117798,-17.728257848731));
#47232=CARTESIAN_POINT('Ctrl Pts',(6.27314946023938,10.9256764527698,-17.5028050812689));
#47233=CARTESIAN_POINT('Ctrl Pts',(6.27280482739841,10.8172505232637,-17.2787308995921));
#47234=CARTESIAN_POINT('Ctrl Pts',(6.27260798345405,10.7553208836645,-17.1507464462612));
#47235=CARTESIAN_POINT('Ctrl Pts',(6.272397535514,10.6907994758282,-17.0232126335942));
#47236=CARTESIAN_POINT('Ctrl Pts',(6.27217348498568,10.6236555852736,-16.8962479574695));
#47237=CARTESIAN_POINT('Ctrl Pts',(6.27177013698152,10.5027794844665,-16.6676792096146));
#47238=CARTESIAN_POINT('Ctrl Pts',(6.27132270396134,10.3734026228786,-16.4409516713369));
#47239=CARTESIAN_POINT('Ctrl Pts',(6.27083119612744,10.2354142164086,-16.2167887268486));
#47240=CARTESIAN_POINT('Ctrl Pts',(6.27036732554269,10.1051848316808,-16.0052303569369));
#47241=CARTESIAN_POINT('Ctrl Pts',(6.26986419868896,9.9672852585331,-15.7959566509888));
#47242=CARTESIAN_POINT('Ctrl Pts',(6.26932182550144,9.82164211896925,-15.5896237836272));
#47243=CARTESIAN_POINT('Ctrl Pts',(6.26905884966486,9.75102537877976,-15.4895809355352));
#47244=CARTESIAN_POINT('Ctrl Pts',(6.26878664742083,9.67858849328747,-15.3902301631767));
#47245=CARTESIAN_POINT('Ctrl Pts',(6.26850522012318,9.60432480000494,-15.2916503518621));
#47246=CARTESIAN_POINT('Ctrl Pts',(6.26791729758894,9.44918242710482,-15.0857098017579));
#47247=CARTESIAN_POINT('Ctrl Pts',(6.26728911457511,9.28606521508869,-14.8831314821586));
#47248=CARTESIAN_POINT('Ctrl Pts',(6.26662068570985,9.11502603156112,-14.6845483878654));
#47249=CARTESIAN_POINT('Ctrl Pts',(6.2659595690909,8.94585792318419,-14.4881376840467));
#47250=CARTESIAN_POINT('Ctrl Pts',(6.26525908231365,8.76894017634307,-14.2956352473713));
#47251=CARTESIAN_POINT('Ctrl Pts',(6.26451924289097,8.5843553372276,-14.107693790117));
#47252=CARTESIAN_POINT('Ctrl Pts',(6.26430323665952,8.53046327057285,-14.0528217129189));
#47253=CARTESIAN_POINT('Ctrl Pts',(6.26408387592249,8.47591784790006,-13.998338691807));
#47254=CARTESIAN_POINT('Ctrl Pts',(6.26386116117568,8.42072164460613,-13.9442616338722));
#47255=CARTESIAN_POINT('Ctrl Pts',(6.99999999998951,9.33248386900998,-24.7867299441529));
#47256=CARTESIAN_POINT('Ctrl Pts',(6.99999999998951,9.33249195738903,-24.7867268023194));
#47257=CARTESIAN_POINT('Ctrl Pts',(6.99999999998951,9.60233986589691,-24.6819075265188));
#47258=CARTESIAN_POINT('Ctrl Pts',(6.99999999998951,10.1365881548997,-24.4674868372888));
#47259=CARTESIAN_POINT('Ctrl Pts',(6.99999999998951,10.6659288230102,-24.2412740855147));
#47260=CARTESIAN_POINT('Ctrl Pts',(6.99999999998951,10.9277807259391,-24.1259369153972));
#47261=CARTESIAN_POINT('Ctrl Pts',(7.00000270566769,9.54650236981204,-25.3377021349734));
#47262=CARTESIAN_POINT('Ctrl Pts',(7.00000270566769,9.54651058119136,-25.3376989453619));
#47263=CARTESIAN_POINT('Ctrl Pts',(7.00000270566769,9.82046207621099,-25.2312856794742));
#47264=CARTESIAN_POINT('Ctrl Pts',(7.00000270566769,10.3628264314847,-25.0136075515436));
#47265=CARTESIAN_POINT('Ctrl Pts',(7.00000270566769,10.9002087461683,-24.783958270892));
#47266=CARTESIAN_POINT('Ctrl Pts',(7.00000270566769,11.1660426386392,-24.6668671648011));
#47267=CARTESIAN_POINT('Ctrl Pts',(6.57967198012589,9.69699923069234,-25.7251433367391));
#47268=CARTESIAN_POINT('Ctrl Pts',(6.57967198012589,9.6970075285649,-25.7251401135304));
#47269=CARTESIAN_POINT('Ctrl Pts',(6.57967198012589,9.97384464742593,-25.6176059608812));
#47270=CARTESIAN_POINT('Ctrl Pts',(6.57967198012589,10.5219161845169,-25.3976372164973));
#47271=CARTESIAN_POINT('Ctrl Pts',(6.57967198012589,11.0649533494165,-25.1655713839739));
#47272=CARTESIAN_POINT('Ctrl Pts',(6.57967198012589,11.3335873592823,-25.0472469178922));
#47273=CARTESIAN_POINT('Ctrl Pts',(5.98852436209119,9.69454278461807,-25.7188194279642));
#47274=CARTESIAN_POINT('Ctrl Pts',(5.98852436209119,9.69455108107884,-25.7188162053039));
#47275=CARTESIAN_POINT('Ctrl Pts',(5.98852436209119,9.9713411000889,-25.611300348033));
#47276=CARTESIAN_POINT('Ctrl Pts',(5.98852436209119,10.519319483182,-25.3913689916453));
#47277=CARTESIAN_POINT('Ctrl Pts',(5.98852436209119,11.062264348252,-25.159342602665));
#47278=CARTESIAN_POINT('Ctrl Pts',(5.98852436209119,11.330852653926,-25.0410382677823));
#47279=CARTESIAN_POINT('',(6.99999999994009,9.33250873275974,-24.7867180661797));
#47280=CARTESIAN_POINT('',(5.98852583803805,9.69456766152529,-25.7188097331007));
#47281=CARTESIAN_POINT('Origin',(5.999999999061,9.33250979146072,-24.7867247845918));
#47282=CARTESIAN_POINT('',(5.98852581751677,11.3308503372889,-25.041038957009));
#47283=CARTESIAN_POINT('Origin',(5.98846864787388,-4.75314843312467,11.4751155009116));
#47284=CARTESIAN_POINT('Origin',(6.,10.9277801936247,-24.1259421517584));
#47285=CARTESIAN_POINT('Origin',(6.9999999787379,-4.74946026808531,11.4664779416658));
#47286=CARTESIAN_POINT('Origin',(5.999999877385,10.9277801432447,-24.1259420367213));
#47287=CARTESIAN_POINT('Origin',(5.99999763275393,10.9277792104516,-24.1259401189103));
#47288=CARTESIAN_POINT('Ctrl Pts',(-6.094431914356,11.2713279469382,-25.06822360013));
#47289=CARTESIAN_POINT('Ctrl Pts',(-6.05633875273873,11.2835945308545,-25.0623206876246));
#47290=CARTESIAN_POINT('Ctrl Pts',(-5.71232895575907,11.3934006872462,-25.0095886523243));
#47291=CARTESIAN_POINT('Ctrl Pts',(-5.02622191935904,11.5949850066956,-24.9146104214381));
#47292=CARTESIAN_POINT('Ctrl Pts',(-3.98582966114027,11.8491084122632,-24.7976169741646));
#47293=CARTESIAN_POINT('Ctrl Pts',(-2.81226414593484,12.0688095588167,-24.6984861183588));
#47294=CARTESIAN_POINT('Ctrl Pts',(-1.52049089173392,12.2251956038408,-24.6294270360226));
#47295=CARTESIAN_POINT('Ctrl Pts',(-0.189402768830715,12.2883719696366,
-24.602518522178));
#47296=CARTESIAN_POINT('Ctrl Pts',(1.08608586084807,12.2535038348118,-24.6172525448486));
#47297=CARTESIAN_POINT('Ctrl Pts',(2.24125031189288,12.1446943722227,-24.6648482773845));
#47298=CARTESIAN_POINT('Ctrl Pts',(3.27297079100125,11.9869972429091,-24.7352727477233));
#47299=CARTESIAN_POINT('Ctrl Pts',(4.19996253752107,11.7980284275134,-24.8210647839224));
#47300=CARTESIAN_POINT('Ctrl Pts',(5.05700893760704,11.5844416805762,-24.9196521454285));
#47301=CARTESIAN_POINT('Ctrl Pts',(5.68046392601282,11.4027971502045,-25.0051676719571));
#47302=CARTESIAN_POINT('Ctrl Pts',(6.02236021770785,11.294542540446,-25.0570504367922));
#47303=CARTESIAN_POINT('Ctrl Pts',(6.09429718612962,11.2713792138499,-25.0681981524802));
#47304=CARTESIAN_POINT('Ctrl Pts',(-6.21850174075154,11.6026144911347,-24.9351568017923));
#47305=CARTESIAN_POINT('Ctrl Pts',(-6.17967941190587,11.6150637612153,-24.9290290295733));
#47306=CARTESIAN_POINT('Ctrl Pts',(-5.82908090970353,11.726491587308,-24.8742543611295));
#47307=CARTESIAN_POINT('Ctrl Pts',(-5.12975016911477,11.9308145015291,-24.7750066996334));
#47308=CARTESIAN_POINT('Ctrl Pts',(-4.06876019721386,12.1879451786412,-24.6515284137366));
#47309=CARTESIAN_POINT('Ctrl Pts',(-2.87125002534106,12.4098505899583,-24.5458499626876));
#47310=CARTESIAN_POINT('Ctrl Pts',(-1.55244063361097,12.5674388783431,-24.4713861765985));
#47311=CARTESIAN_POINT('Ctrl Pts',(-0.193343170191578,12.6308275658389,
-24.4418368498252));
#47312=CARTESIAN_POINT('Ctrl Pts',(1.10885808493883,12.5958746635933,-24.4580801160618));
#47313=CARTESIAN_POINT('Ctrl Pts',(2.28833313380122,12.4863530460059,-24.5096523636422));
#47314=CARTESIAN_POINT('Ctrl Pts',(3.34139767194732,12.3272452030784,-24.5851371770129));
#47315=CARTESIAN_POINT('Ctrl Pts',(4.28714760515426,12.1362723269595,-24.6763093639965));
#47316=CARTESIAN_POINT('Ctrl Pts',(5.16111360517402,11.9201148911425,-24.7802386217786));
#47317=CARTESIAN_POINT('Ctrl Pts',(5.79660359327198,11.736017123652,-24.8696394150045));
#47318=CARTESIAN_POINT('Ctrl Pts',(6.1450501863258,11.626174088922,-24.9235557444498));
#47319=CARTESIAN_POINT('Ctrl Pts',(6.21836436549247,11.6026655148077,-24.9351277338151));
#47320=CARTESIAN_POINT('Ctrl Pts',(-6.32914231245861,11.8134514838489,-24.6414301321201));
#47321=CARTESIAN_POINT('Ctrl Pts',(-6.28961575230152,11.826020158596,-24.6351228661687));
#47322=CARTESIAN_POINT('Ctrl Pts',(-5.93266612704154,11.9384843908636,-24.578725067509));
#47323=CARTESIAN_POINT('Ctrl Pts',(-5.22080330516413,12.1441505239257,-24.4762093893228));
#47324=CARTESIAN_POINT('Ctrl Pts',(-4.14080139185458,12.4019094797043,-24.3479823384532));
#47325=CARTESIAN_POINT('Ctrl Pts',(-2.92180263005805,12.6234437730966,-24.2376755293907));
#47326=CARTESIAN_POINT('Ctrl Pts',(-1.57941068834376,12.7799962770451,-24.1595144784238));
#47327=CARTESIAN_POINT('Ctrl Pts',(-0.196615490582365,12.8424503644217,
-24.1282201087162));
#47328=CARTESIAN_POINT('Ctrl Pts',(1.1279890562748,12.8080728412826,-24.1454554856207));
#47329=CARTESIAN_POINT('Ctrl Pts',(2.32846050235933,12.6995118079923,-24.1997176236243));
#47330=CARTESIAN_POINT('Ctrl Pts',(3.40038217913011,12.5410385067355,-24.2787204343849));
#47331=CARTESIAN_POINT('Ctrl Pts',(4.36310491630567,12.3501384318674,-24.3737347034933));
#47332=CARTESIAN_POINT('Ctrl Pts',(5.25272701250916,12.1333494366402,-24.4815931017532));
#47333=CARTESIAN_POINT('Ctrl Pts',(5.89960976867062,11.9480757051294,-24.5739613947287));
#47334=CARTESIAN_POINT('Ctrl Pts',(6.25435740425776,11.8372353972519,-24.6294877375989));
#47335=CARTESIAN_POINT('Ctrl Pts',(6.32900167463278,11.813500894588,-24.6413984641695));
#47336=CARTESIAN_POINT('Ctrl Pts',(-6.39488491639353,11.843659109667,-24.2701454915518));
#47337=CARTESIAN_POINT('Ctrl Pts',(-6.3548792244511,11.8562498366404,-24.263755202918));
#47338=CARTESIAN_POINT('Ctrl Pts',(-5.99362126599835,11.9688694024556,-24.2066159318454));
#47339=CARTESIAN_POINT('Ctrl Pts',(-5.27348053464344,12.1740985697827,-24.1027645072777));
#47340=CARTESIAN_POINT('Ctrl Pts',(-4.18145826340194,12.4299229451767,-23.9728780259458));
#47341=CARTESIAN_POINT('Ctrl Pts',(-2.94953848407,12.6486104098926,-23.8611815544649));
#47342=CARTESIAN_POINT('Ctrl Pts',(-1.5937263245113,12.8021783961345,-23.7820850898753));
#47343=CARTESIAN_POINT('Ctrl Pts',(-0.19828839899972,12.8628139539125,-23.7504393128011));
#47344=CARTESIAN_POINT('Ctrl Pts',(1.13803452697083,12.8295099441217,-23.7678665979002));
#47345=CARTESIAN_POINT('Ctrl Pts',(2.35021459441548,12.723313039055,-23.8227647798885));
#47346=CARTESIAN_POINT('Ctrl Pts',(3.4331426425149,12.5673438207858,-23.9027401395622));
#47347=CARTESIAN_POINT('Ctrl Pts',(4.40622596342085,12.3785773849159,-23.9989632401039));
#47348=CARTESIAN_POINT('Ctrl Pts',(5.30578912917227,12.1632797707017,-24.1082183846146));
#47349=CARTESIAN_POINT('Ctrl Pts',(5.96018372008034,11.9784443662577,-24.2017911337946));
#47350=CARTESIAN_POINT('Ctrl Pts',(6.31919213586667,11.867482639712,-24.2580455020914));
#47351=CARTESIAN_POINT('Ctrl Pts',(6.39474132614597,11.8437059930189,-24.2701129850578));
#47352=CARTESIAN_POINT('',(-5.98852245733775,11.3308498383565,-25.0410395152735));
#47353=CARTESIAN_POINT('Ctrl Pts',(-5.98852261949162,11.3308502493357,-25.0410393033403));
#47354=CARTESIAN_POINT('Ctrl Pts',(-5.87206434378358,11.3676808033278,-25.0233565226301));
#47355=CARTESIAN_POINT('Ctrl Pts',(-5.74891036709195,11.4056203108354,-25.0052460172911));
#47356=CARTESIAN_POINT('Ctrl Pts',(-5.61905842407995,11.4443053364402,-24.9868889199126));
#47357=CARTESIAN_POINT('Ctrl Pts',(-5.51153067681731,11.4763396176347,-24.9716877817424));
#47358=CARTESIAN_POINT('Ctrl Pts',(-5.39940999143908,11.5088843415234,-24.9563177908387));
#47359=CARTESIAN_POINT('Ctrl Pts',(-5.28269811087122,11.5417066610665,-24.9408868513054));
#47360=CARTESIAN_POINT('Ctrl Pts',(-5.21045748179925,11.5620225449325,-24.9313356318954));
#47361=CARTESIAN_POINT('Ctrl Pts',(-5.13645747600364,11.5824416608345,-24.9217623183797));
#47362=CARTESIAN_POINT('Ctrl Pts',(-5.06069821746738,11.6028970082404,-24.9121963780487));
#47363=CARTESIAN_POINT('Ctrl Pts',(-5.00135512740382,11.6189199148375,-24.9047032680372));
#47364=CARTESIAN_POINT('Ctrl Pts',(-4.94093262964919,11.6349649716179,-24.8972146778942));
#47365=CARTESIAN_POINT('Ctrl Pts',(-4.8794305921878,11.6509987287575,-24.8897461628098));
#47366=CARTESIAN_POINT('Ctrl Pts',(-4.80942185405327,11.6692502071026,-24.8812446344316));
#47367=CARTESIAN_POINT('Ctrl Pts',(-4.73801437161174,11.687486798311,-24.8727692375187));
#47368=CARTESIAN_POINT('Ctrl Pts',(-4.66520814405306,11.7056554054938,-24.8643442713963));
#47369=CARTESIAN_POINT('Ctrl Pts',(-4.62880503027372,11.7147397090852,-24.8601317883351));
#47370=CARTESIAN_POINT('Ctrl Pts',(-4.59205223025826,11.7238070144719,-24.8559319079964));
#47371=CARTESIAN_POINT('Ctrl Pts',(-4.55494974407041,11.7328503323779,-24.8517477910442));
#47372=CARTESIAN_POINT('Ctrl Pts',(-4.53639850097649,11.7373719913309,-24.8496557325681));
#47373=CARTESIAN_POINT('Ctrl Pts',(-4.51775983634088,11.7418876532688,-24.8475676146158));
#47374=CARTESIAN_POINT('Ctrl Pts',(-4.49903375017708,11.7463964357147,-24.8454838338858));
#47375=CARTESIAN_POINT('Ctrl Pts',(-4.48967070709519,11.7486508269376,-24.8444419435208));
#47376=CARTESIAN_POINT('Ctrl Pts',(-4.48028580863127,11.7509034982779,-24.8434011374401));
#47377=CARTESIAN_POINT('Ctrl Pts',(-4.47087905478714,11.7531543382301,-24.8423614656213));
#47378=CARTESIAN_POINT('Ctrl Pts',(-4.46147230094301,11.7554051781823,-24.8413217938026));
#47379=CARTESIAN_POINT('Ctrl Pts',(-4.45080026163169,11.7579498409444,-24.8401467680703));
#47380=CARTESIAN_POINT('Ctrl Pts',(-4.44259322711588,11.7599012520483,-24.8392459029919));
#47381=CARTESIAN_POINT('Ctrl Pts',(-4.30856578831259,11.7917693563927,-24.8245340556212));
#47382=CARTESIAN_POINT('Ctrl Pts',(-4.17021571232689,11.8233378307119,-24.8100191830527));
#47383=CARTESIAN_POINT('Ctrl Pts',(-4.02753511600434,11.854287492411,-24.7958396904698));
#47384=CARTESIAN_POINT('Ctrl Pts',(-3.89063485295398,11.8839833090611,-24.7822346431504));
#47385=CARTESIAN_POINT('Ctrl Pts',(-3.74974763050038,11.9131091571202,-24.7689383171711));
#47386=CARTESIAN_POINT('Ctrl Pts',(-3.60488117571044,11.9413675073944,-24.7560825402895));
#47387=CARTESIAN_POINT('Ctrl Pts',(-3.4569563762176,11.9702224331561,-24.7429553589812));
#47388=CARTESIAN_POINT('Ctrl Pts',(-3.30487851548619,11.9981719243682,-24.7302880082315));
#47389=CARTESIAN_POINT('Ctrl Pts',(-3.14864759365074,12.0248803860776,-24.7182264051025));
#47390=CARTESIAN_POINT('Ctrl Pts',(-3.07053213273301,12.0382346169323,-24.7121956035379));
#47391=CARTESIAN_POINT('Ctrl Pts',(-2.99137840642891,12.0512783404329,-24.7063163011558));
#47392=CARTESIAN_POINT('Ctrl Pts',(-2.91118641388078,12.0639682856377,-24.7006069887942));
#47393=CARTESIAN_POINT('Ctrl Pts',(-2.89492183652573,12.0665420662466,-24.6994490233964));
#47394=CARTESIAN_POINT('Ctrl Pts',(-2.87861455189655,12.0691012967118,-24.6982980484005));
#47395=CARTESIAN_POINT('Ctrl Pts',(-2.86226455461567,12.0716456047884,-24.6971542220298));
#47396=CARTESIAN_POINT('Ctrl Pts',(-2.83830797547933,12.0753736126124,-24.6954782482362));
#47397=CARTESIAN_POINT('Ctrl Pts',(-2.81425969567364,12.079069583887,-24.6938176217293));
#47398=CARTESIAN_POINT('Ctrl Pts',(-2.7901197252096,12.0827323810601,-24.6921728353577));
#47399=CARTESIAN_POINT('Ctrl Pts',(-2.76981216045503,12.0858136810512,-24.6907891714547));
#47400=CARTESIAN_POINT('Ctrl Pts',(-2.74943970405002,12.0888715008226,-24.6894167189943));
#47401=CARTESIAN_POINT('Ctrl Pts',(-2.72900235600345,12.0919051557977,-24.6880557739761));
#47402=CARTESIAN_POINT('Ctrl Pts',(-2.71878368198016,12.0934219832853,-24.687375301467));
#47403=CARTESIAN_POINT('Ctrl Pts',(-2.70854878504645,12.0949327695685,-24.6866977058071));
#47404=CARTESIAN_POINT('Ctrl Pts',(-2.69829766520351,12.0964374288369,-24.6860230240256));
#47405=CARTESIAN_POINT('Ctrl Pts',(-2.68804654536057,12.0979420881053,-24.6853483422442));
#47406=CARTESIAN_POINT('Ctrl Pts',(-2.67637482462903,12.0996444193795,-24.6845852371531));
#47407=CARTESIAN_POINT('Ctrl Pts',(-2.66749563694813,12.1009329397115,-24.6840077573249));
#47408=CARTESIAN_POINT('Ctrl Pts',(-2.48177212083922,12.1278845635803,-24.67192877127));
#47409=CARTESIAN_POINT('Ctrl Pts',(-2.29115211409166,12.1528042226412,-24.6608136069641));
#47410=CARTESIAN_POINT('Ctrl Pts',(-2.09562977712304,12.175220720871,-24.6508597438541));
#47411=CARTESIAN_POINT('Ctrl Pts',(-1.99202712449424,12.187098692029,-24.6455854276911));
#47412=CARTESIAN_POINT('Ctrl Pts',(-1.88704840017349,12.1982731209495,-24.6406374110466));
#47413=CARTESIAN_POINT('Ctrl Pts',(-1.78069528395011,12.2086687666313,-24.6360467563646));
#47414=CARTESIAN_POINT('Ctrl Pts',(-1.69992409321344,12.2165638684395,-24.6325603268353));
#47415=CARTESIAN_POINT('Ctrl Pts',(-1.61836026605962,12.224010927817,-24.629279446292));
#47416=CARTESIAN_POINT('Ctrl Pts',(-1.53600234379191,12.2309786067084,-24.6262166791347));
#47417=CARTESIAN_POINT('Ctrl Pts',(-1.46181103399259,12.2372553704852,-24.623457616002));
#47418=CARTESIAN_POINT('Ctrl Pts',(-1.38697529504412,12.2431430893884,-24.620875568631));
#47419=CARTESIAN_POINT('Ctrl Pts',(-1.31149638890661,12.2486185489259,-24.6184788953444));
#47420=CARTESIAN_POINT('Ctrl Pts',(-1.23186331041638,12.2543953642169,-24.6159503150865));
#47421=CARTESIAN_POINT('Ctrl Pts',(-1.15151359877784,12.2597132633044,-24.6136280968113));
#47422=CARTESIAN_POINT('Ctrl Pts',(-1.07044725243966,12.2645452944849,-24.6115216096605));
#47423=CARTESIAN_POINT('Ctrl Pts',(-1.02991407927057,12.2669613100752,-24.610468366085));
#47424=CARTESIAN_POINT('Ctrl Pts',(-0.989201747425264,12.269255856687,-24.6094690513367));
#47425=CARTESIAN_POINT('Ctrl Pts',(-0.948310256806896,12.2714255828555,
-24.6085247974033));
#47426=CARTESIAN_POINT('Ctrl Pts',(-0.927864511497712,12.2725104459398,
-24.6080526704366));
#47427=CARTESIAN_POINT('Ctrl Pts',(-0.907373976495706,12.2735641037824,
-24.6075943084147));
#47428=CARTESIAN_POINT('Ctrl Pts',(-0.886838651798443,12.2745861390056,
-24.6071498500979));
#47429=CARTESIAN_POINT('Ctrl Pts',(-0.876570989449812,12.2750971566172,
-24.6069276209395));
#47430=CARTESIAN_POINT('Ctrl Pts',(-0.866292129677403,12.2756002685656,
-24.6067088676909));
#47431=CARTESIAN_POINT('Ctrl Pts',(-0.856002072481586,12.276095422804,-24.6064936075101));
#47432=CARTESIAN_POINT('Ctrl Pts',(-0.84571201528577,12.2765905770423,-24.6062783473294));
#47433=CARTESIAN_POINT('Ctrl Pts',(-0.833723425588129,12.2771561786407,
-24.6060325049814));
#47434=CARTESIAN_POINT('Ctrl Pts',(-0.82509830862458,12.2775569603653,-24.6058583232348));
#47435=CARTESIAN_POINT('Ctrl Pts',(-0.60331200137841,12.2878626639384,-24.6013794128003));
#47436=CARTESIAN_POINT('Ctrl Pts',(-0.37942147470136,12.2940995949959,-24.5986970076597));
#47437=CARTESIAN_POINT('Ctrl Pts',(-0.153422040659201,12.2960206310907,
-24.5978631981353));
#47438=CARTESIAN_POINT('Ctrl Pts',(-0.0981746725502134,12.2964902437192,
-24.5976593667323));
#47439=CARTESIAN_POINT('Ctrl Pts',(-0.0428013115823766,12.2967017237989,
-24.5975660637919));
#47440=CARTESIAN_POINT('Ctrl Pts',(0.0126974871764322,12.2966538031459,
-24.5975843468163));
#47441=CARTESIAN_POINT('Ctrl Pts',(0.15396086503864,12.2965318287344,-24.597630883351));
#47442=CARTESIAN_POINT('Ctrl Pts',(0.296039615275695,12.2947248108631,-24.5984025596996));
#47443=CARTESIAN_POINT('Ctrl Pts',(0.43893375204779,12.2912000474167,-24.5999229059135));
#47444=CARTESIAN_POINT('Ctrl Pts',(0.510380820433836,12.2894376656936,-24.6006830790204));
#47445=CARTESIAN_POINT('Ctrl Pts',(0.582031734977933,12.2872458491615,-24.6016304233117));
#47446=CARTESIAN_POINT('Ctrl Pts',(0.65388649564414,12.2846217901291,-24.6027672829694));
#47447=CARTESIAN_POINT('Ctrl Pts',(0.689813875977243,12.2833097606128,-24.6033357127982));
#47448=CARTESIAN_POINT('Ctrl Pts',(0.725792217826846,12.2818896707049,-24.6039515219213));
#47449=CARTESIAN_POINT('Ctrl Pts',(0.761821521118555,12.2803612097145,-24.6046149872946));
#47450=CARTESIAN_POINT('Ctrl Pts',(0.779836172764409,12.2795969792193,-24.6049467199812));
#47451=CARTESIAN_POINT('Ctrl Pts',(0.797863564770144,12.2788056559728,-24.6052903667671));
#47452=CARTESIAN_POINT('Ctrl Pts',(0.815903697124266,12.2779872059043,-24.6056459601989));
#47453=CARTESIAN_POINT('Ctrl Pts',(0.833943829478388,12.2771687558359,-24.6060015536307));
#47454=CARTESIAN_POINT('Ctrl Pts',(0.853616708411465,12.2762449172183,-24.6064031266869));
#47455=CARTESIAN_POINT('Ctrl Pts',(0.870062315218929,12.2754504426786,-24.6067486124422));
#47456=CARTESIAN_POINT('Ctrl Pts',(0.95490688162133,12.2713516673258,-24.6085310087654));
#47457=CARTESIAN_POINT('Ctrl Pts',(1.03913119396567,12.2666920819471,-24.6105613373092));
#47458=CARTESIAN_POINT('Ctrl Pts',(1.12272942610553,12.2614987222179,-24.6128297808952));
#47459=CARTESIAN_POINT('Ctrl Pts',(1.3402298823131,12.2479869758395,-24.6187316702318));
#47460=CARTESIAN_POINT('Ctrl Pts',(1.553491070849,12.2308655865203,-24.6262443285959));
#47461=CARTESIAN_POINT('Ctrl Pts',(1.76251278772209,12.2106188688103,-24.6351844059209));
#47462=CARTESIAN_POINT('Ctrl Pts',(1.93917904843176,12.193506235908,-24.6427406065641));
#47463=CARTESIAN_POINT('Ctrl Pts',(2.11281720147879,12.174160036699,-24.6513167790797));
#47464=CARTESIAN_POINT('Ctrl Pts',(2.28343846124246,12.1528471286757,-24.6608097041831));
#47465=CARTESIAN_POINT('Ctrl Pts',(2.3146215826453,12.1489519341422,-24.6625446523154));
#47466=CARTESIAN_POINT('Ctrl Pts',(2.34570395955438,12.1449909873965,-24.6643102395043));
#47467=CARTESIAN_POINT('Ctrl Pts',(2.37668568819775,12.1409658927933,-24.6661058189143));
#47468=CARTESIAN_POINT('Ctrl Pts',(2.477450908615,12.1278746431226,-24.6719457756552));
#47469=CARTESIAN_POINT('Ctrl Pts',(2.57802287628754,12.1139949965248,-24.6781518005778));
#47470=CARTESIAN_POINT('Ctrl Pts',(2.67763147125897,12.0994620485983,-24.6846663127365));
#47471=CARTESIAN_POINT('Ctrl Pts',(2.77938420239324,12.084616270045,-24.6913210537691));
#47472=CARTESIAN_POINT('Ctrl Pts',(2.88013149186452,12.0690888669585,-24.6982976933924));
#47473=CARTESIAN_POINT('Ctrl Pts',(2.97906267521312,12.0530722864747,-24.7055117542209));
#47474=CARTESIAN_POINT('Ctrl Pts',(3.01306542757817,12.0475673708203,-24.7079912345586));
#47475=CARTESIAN_POINT('Ctrl Pts',(3.04685374015803,12.0420050730082,-24.7104985660293));
#47476=CARTESIAN_POINT('Ctrl Pts',(3.08039501457754,12.0363944358889,-24.7130297203968));
#47477=CARTESIAN_POINT('Ctrl Pts',(3.1589490848206,12.0232542559167,-24.7189577145299));
#47478=CARTESIAN_POINT('Ctrl Pts',(3.2363619939274,12.0098153834099,-24.7250314766478));
#47479=CARTESIAN_POINT('Ctrl Pts',(3.31263226369929,11.9961218910734,-24.7312316528785));
#47480=CARTESIAN_POINT('Ctrl Pts',(3.45643416665273,11.9703038329761,-24.7429216225521));
#47481=CARTESIAN_POINT('Ctrl Pts',(3.59617381541188,11.9435821435806,-24.7550605159897));
#47482=CARTESIAN_POINT('Ctrl Pts',(3.73185546034114,11.9162415601785,-24.7675242517846));
#47483=CARTESIAN_POINT('Ctrl Pts',(3.83567798906037,11.89532076056,-24.7770614044938));
#47484=CARTESIAN_POINT('Ctrl Pts',(3.93712341204653,11.874037281912,-24.7867888199111));
#47485=CARTESIAN_POINT('Ctrl Pts',(4.03619172864908,11.8525110818394,-24.7966530844071));
#47486=CARTESIAN_POINT('Ctrl Pts',(4.06095880779972,11.8471295318213,-24.7991191505311));
#47487=CARTESIAN_POINT('Ctrl Pts',(4.08659007135158,11.8415152815526,-24.8016933679325));
#47488=CARTESIAN_POINT('Ctrl Pts',(4.11454680505952,11.8353264265799,-24.8045332735786));
#47489=CARTESIAN_POINT('Ctrl Pts',(4.14250353876745,11.8291375716072,-24.8073731792247));
#47490=CARTESIAN_POINT('Ctrl Pts',(4.17028170984898,11.8229263741544,-24.810225435238));
#47491=CARTESIAN_POINT('Ctrl Pts',(4.19788131832375,11.8166954630904,-24.8130888540882));
#47492=CARTESIAN_POINT('Ctrl Pts',(4.20564503586813,11.8149427196198,-24.8138943283827));
#47493=CARTESIAN_POINT('Ctrl Pts',(4.21339462460221,11.8131884156165,-24.8147006862325));
#47494=CARTESIAN_POINT('Ctrl Pts',(4.22113008395014,11.8114326080531,-24.8155079018423));
#47495=CARTESIAN_POINT('Ctrl Pts',(4.26839292874062,11.8007048081103,-24.8204399045018));
#47496=CARTESIAN_POINT('Ctrl Pts',(4.31512830212096,11.7899209103131,-24.8254039196623));
#47497=CARTESIAN_POINT('Ctrl Pts',(4.36133621816581,11.7790939163167,-24.830394262819));
#47498=CARTESIAN_POINT('Ctrl Pts',(4.5192928999517,11.7420830274521,-24.8474532023575));
#47499=CARTESIAN_POINT('Ctrl Pts',(4.6710868612562,11.7045739579164,-24.8648180143462));
#47500=CARTESIAN_POINT('Ctrl Pts',(4.81671584757079,11.6670461923498,-24.8822738066032));
#47501=CARTESIAN_POINT('Ctrl Pts',(4.86938363032469,11.6534740028144,-24.8885868209121));
#47502=CARTESIAN_POINT('Ctrl Pts',(4.92124518390333,11.6398989012584,-24.894911863262));
#47503=CARTESIAN_POINT('Ctrl Pts',(4.97230079099022,11.6263420121853,-24.9012392056704));
#47504=CARTESIAN_POINT('Ctrl Pts',(5.00457282564062,11.6177727595824,-24.9052386922126));
#47505=CARTESIAN_POINT('Ctrl Pts',(5.03652280196598,11.6092116132764,-24.9092387214196));
#47506=CARTESIAN_POINT('Ctrl Pts',(5.06815068438951,11.6006631633034,-24.9132371465457));
#47507=CARTESIAN_POINT('Ctrl Pts',(5.21038989559504,11.5622184528763,-24.931219154585));
#47508=CARTESIAN_POINT('Ctrl Pts',(5.34611433022111,11.5240346408721,-24.9491680609103));
#47509=CARTESIAN_POINT('Ctrl Pts',(5.47532353418555,11.4865031871949,-24.9669056709416));
#47510=CARTESIAN_POINT('Ctrl Pts',(5.60704917663317,11.4482407825369,-24.9849887331784));
#47511=CARTESIAN_POINT('Ctrl Pts',(5.73200353346943,11.4106562721611,-25.0028520396424));
#47512=CARTESIAN_POINT('Ctrl Pts',(5.85018815143144,11.3741116577444,-25.0203170142959));
#47513=CARTESIAN_POINT('Ctrl Pts',(5.86232620871315,11.370358372158,-25.0221107406406));
#47514=CARTESIAN_POINT('Ctrl Pts',(5.87439285795211,11.3666160114644,-25.0239002752262));
#47515=CARTESIAN_POINT('Ctrl Pts',(5.88638810071823,11.3628849378978,-25.0256854315412));
#47516=CARTESIAN_POINT('Ctrl Pts',(5.92102970000301,11.3521098032951,-25.030840864485));
#47517=CARTESIAN_POINT('Ctrl Pts',(5.95507574647161,11.3414288270981,-25.0359597835312));
#47518=CARTESIAN_POINT('Ctrl Pts',(5.98852582557461,11.3308501354092,-25.0410382780203));
#47519=CARTESIAN_POINT('',(-6.27159361731535,11.8794975616035,-24.2690120888704));
#47520=CARTESIAN_POINT('Origin',(-5.999994980806,10.9277770011849,-24.1259380084193));
#47521=CARTESIAN_POINT('Ctrl Pts',(-6.27159386307714,11.8794985003159,-24.2690123725043));
#47522=CARTESIAN_POINT('Ctrl Pts',(-6.19708063788404,11.9025009437873,-24.2574475519448));
#47523=CARTESIAN_POINT('Ctrl Pts',(-6.1154389212118,11.9272858632909,-24.2450493518731));
#47524=CARTESIAN_POINT('Ctrl Pts',(-6.02658468059905,11.9536191513622,-24.2319368683802));
#47525=CARTESIAN_POINT('Ctrl Pts',(-5.93855991338491,11.9797066125399,-24.2189467927338));
#47526=CARTESIAN_POINT('Ctrl Pts',(-5.84345650103252,12.0073138014567,-24.2052557265519));
#47527=CARTESIAN_POINT('Ctrl Pts',(-5.74118376321366,12.0361672962737,-24.1909996607511));
#47528=CARTESIAN_POINT('Ctrl Pts',(-5.64049526534308,12.064573840514,-24.1769644263216));
#47529=CARTESIAN_POINT('Ctrl Pts',(-5.53285766402706,12.0941884806745,-24.1623815976342));
#47530=CARTESIAN_POINT('Ctrl Pts',(-5.41817807500658,12.1247040286673,-24.1474001686258));
#47531=CARTESIAN_POINT('Ctrl Pts',(-5.37925205568429,12.1350620079812,-24.1423149795348));
#47532=CARTESIAN_POINT('Ctrl Pts',(-5.33951465291907,12.1455233798207,-24.1371840288087));
#47533=CARTESIAN_POINT('Ctrl Pts',(-5.29896211848521,12.1560748552828,-24.1320136472455));
#47534=CARTESIAN_POINT('Ctrl Pts',(-5.21821342548053,12.1770850797912,-24.1217183214566));
#47535=CARTESIAN_POINT('Ctrl Pts',(-5.13423279998965,12.1984532303221,-24.1112662958196));
#47536=CARTESIAN_POINT('Ctrl Pts',(-5.04699089619075,12.2200666393085,-24.1007138120776));
#47537=CARTESIAN_POINT('Ctrl Pts',(-4.92201131250236,12.2510292242542,-24.0855967070222));
#47538=CARTESIAN_POINT('Ctrl Pts',(-4.79033868087646,12.282497284018,-24.0702723742906));
#47539=CARTESIAN_POINT('Ctrl Pts',(-4.65188708480657,12.3140998001835,-24.0549259456217));
#47540=CARTESIAN_POINT('Ctrl Pts',(-4.51343548873669,12.3457023163489,-24.0395795169528));
#47541=CARTESIAN_POINT('Ctrl Pts',(-4.36820473066936,12.3774395505853,-24.024210870021));
#47542=CARTESIAN_POINT('Ctrl Pts',(-4.21611190204382,12.4088902288773,-24.0090300413631));
#47543=CARTESIAN_POINT('Ctrl Pts',(-4.07082877054265,12.4389327566637,-23.9945289084291));
#47544=CARTESIAN_POINT('Ctrl Pts',(-3.91928373183408,12.4687134990666,-23.9801991837209));
#47545=CARTESIAN_POINT('Ctrl Pts',(-3.76142159657237,12.4978246559702,-23.9662477012005));
#47546=CARTESIAN_POINT('Ctrl Pts',(-3.73054731973014,12.5035181423527,-23.9635191055625));
#47547=CARTESIAN_POINT('Ctrl Pts',(-3.69943144642957,12.5091858792516,-23.9608050504824));
#47548=CARTESIAN_POINT('Ctrl Pts',(-3.66807361915617,12.5148246128436,-23.9581071905609));
#47549=CARTESIAN_POINT('Ctrl Pts',(-3.58017497289932,12.530630460775,-23.9505448606574));
#47550=CARTESIAN_POINT('Ctrl Pts',(-3.49037512701031,12.5462087349511,-23.9431096148398));
#47551=CARTESIAN_POINT('Ctrl Pts',(-3.39866710774328,12.5614848736542,-23.935839448839));
#47552=CARTESIAN_POINT('Ctrl Pts',(-3.35281309810976,12.5691229430058,-23.9322043658387));
#47553=CARTESIAN_POINT('Ctrl Pts',(-3.3064820361792,12.5766854208569,-23.9286105461331));
#47554=CARTESIAN_POINT('Ctrl Pts',(-3.25967322046985,12.5841625651488,-23.9250630070349));
#47555=CARTESIAN_POINT('Ctrl Pts',(-3.23626881261517,12.5879011372948,-23.9232892374858));
#47556=CARTESIAN_POINT('Ctrl Pts',(-3.21274496571995,12.5916183723679,-23.9215270376585));
#47557=CARTESIAN_POINT('Ctrl Pts',(-3.18910159606633,12.5953130280354,-23.9197770413011));
#47558=CARTESIAN_POINT('Ctrl Pts',(-3.17727991123952,12.5971603558692,-23.9189020431224));
#47559=CARTESIAN_POINT('Ctrl Pts',(-3.16542834568841,12.5990020386154,-23.9180300957842));
#47560=CARTESIAN_POINT('Ctrl Pts',(-3.15354688958086,12.6008379193071,-23.9171612794639));
#47561=CARTESIAN_POINT('Ctrl Pts',(-3.14166543347331,12.6026737999988,-23.9162924631437));
#47562=CARTESIAN_POINT('Ctrl Pts',(-3.12814004437027,12.6047504362156,-23.9153102011917));
#47563=CARTESIAN_POINT('Ctrl Pts',(-3.11781283988084,12.6063279972199,-23.914564303968));
#47564=CARTESIAN_POINT('Ctrl Pts',(-3.07662101472915,12.6126203696738,-23.9115891650469));
#47565=CARTESIAN_POINT('Ctrl Pts',(-3.03568844271223,12.6187482436968,-23.9086933705156));
#47566=CARTESIAN_POINT('Ctrl Pts',(-2.99501685896893,12.6247159725055,-23.9058747757425));
#47567=CARTESIAN_POINT('Ctrl Pts',(-2.79740091771027,12.6537120979859,-23.892179728541));
#47568=CARTESIAN_POINT('Ctrl Pts',(-2.60595035920182,12.6789291266892,-23.880306669677));
#47569=CARTESIAN_POINT('Ctrl Pts',(-2.42085823416444,12.7008772951465,-23.8700052682326));
#47570=CARTESIAN_POINT('Ctrl Pts',(-2.23093018158733,12.7233989064354,-23.8594347206484));
#47571=CARTESIAN_POINT('Ctrl Pts',(-2.04769684133198,12.7424789282856,-23.8505188343068));
#47572=CARTESIAN_POINT('Ctrl Pts',(-1.87131798152509,12.758644782564,-23.8429959900435));
#47573=CARTESIAN_POINT('Ctrl Pts',(-1.78117118117997,12.7669071108251,-23.8391510828899));
#47574=CARTESIAN_POINT('Ctrl Pts',(-1.69281416813676,12.7744077891968,-23.8356702264102));
#47575=CARTESIAN_POINT('Ctrl Pts',(-1.60626396046494,12.7812145160159,-23.8325195992654));
#47576=CARTESIAN_POINT('Ctrl Pts',(-1.43907018368183,12.7943634430379,-23.8264333602402));
#47577=CARTESIAN_POINT('Ctrl Pts',(-1.27862092434264,12.8049252529317,-23.8215783807087));
#47578=CARTESIAN_POINT('Ctrl Pts',(-1.12501574086879,12.8133804823945,-23.8177149964479));
#47579=CARTESIAN_POINT('Ctrl Pts',(-0.969938834043967,12.8219167231771,
-23.8138145962954));
#47580=CARTESIAN_POINT('Ctrl Pts',(-0.82183738744044,12.8283059524179,-23.8109247713977));
#47581=CARTESIAN_POINT('Ctrl Pts',(-0.680781472353746,12.8330037303229,
-23.8088158751191));
#47582=CARTESIAN_POINT('Ctrl Pts',(-0.538387190839892,12.8377460816741,
-23.8066869692154));
#47583=CARTESIAN_POINT('Ctrl Pts',(-0.40317239011466,12.8407648691305,-23.8053537705296));
#47584=CARTESIAN_POINT('Ctrl Pts',(-0.2751822190389,12.8424872425574,-23.8045989425387));
#47585=CARTESIAN_POINT('Ctrl Pts',(-0.236222340744794,12.8430115285907,
-23.8043691748432));
#47586=CARTESIAN_POINT('Ctrl Pts',(-0.197931715385525,12.8434153954412,
-23.8041931354355));
#47587=CARTESIAN_POINT('Ctrl Pts',(-0.160311209395224,12.8437101078661,
-23.8040650611514));
#47588=CARTESIAN_POINT('Ctrl Pts',(-0.153998805357433,12.8437595581288,
-23.8040435713652));
#47589=CARTESIAN_POINT('Ctrl Pts',(-0.147705267480093,12.8438059344178,
-23.804023432385));
#47590=CARTESIAN_POINT('Ctrl Pts',(-0.141430599074373,12.843849289921,-23.8040046162681));
#47591=CARTESIAN_POINT('Ctrl Pts',(-0.103047863108373,12.8441144996061,
-23.8038895163139));
#47592=CARTESIAN_POINT('Ctrl Pts',(-0.0662557649282347,12.844264401576,
-23.8038251195063));
#47593=CARTESIAN_POINT('Ctrl Pts',(-0.0289811583181769,12.8443170156573,
-23.8038019482852));
#47594=CARTESIAN_POINT('Ctrl Pts',(-0.0185590826975259,12.8443317266893,
-23.8037954695523));
#47595=CARTESIAN_POINT('Ctrl Pts',(-0.00809928444716131,12.8443385554483,
-23.803792357389));
#47596=CARTESIAN_POINT('Ctrl Pts',(0.00244355322809239,12.8443372524163,
-23.8037927386336));
#47597=CARTESIAN_POINT('Ctrl Pts',(0.127127961177523,12.8443218421664,-23.8037972474059));
#47598=CARTESIAN_POINT('Ctrl Pts',(0.258986374602228,12.8431696770572,-23.8042924738699));
#47599=CARTESIAN_POINT('Ctrl Pts',(0.397985575007477,12.8404650174786,-23.8054910540718));
#47600=CARTESIAN_POINT('Ctrl Pts',(0.535666628784619,12.8377860065216,-23.8066782679893));
#47601=CARTESIAN_POINT('Ctrl Pts',(0.680354002368223,12.8335836937305,-23.8085556417309));
#47602=CARTESIAN_POINT('Ctrl Pts',(0.831993459648986,12.8274126547388,-23.8113495682372));
#47603=CARTESIAN_POINT('Ctrl Pts',(0.942266738698048,12.8229250318144,-23.8133813312283));
#47604=CARTESIAN_POINT('Ctrl Pts',(1.05621605905989,12.8173954294566,-23.8158982066978));
#47605=CARTESIAN_POINT('Ctrl Pts',(1.17381162283179,12.8106390770448,-23.8189935431595));
#47606=CARTESIAN_POINT('Ctrl Pts',(1.33437225665151,12.8014142033273,-23.8232198010917));
#47607=CARTESIAN_POINT('Ctrl Pts',(1.5017320685743,12.7899032047958,-23.8285241622485));
#47608=CARTESIAN_POINT('Ctrl Pts',(1.67578004683143,12.7756204063144,-23.8351494352146));
#47609=CARTESIAN_POINT('Ctrl Pts',(1.8437866770057,12.7618333754834,-23.8415447395218));
#47610=CARTESIAN_POINT('Ctrl Pts',(2.01802545755619,12.7454633391203,-23.8491710217748));
#47611=CARTESIAN_POINT('Ctrl Pts',(2.19835985514866,12.7260475950067,-23.8582571155746));
#47612=CARTESIAN_POINT('Ctrl Pts',(2.26108424966836,12.7192943587415,-23.8614174651238));
#47613=CARTESIAN_POINT('Ctrl Pts',(2.32454574572609,12.7121724347413,-23.8647545068279));
#47614=CARTESIAN_POINT('Ctrl Pts',(2.38873742216605,12.7046616766872,-23.8682781206306));
#47615=CARTESIAN_POINT('Ctrl Pts',(2.47500004842828,12.6945685033834,-23.8730132544892));
#47616=CARTESIAN_POINT('Ctrl Pts',(2.56258134583149,12.6837731521358,-23.8780853123256));
#47617=CARTESIAN_POINT('Ctrl Pts',(2.65146464768891,12.6722277501361,-23.8835179324179));
#47618=CARTESIAN_POINT('Ctrl Pts',(2.72897721473141,12.6621593376465,-23.8882555639001));
#47619=CARTESIAN_POINT('Ctrl Pts',(2.80747997654866,12.6515204820078,-23.8932674650598));
#47620=CARTESIAN_POINT('Ctrl Pts',(2.88696064472235,12.6402790323444,-23.8985693852204));
#47621=CARTESIAN_POINT('Ctrl Pts',(2.92670097880919,12.6346583075128,-23.9012203453007));
#47622=CARTESIAN_POINT('Ctrl Pts',(2.96668578829657,12.6288869265186,-23.9039438092491));
#47623=CARTESIAN_POINT('Ctrl Pts',(3.00691341611986,12.6229608373452,-23.9067417717684));
#47624=CARTESIAN_POINT('Ctrl Pts',(3.0270272300315,12.6199977927584,-23.9081407530281));
#47625=CARTESIAN_POINT('Ctrl Pts',(3.04720174847246,12.6169960706657,-23.90955835888));
#47626=CARTESIAN_POINT('Ctrl Pts',(3.06743675972051,12.6139551624287,-23.9109948380374));
#47627=CARTESIAN_POINT('Ctrl Pts',(3.07755426534454,12.6124347083102,-23.9117130776161));
#47628=CARTESIAN_POINT('Ctrl Pts',(3.08768689416621,12.6109044576268,-23.9124360355178));
#47629=CARTESIAN_POINT('Ctrl Pts',(3.09783461924249,12.6093643466848,-23.9131637428685));
#47630=CARTESIAN_POINT('Ctrl Pts',(3.10798234431877,12.6078242357429,-23.9138914502192));
#47631=CARTESIAN_POINT('Ctrl Pts',(3.11649243293453,12.6065275675155,-23.9145041910091));
#47632=CARTESIAN_POINT('Ctrl Pts',(3.12832305613605,12.6047143692937,-23.9153611443954));
#47633=CARTESIAN_POINT('Ctrl Pts',(3.24396819268312,12.5869902348685,-23.9237379213154));
#47634=CARTESIAN_POINT('Ctrl Pts',(3.35682173873388,12.5687084797174,-23.9324156970004));
#47635=CARTESIAN_POINT('Ctrl Pts',(3.46689179393769,12.5500057596089,-23.9413244112923));
#47636=CARTESIAN_POINT('Ctrl Pts',(3.6391299746952,12.5207396483061,-23.9552648126092));
#47637=CARTESIAN_POINT('Ctrl Pts',(3.80455199630043,12.4904455345154,-23.9697692758995));
#47638=CARTESIAN_POINT('Ctrl Pts',(3.96321409848656,12.4596117546677,-23.9845901751178));
#47639=CARTESIAN_POINT('Ctrl Pts',(4.12187620067269,12.4287779748199,-23.999411074336));
#47640=CARTESIAN_POINT('Ctrl Pts',(4.27377865463948,12.3974042624314,-24.0145485508317));
#47641=CARTESIAN_POINT('Ctrl Pts',(4.41898996525194,12.3659261737581,-24.0297825391726));
#47642=CARTESIAN_POINT('Ctrl Pts',(4.56351963026574,12.3345958483719,-24.0449450166851));
#47643=CARTESIAN_POINT('Ctrl Pts',(4.70142133579754,12.3031619818066,-24.0602033369487));
#47644=CARTESIAN_POINT('Ctrl Pts',(4.8327759042808,12.2720083557111,-24.0753672902913));
#47645=CARTESIAN_POINT('Ctrl Pts',(4.90532428615046,12.2548019106769,-24.0837424864527));
#47646=CARTESIAN_POINT('Ctrl Pts',(4.97587555827759,12.2376800953812,-24.0920893088182));
#47647=CARTESIAN_POINT('Ctrl Pts',(5.04444364113545,12.2207014823019,-24.1003786547038));
#47648=CARTESIAN_POINT('Ctrl Pts',(5.13538850289719,12.1981820015896,-24.1113731784565));
#47649=CARTESIAN_POINT('Ctrl Pts',(5.22284458178628,12.1759148649416,-24.1222663823038));
#47650=CARTESIAN_POINT('Ctrl Pts',(5.30684444827954,12.1540256279075,-24.1329957660341));
#47651=CARTESIAN_POINT('Ctrl Pts',(5.42689922171342,12.1227409663661,-24.1483304777022));
#47652=CARTESIAN_POINT('Ctrl Pts',(5.53989448945818,12.0922301987086,-24.1633298754751));
#47653=CARTESIAN_POINT('Ctrl Pts',(5.64592729865616,12.0628173208656,-24.1778362675318));
#47654=CARTESIAN_POINT('Ctrl Pts',(5.75378658155754,12.0328977899561,-24.192592540204));
#47655=CARTESIAN_POINT('Ctrl Pts',(5.85444162547483,12.0041142009824,-24.2068386546953));
#47656=CARTESIAN_POINT('Ctrl Pts',(5.94798723082197,11.9767580922063,-24.220429963577));
#47657=CARTESIAN_POINT('Ctrl Pts',(6.02496433639105,11.9542472103172,-24.2316140231032));
#47658=CARTESIAN_POINT('Ctrl Pts',(6.09712727222615,11.9327019687062,-24.242355090011));
#47659=CARTESIAN_POINT('Ctrl Pts',(6.16452420707849,11.9122610939159,-24.2525832257952));
#47660=CARTESIAN_POINT('Ctrl Pts',(6.20165893254129,11.9009984708423,-24.2582187790318));
#47661=CARTESIAN_POINT('Ctrl Pts',(6.23734668812422,11.8900707437737,-24.2636988187805));
#47662=CARTESIAN_POINT('Ctrl Pts',(6.2715947931636,11.8794983798023,-24.2690136880224));
#47663=CARTESIAN_POINT('Ctrl Pts',(-6.390311350217,11.8061921052281,-24.5118549102149));
#47664=CARTESIAN_POINT('Ctrl Pts',(-4.260207566811,12.4817967425171,-24.1870628120273));
#47665=CARTESIAN_POINT('Ctrl Pts',(0.0001663376444951,13.1582619823406,
-23.8622671604308));
#47666=CARTESIAN_POINT('Ctrl Pts',(4.2605402421,12.4817439180343,-24.1870881749925));
#47667=CARTESIAN_POINT('Ctrl Pts',(6.39081036315,11.8060338272127,-24.5119310012438));
#47668=CARTESIAN_POINT('Ctrl Pts',(-6.390311350217,11.9720498317925,-23.5459010687554));
#47669=CARTESIAN_POINT('Ctrl Pts',(-4.260207566811,12.6077623797797,-23.2652608575561));
#47670=CARTESIAN_POINT('Ctrl Pts',(0.0001663376444951,13.2461470249007,
-22.9846424253836));
#47671=CARTESIAN_POINT('Ctrl Pts',(4.2605402421,12.6077125289674,-23.2652827707593));
#47672=CARTESIAN_POINT('Ctrl Pts',(6.39081036315,11.9719008995601,-23.5459668160588));
#47673=CARTESIAN_POINT('Ctrl Pts',(-6.390311350217,12.0713623708286,-21.4528943057181));
#47674=CARTESIAN_POINT('Ctrl Pts',(-4.260207566811,12.6592430855888,-21.279241698184));
#47675=CARTESIAN_POINT('Ctrl Pts',(0.0001663376444951,13.245691316649,-21.1056360824358));
#47676=CARTESIAN_POINT('Ctrl Pts',(4.2605402421,12.6591972904408,-21.2792552548697));
#47677=CARTESIAN_POINT('Ctrl Pts',(6.39081036315,12.0712246444089,-21.4529349883696));
#47678=CARTESIAN_POINT('Ctrl Pts',(-6.390311350217,11.387980855255,-18.3168609136256));
#47679=CARTESIAN_POINT('Ctrl Pts',(-4.260207566811,12.0191856806278,-18.3050659001773));
#47680=CARTESIAN_POINT('Ctrl Pts',(0.0001663376444952,12.6510858022935,
-18.2929947474349));
#47681=CARTESIAN_POINT('Ctrl Pts',(4.2605402421,12.019136336187,-18.3050668428002));
#47682=CARTESIAN_POINT('Ctrl Pts',(6.39081036315,11.3878329790519,-18.3168636769111));
#47683=CARTESIAN_POINT('Ctrl Pts',(-6.390311350217,9.96966247179778,-15.6639900925141));
#47684=CARTESIAN_POINT('Ctrl Pts',(-4.260207566811,10.7489275346341,-15.7525652586985));
#47685=CARTESIAN_POINT('Ctrl Pts',(0.0001663376444948,11.5272506786203,
-15.8420539986973));
#47686=CARTESIAN_POINT('Ctrl Pts',(4.2605402421,10.7488667561688,-15.7525582706139));
#47687=CARTESIAN_POINT('Ctrl Pts',(6.39081036315,9.9694799086042,-15.6639693414749));
#47688=CARTESIAN_POINT('Ctrl Pts',(-6.390311350217,8.71289904002423,-14.2541069570423));
#47689=CARTESIAN_POINT('Ctrl Pts',(-4.260207566811,9.62695763387275,-14.3565480390593));
#47690=CARTESIAN_POINT('Ctrl Pts',(0.0001663376444956,10.5424016003325,
-14.4576175588418));
#47691=CARTESIAN_POINT('Ctrl Pts',(4.2605402421,9.62688614778384,-14.3565401466471));
#47692=CARTESIAN_POINT('Ctrl Pts',(6.39081036315,8.71268489794962,-14.2540829575325));
#47693=CARTESIAN_POINT('Ctrl Pts',(-6.390311350217,8.13905341860134,-13.7246653228991));
#47694=CARTESIAN_POINT('Ctrl Pts',(-4.260207566811,9.11397509263302,-13.8218701645398));
#47695=CARTESIAN_POINT('Ctrl Pts',(0.0001663376444956,10.0900092059685,
-13.9179922581859));
#47696=CARTESIAN_POINT('Ctrl Pts',(4.2605402421,9.11389887511922,-13.8218626584636));
#47697=CARTESIAN_POINT('Ctrl Pts',(6.39081036315,8.13882501775734,-13.7246425501129));
#47698=CARTESIAN_POINT('',(-6.26385954125917,8.42070865985895,-13.9442611207816));
#47699=CARTESIAN_POINT('Ctrl Pts',(-6.27159552384948,11.8794980574136,-24.2690121660567));
#47700=CARTESIAN_POINT('Ctrl Pts',(-6.27195777359891,11.9156534386679,-24.0278185403221));
#47701=CARTESIAN_POINT('Ctrl Pts',(-6.27229031327766,11.9441024445609,-23.7878332543352));
#47702=CARTESIAN_POINT('Ctrl Pts',(-6.27259314313179,11.9652318805478,-23.549555389302));
#47703=CARTESIAN_POINT('Ctrl Pts',(-6.27289863582238,11.986547111402,-23.3091823048629));
#47704=CARTESIAN_POINT('Ctrl Pts',(-6.27317389390371,12.0004135052366,-23.0705467116799));
#47705=CARTESIAN_POINT('Ctrl Pts',(-6.2734189176284,12.0072245125693,-22.8341074537603));
#47706=CARTESIAN_POINT('Ctrl Pts',(-6.2736675427985,12.014135630498,-22.5941929279593));
#47707=CARTESIAN_POINT('Ctrl Pts',(-6.27388503828953,12.0137824613635,-22.3565397318801));
#47708=CARTESIAN_POINT('Ctrl Pts',(-6.27407140436542,12.0065719181025,-22.1215733227915));
#47709=CARTESIAN_POINT('Ctrl Pts',(-6.27421804490314,12.0008983643939,-21.9366920325141));
#47710=CARTESIAN_POINT('Ctrl Pts',(-6.27434541261805,11.9909791988454,-21.7534730876361));
#47711=CARTESIAN_POINT('Ctrl Pts',(-6.27445350763872,11.9770107164655,-21.5721011929313));
#47712=CARTESIAN_POINT('Ctrl Pts',(-6.27450262997305,11.970662926741,-21.4896791646682));
#47713=CARTESIAN_POINT('Ctrl Pts',(-6.27454777225262,11.9634788985147,-21.4076383087566));
#47714=CARTESIAN_POINT('Ctrl Pts',(-6.2745889344895,11.9554821775698,-21.3259943087072));
#47715=CARTESIAN_POINT('Ctrl Pts',(-6.27470712629419,11.9325206732496,-21.0915645877277));
#47716=CARTESIAN_POINT('Ctrl Pts',(-6.27479250331386,11.9028603066983,-20.8604106389224));
#47717=CARTESIAN_POINT('Ctrl Pts',(-6.27484506554851,11.8670439026963,-20.6328684248961));
#47718=CARTESIAN_POINT('Ctrl Pts',(-6.27489762778317,11.8312274986943,-20.4053262108699));
#47719=CARTESIAN_POINT('Ctrl Pts',(-6.2749173752328,11.7892550183211,-20.1813955414873));
#47720=CARTESIAN_POINT('Ctrl Pts',(-6.27490430789742,11.7416481097758,-19.9613622676294));
#47721=CARTESIAN_POINT('Ctrl Pts',(-6.27489476776732,11.7068915134432,-19.800721555747));
#47722=CARTESIAN_POINT('Ctrl Pts',(-6.27486753874024,11.6690645752864,-19.6418696984425));
#47723=CARTESIAN_POINT('Ctrl Pts',(-6.27482283800117,11.6284224018795,-19.4852203578817));
#47724=CARTESIAN_POINT('Ctrl Pts',(-6.27477792037291,11.5875830315618,-19.3278109505361));
#47725=CARTESIAN_POINT('Ctrl Pts',(-6.27471536107492,11.5439012264961,-19.1726257824396));
#47726=CARTESIAN_POINT('Ctrl Pts',(-6.2746353804689,11.4976813102105,-19.0200578211033));
#47727=CARTESIAN_POINT('Ctrl Pts',(-6.27457691089758,11.4638923852968,-18.9085234912273));
#47728=CARTESIAN_POINT('Ctrl Pts',(-6.274509130865,11.4287479827558,-18.7983873253195));
#47729=CARTESIAN_POINT('Ctrl Pts',(-6.27443212646492,11.3923813207739,-18.6897925952231));
#47730=CARTESIAN_POINT('Ctrl Pts',(-6.2743563547694,11.3565968248678,-18.5829362750997));
#47731=CARTESIAN_POINT('Ctrl Pts',(-6.27427024762582,11.3190562081082,-18.4758583357969));
#47732=CARTESIAN_POINT('Ctrl Pts',(-6.27417380503419,11.2797074661642,-18.3686262100786));
#47733=CARTESIAN_POINT('Ctrl Pts',(-6.27399075538353,11.2050228963577,-18.1650978434006));
#47734=CARTESIAN_POINT('Ctrl Pts',(-6.27377047261781,11.1238235000032,-17.9610111481595));
#47735=CARTESIAN_POINT('Ctrl Pts',(-6.27351295673702,11.0358412016767,-17.7568354684592));
#47736=CARTESIAN_POINT('Ctrl Pts',(-6.2732582330049,10.9488128626037,-17.5548735895199));
#47737=CARTESIAN_POINT('Ctrl Pts',(-6.27296707919006,10.8551478403144,-17.3528245563033));
#47738=CARTESIAN_POINT('Ctrl Pts',(-6.27263949529251,10.754600520291,-17.1511912440502));
#47739=CARTESIAN_POINT('Ctrl Pts',(-6.27231699856497,10.6556146363325,-16.9526891691644));
#47740=CARTESIAN_POINT('Ctrl Pts',(-6.27195919444132,10.549958495229,-16.7545899618257));
#47741=CARTESIAN_POINT('Ctrl Pts',(-6.27156608292156,10.437412155432,-16.5574217276117));
#47742=CARTESIAN_POINT('Ctrl Pts',(-6.27136275152317,10.3791991458823,-16.4554392346946));
#47743=CARTESIAN_POINT('Ctrl Pts',(-6.27114997423131,10.3191430227536,-16.3537066057444));
#47744=CARTESIAN_POINT('Ctrl Pts',(-6.27092775104597,10.2572149753916,-16.2523021740491));
#47745=CARTESIAN_POINT('Ctrl Pts',(-6.27050608299771,10.1397066297922,-16.0598874683938));
#47746=CARTESIAN_POINT('Ctrl Pts',(-6.27005040567849,10.0154574689945,-15.8686514742631));
#47747=CARTESIAN_POINT('Ctrl Pts',(-6.26956071861759,9.88428240632285,-15.6791662493658));
#47748=CARTESIAN_POINT('Ctrl Pts',(-6.26938505208526,9.8372256833115,-15.6111917917125));
#47749=CARTESIAN_POINT('Ctrl Pts',(-6.26920500887961,9.78927782249918,-15.5434430983117));
#47750=CARTESIAN_POINT('Ctrl Pts',(-6.2690205889789,9.74043078877536,-15.475948142725));
#47751=CARTESIAN_POINT('Ctrl Pts',(-6.26850854175106,9.60480557636394,-15.2885464319087));
#47752=CARTESIAN_POINT('Ctrl Pts',(-6.26796275408184,9.46224623827901,-15.1030978701136));
#47753=CARTESIAN_POINT('Ctrl Pts',(-6.26738322550613,9.31269281092479,-14.9201597106969));
#47754=CARTESIAN_POINT('Ctrl Pts',(-6.26681231337191,9.16536294666898,-14.7399414791867));
#47755=CARTESIAN_POINT('Ctrl Pts',(-6.26620865619333,9.01124537325366,-14.562159540734));
#47756=CARTESIAN_POINT('Ctrl Pts',(-6.26557225352572,8.85031207893392,-14.3873873981266));
#47757=CARTESIAN_POINT('Ctrl Pts',(-6.26502584199882,8.71213571425886,-14.2373290810205));
#47758=CARTESIAN_POINT('Ctrl Pts',(-6.26445529103124,8.5689353367174,-14.0894901472568));
#47759=CARTESIAN_POINT('Ctrl Pts',(-6.26386060034155,8.42071136787207,-13.9442583527127));
#47760=CARTESIAN_POINT('Ctrl Pts',(6.26385989003177,8.42071839535226,-13.9442649557177));
#47761=CARTESIAN_POINT('Ctrl Pts',(5.97577254680956,8.54495172007927,-13.9555523998957));
#47762=CARTESIAN_POINT('Ctrl Pts',(5.6858636247251,8.66055598080169,-13.9652104797869));
#47763=CARTESIAN_POINT('Ctrl Pts',(5.39461985275565,8.76740388601456,-13.9734951213447));
#47764=CARTESIAN_POINT('Ctrl Pts',(5.12099027440223,8.86778971419429,-13.9812787143154));
#47765=CARTESIAN_POINT('Ctrl Pts',(4.8461824249731,8.96044566896363,-13.9878501532703));
#47766=CARTESIAN_POINT('Ctrl Pts',(4.5705999557957,9.04530802050967,-13.9934329340466));
#47767=CARTESIAN_POINT('Ctrl Pts',(4.31429754858432,9.12423330573478,-13.9986251371507));
#47768=CARTESIAN_POINT('Ctrl Pts',(4.05732511675319,9.19641709480444,-14.0029623014545));
#47769=CARTESIAN_POINT('Ctrl Pts',(3.80000738078161,9.26185125996808,-14.0066322166875));
#47770=CARTESIAN_POINT('Ctrl Pts',(3.5789007966154,9.31807717339948,-14.0097856814819));
#47771=CARTESIAN_POINT('Ctrl Pts',(3.35753925618122,9.36931990538708,-14.0124466098116));
#47772=CARTESIAN_POINT('Ctrl Pts',(3.13612877765637,9.41560490622071,-14.0147385401857));
#47773=CARTESIAN_POINT('Ctrl Pts',(2.89298897625723,9.46643233762966,-14.0172554016264));
#47774=CARTESIAN_POINT('Ctrl Pts',(2.64981042803868,9.51128973564011,-14.0193424104729));
#47775=CARTESIAN_POINT('Ctrl Pts',(2.40683512391639,9.55016652404637,-14.021058970814));
#47776=CARTESIAN_POINT('Ctrl Pts',(2.1674244150099,9.58847296636557,-14.0227503481728));
#47777=CARTESIAN_POINT('Ctrl Pts',(1.92821103051466,9.62097295201155,-14.0240820878113));
#47778=CARTESIAN_POINT('Ctrl Pts',(1.68942646637008,9.64770677387914,-14.0251157328352));
#47779=CARTESIAN_POINT('Ctrl Pts',(1.45224648068838,9.67426095048804,-14.0261424319974));
#47780=CARTESIAN_POINT('Ctrl Pts',(1.21548957156862,9.69512612507554,-14.0268750438104));
#47781=CARTESIAN_POINT('Ctrl Pts',(0.97938259943816,9.71039281056508,-14.0273783103472));
#47782=CARTESIAN_POINT('Ctrl Pts',(0.744965115348874,9.72555025369582,-14.0278779757079));
#47783=CARTESIAN_POINT('Ctrl Pts',(0.511188300143692,9.73518900756007,-14.0281515795311));
#47784=CARTESIAN_POINT('Ctrl Pts',(0.278274179044154,9.73944891642537,-14.028266658906));
#47785=CARTESIAN_POINT('Ctrl Pts',(0.185516959949696,9.74114540995729,-14.0283124888572));
#47786=CARTESIAN_POINT('Ctrl Pts',(0.0928965643348469,9.74198939312604,
-14.0283332223861));
#47787=CARTESIAN_POINT('Ctrl Pts',(0.000427015751061975,9.74199199953944,
-14.0283333049114));
#47788=CARTESIAN_POINT('Ctrl Pts',(0.000284677535436571,9.74199200355149,
-14.0283333050384));
#47789=CARTESIAN_POINT('Ctrl Pts',(0.000142338952074239,9.74199200557029,
-14.0283333051166));
#47790=CARTESIAN_POINT('Ctrl Pts',(1.02735216839658E-12,9.74199200559579,
-14.0283333051459));
#47791=CARTESIAN_POINT('Ctrl Pts',(-0.229753074916458,9.74199204676546,
-14.0283333524958));
#47792=CARTESIAN_POINT('Ctrl Pts',(-0.460464115169766,9.73679441031726,
-14.0282057699318));
#47793=CARTESIAN_POINT('Ctrl Pts',(-0.691907629373254,9.72624035113783,
-14.0278832023527));
#47794=CARTESIAN_POINT('Ctrl Pts',(-0.925171026103522,9.71560330346787,
-14.0275580983659));
#47795=CARTESIAN_POINT('Ctrl Pts',(-1.15917846122486,9.69952527300279,-14.0270349177334));
#47796=CARTESIAN_POINT('Ctrl Pts',(-1.39369908217627,9.6778966747267,-14.0262489641265));
#47797=CARTESIAN_POINT('Ctrl Pts',(-1.62968668811577,9.65613278417288,-14.0254580941837));
#47798=CARTESIAN_POINT('Ctrl Pts',(-1.86619392017613,9.62874872580037,-14.0244011396557));
#47799=CARTESIAN_POINT('Ctrl Pts',(-2.10298556652029,9.5956857160992,-14.0230166836363));
#47800=CARTESIAN_POINT('Ctrl Pts',(-2.34260943261476,9.56222724604067,-14.0216156684023));
#47801=CARTESIAN_POINT('Ctrl Pts',(-2.58252455733169,9.52295320564077,-14.0198792512116));
#47802=CARTESIAN_POINT('Ctrl Pts',(-2.82248718751079,9.47785596126532,-14.0177486392004));
#47803=CARTESIAN_POINT('Ctrl Pts',(-2.92697581546807,9.45821894867745,-14.016820891719));
#47804=CARTESIAN_POINT('Ctrl Pts',(-3.03147345072008,9.4374784976985,-14.0158184661558));
#47805=CARTESIAN_POINT('Ctrl Pts',(-3.13595996870217,9.41563703601003,-14.014736804792));
#47806=CARTESIAN_POINT('Ctrl Pts',(-3.39875183271366,9.36070403086545,-14.0120163408361));
#47807=CARTESIAN_POINT('Ctrl Pts',(-3.66146917368842,9.29878661121169,-14.0087759041241));
#47808=CARTESIAN_POINT('Ctrl Pts',(-3.92376785677122,9.2298478371932,-14.0048097516279));
#47809=CARTESIAN_POINT('Ctrl Pts',(-4.1932923765918,9.15900992925567,-14.0007343390696));
#47810=CARTESIAN_POINT('Ctrl Pts',(-4.46237485432196,9.0807590675398,-13.9958926176489));
#47811=CARTESIAN_POINT('Ctrl Pts',(-4.73064192361157,8.99511526164949,-13.9900702628746));
#47812=CARTESIAN_POINT('Ctrl Pts',(-5.02409522627783,8.90143079356337,-13.9837012767655));
#47813=CARTESIAN_POINT('Ctrl Pts',(-5.31657282406583,8.79890033659665,-13.9761586571199));
#47814=CARTESIAN_POINT('Ctrl Pts',(-5.60758600825935,8.68761493815447,-13.9671747121499));
#47815=CARTESIAN_POINT('Ctrl Pts',(-5.82724861853753,8.6036144789471,-13.9603934496164));
#47816=CARTESIAN_POINT('Ctrl Pts',(-6.04607687414356,8.51462738981054,-13.9527912470521));
#47817=CARTESIAN_POINT('Ctrl Pts',(-6.26386060034155,8.42071136787207,-13.9442583527127));
#47818=CARTESIAN_POINT('Ctrl Pts',(6.38290223050635,8.3687128810708,-13.9393718887612));
#47819=CARTESIAN_POINT('Ctrl Pts',(6.33185069333287,8.39190678947241,-13.9421546546274));
#47820=CARTESIAN_POINT('Ctrl Pts',(5.69974726342303,8.67523140046431,-13.9757998821803));
#47821=CARTESIAN_POINT('Ctrl Pts',(4.36985154284018,9.17370085496103,-14.0265657717891));
#47822=CARTESIAN_POINT('Ctrl Pts',(2.2815889278797,9.66167562240798,-14.0640584776628));
#47823=CARTESIAN_POINT('Ctrl Pts',(0.00160354234010209,9.84365792812771,
-14.0750234441869));
#47824=CARTESIAN_POINT('Ctrl Pts',(-2.27862803912884,9.66215989653315,-14.0640901144711));
#47825=CARTESIAN_POINT('Ctrl Pts',(-4.36746288708299,9.17445077621545,-14.026632517581));
#47826=CARTESIAN_POINT('Ctrl Pts',(-5.69840031280849,8.67579539900824,-13.9758632341147));
#47827=CARTESIAN_POINT('Ctrl Pts',(-6.33127835061241,8.39216684434521,-13.9421858490072));
#47828=CARTESIAN_POINT('Ctrl Pts',(-6.38290560157758,8.36871136134604,-13.9393716976888));
#47829=CARTESIAN_POINT('Ctrl Pts',(6.18027446328495,7.97034175760265,-13.4733537657383));
#47830=CARTESIAN_POINT('Ctrl Pts',(6.13081737426996,7.99266609326119,-13.4761866177629));
#47831=CARTESIAN_POINT('Ctrl Pts',(5.51846302072903,8.26537074194175,-13.510454637066));
#47832=CARTESIAN_POINT('Ctrl Pts',(4.23030987628035,8.7451984323429,-13.5625812544442));
#47833=CARTESIAN_POINT('Ctrl Pts',(2.2083741148917,9.21486873360186,-13.6017979517399));
#47834=CARTESIAN_POINT('Ctrl Pts',(0.00155196199890026,9.3899873070007,
-13.6135063985893));
#47835=CARTESIAN_POINT('Ctrl Pts',(-2.20550781210377,9.21533478109097,-13.601831483555));
#47836=CARTESIAN_POINT('Ctrl Pts',(-4.22799656394489,8.74592029438878,-13.562650353087));
#47837=CARTESIAN_POINT('Ctrl Pts',(-5.51715822420132,8.26591362788774,-13.5105193424603));
#47838=CARTESIAN_POINT('Ctrl Pts',(-6.13026290690437,7.99291639770159,-13.476218374096));
#47839=CARTESIAN_POINT('Ctrl Pts',(-6.18027772914287,7.97034029398681,-13.4733535718789));
#47840=CARTESIAN_POINT('Ctrl Pts',(6.17611521160237,8.03272083803512,-12.8315071320912));
#47841=CARTESIAN_POINT('Ctrl Pts',(6.1268036055389,8.05477000112189,-12.8343123479053));
#47842=CARTESIAN_POINT('Ctrl Pts',(5.51621999278854,8.32413445990068,-12.8682474805547));
#47843=CARTESIAN_POINT('Ctrl Pts',(4.2309697607976,8.79862201718509,-12.9199037439559));
#47844=CARTESIAN_POINT('Ctrl Pts',(2.21024860961346,9.26409347188965,-12.9587969182466));
#47845=CARTESIAN_POINT('Ctrl Pts',(0.00155380889916294,9.43795850846309,
-12.9704078321066));
#47846=CARTESIAN_POINT('Ctrl Pts',(-2.20738170362344,9.26455590951104,-12.9588301760772));
#47847=CARTESIAN_POINT('Ctrl Pts',(-4.22866008373731,8.79933658603706,-12.9199722536396));
#47848=CARTESIAN_POINT('Ctrl Pts',(-5.51491866660961,8.32467091068186,-12.8683115755957));
#47849=CARTESIAN_POINT('Ctrl Pts',(-6.12625076973956,8.05501722081392,-12.8343437929296));
#47850=CARTESIAN_POINT('Ctrl Pts',(-6.17611846754463,8.03271939355596,-12.8315069384015));
#47851=CARTESIAN_POINT('Ctrl Pts',(6.37205883491417,8.51110576180117,-12.4473561916133));
#47852=CARTESIAN_POINT('Ctrl Pts',(6.32135424616034,8.53365607055721,-12.4500751281646));
#47853=CARTESIAN_POINT('Ctrl Pts',(5.69347570203072,8.80916794902699,-12.4829516268409));
#47854=CARTESIAN_POINT('Ctrl Pts',(4.3705612963381,9.29513699757964,-12.5326341666895));
#47855=CARTESIAN_POINT('Ctrl Pts',(2.28550734776402,9.77326146435145,-12.5693863519979));
#47856=CARTESIAN_POINT('Ctrl Pts',(0.00160752407789911,9.95229479522915,
-12.5801293896245));
#47857=CARTESIAN_POINT('Ctrl Pts',(-2.28254561616144,9.77373725523836,-12.5694173642325));
#47858=CARTESIAN_POINT('Ctrl Pts',(-4.36818151897362,9.29586983131238,-12.5326995597546));
#47859=CARTESIAN_POINT('Ctrl Pts',(-5.69213705177152,8.80971689183168,-12.483013570555));
#47860=CARTESIAN_POINT('Ctrl Pts',(-6.32078579437215,8.53390891051175,-12.4501056035139));
#47861=CARTESIAN_POINT('Ctrl Pts',(-6.37206218235826,8.51110428680498,-12.447356000907));
#47862=CARTESIAN_POINT('',(-6.24994617759994,8.55169242034562,-12.4626545592495));
#47863=CARTESIAN_POINT('Ctrl Pts',(-6.26386065742728,8.42071151387271,-13.9442582034044));
#47864=CARTESIAN_POINT('Ctrl Pts',(-6.25434637310214,8.4015320522143,-13.9218549829862));
#47865=CARTESIAN_POINT('Ctrl Pts',(-6.24501004821117,8.38292731079581,-13.8979905814307));
#47866=CARTESIAN_POINT('Ctrl Pts',(-6.23595412983899,8.36512533432891,-13.8726812830547));
#47867=CARTESIAN_POINT('Ctrl Pts',(-6.2271258172178,8.34777078153087,-13.8480080926499));
#47868=CARTESIAN_POINT('Ctrl Pts',(-6.21856428749895,8.33117984533034,-13.8219614612362));
#47869=CARTESIAN_POINT('Ctrl Pts',(-6.21037053095467,8.31557235347761,-13.7946046387324));
#47870=CARTESIAN_POINT('Ctrl Pts',(-6.20230307295131,8.3002054354615,-13.7676694942157));
#47871=CARTESIAN_POINT('Ctrl Pts',(-6.19459246438177,8.28579263233555,-13.7394641191199));
#47872=CARTESIAN_POINT('Ctrl Pts',(-6.18733649965018,8.27254147840909,-13.710099095204));
#47873=CARTESIAN_POINT('Ctrl Pts',(-6.18020802747487,8.25952315685577,-13.6812500360294));
#47874=CARTESIAN_POINT('Ctrl Pts',(-6.17351870157481,8.24762677503362,-13.6512818652735));
#47875=CARTESIAN_POINT('Ctrl Pts',(-6.16735769517278,8.23703574837833,-13.6203480581767));
#47876=CARTESIAN_POINT('Ctrl Pts',(-6.16655851772455,8.23566192905334,-13.6163354668229));
#47877=CARTESIAN_POINT('Ctrl Pts',(-6.16576822066994,8.23431004579379,-13.6123066933628));
#47878=CARTESIAN_POINT('Ctrl Pts',(-6.16498698947291,8.23298047175863,-13.6082621310938));
#47879=CARTESIAN_POINT('Ctrl Pts',(-6.15905579130535,8.22288619094789,-13.577555343642));
#47880=CARTESIAN_POINT('Ctrl Pts',(-6.1536480685766,8.21408021951287,-13.5459350859393));
#47881=CARTESIAN_POINT('Ctrl Pts',(-6.14883841710609,8.20671036772986,-13.5135971977432));
#47882=CARTESIAN_POINT('Ctrl Pts',(-6.14409038200413,8.1994349310009,-13.4816735897188));
#47883=CARTESIAN_POINT('Ctrl Pts',(-6.13992546528859,8.19355960821916,-13.4490512054137));
#47884=CARTESIAN_POINT('Ctrl Pts',(-6.13640216930785,8.18919262766077,-13.4159537386902));
#47885=CARTESIAN_POINT('Ctrl Pts',(-6.1328995619996,8.18485128986162,-13.3830506191498));
#47886=CARTESIAN_POINT('Ctrl Pts',(-6.13003128219596,8.18200105235029,-13.3496786993339));
#47887=CARTESIAN_POINT('Ctrl Pts',(-6.12783791167436,8.18070711233178,-13.316083169479));
#47888=CARTESIAN_POINT('Ctrl Pts',(-6.12565198276521,8.17941756236048,-13.2826016216944));
#47889=CARTESIAN_POINT('Ctrl Pts',(-6.12413653007737,8.17967399136537,-13.248898808936));
#47890=CARTESIAN_POINT('Ctrl Pts',(-6.12331218772028,8.18149509393478,-13.2152311285308));
#47891=CARTESIAN_POINT('Ctrl Pts',(-6.12248858712431,8.18331455783663,-13.1815937430341));
#47892=CARTESIAN_POINT('Ctrl Pts',(-6.12235489834618,8.1866958860133,-13.1479923024839));
#47893=CARTESIAN_POINT('Ctrl Pts',(-6.12291077007659,8.19161012802485,-13.1146833589572));
#47894=CARTESIAN_POINT('Ctrl Pts',(-6.12346935064114,8.19654831776705,-13.0812120966831));
#47895=CARTESIAN_POINT('Ctrl Pts',(-6.12472418546194,8.20303420465641,-13.0480370555447));
#47896=CARTESIAN_POINT('Ctrl Pts',(-6.12665372884193,8.21099167735592,-13.0154062086923));
#47897=CARTESIAN_POINT('Ctrl Pts',(-6.12859073792394,8.21897993874907,-12.9826491080424));
#47898=CARTESIAN_POINT('Ctrl Pts',(-6.13120753526199,8.22845076770164,-12.9504411865254));
#47899=CARTESIAN_POINT('Ctrl Pts',(-6.1344625045572,8.23928490573034,-12.9190085043198));
#47900=CARTESIAN_POINT('Ctrl Pts',(-6.13775487193949,8.25024352297854,-12.8872146751788));
#47901=CARTESIAN_POINT('Ctrl Pts',(-6.14169993700211,8.26259637936795,-12.8562146498089));
#47902=CARTESIAN_POINT('Ctrl Pts',(-6.14623721161599,8.27618448987975,-12.8262061973638));
#47903=CARTESIAN_POINT('Ctrl Pts',(-6.14954105285304,8.28607874660054,-12.8043553791778));
#47904=CARTESIAN_POINT('Ctrl Pts',(-6.15315850171545,8.29662715152438,-12.7830295350418));
#47905=CARTESIAN_POINT('Ctrl Pts',(-6.15706167140227,8.30775960757765,-12.7622906844641));
#47906=CARTESIAN_POINT('Ctrl Pts',(-6.16251763550829,8.32332087841957,-12.7333013159685));
#47907=CARTESIAN_POINT('Ctrl Pts',(-6.16853202930593,8.34002353013777,-12.7054609962895));
#47908=CARTESIAN_POINT('Ctrl Pts',(-6.17501884145997,8.35766197049687,-12.6788966167709));
#47909=CARTESIAN_POINT('Ctrl Pts',(-6.1816540436465,8.37570390161165,-12.6517245598528));
#47910=CARTESIAN_POINT('Ctrl Pts',(-6.18878317295267,8.39472411391086,-12.6258875792879));
#47911=CARTESIAN_POINT('Ctrl Pts',(-6.19630866220191,8.41449602201175,-12.6014675769469));
#47912=CARTESIAN_POINT('Ctrl Pts',(-6.20394561629464,8.43456078451306,-12.5766858743034));
#47913=CARTESIAN_POINT('Ctrl Pts',(-6.21199040546579,8.45539889874646,-12.5533631997356));
#47914=CARTESIAN_POINT('Ctrl Pts',(-6.22034090105188,8.47677914867427,-12.5315314734822));
#47915=CARTESIAN_POINT('Ctrl Pts',(-6.22889165472525,8.49867213080004,-12.5091761879146));
#47916=CARTESIAN_POINT('Ctrl Pts',(-6.23776262655085,8.52113286412999,-12.4883838248286));
#47917=CARTESIAN_POINT('Ctrl Pts',(-6.24684926282979,8.54393035742536,-12.4691375394487));
#47918=CARTESIAN_POINT('Ctrl Pts',(-6.24787884759462,8.54651348621501,-12.4669567894331));
#47919=CARTESIAN_POINT('Ctrl Pts',(-6.24891120939786,8.54910096258273,-12.4647958402509));
#47920=CARTESIAN_POINT('Ctrl Pts',(-6.24994620285641,8.55169246976548,-12.4626546312706));
#47921=CARTESIAN_POINT('Ctrl Pts',(6.24994600986387,8.55169427781047,-12.4626534555308));
#47922=CARTESIAN_POINT('Ctrl Pts',(6.23834714732467,8.55674697036125,-12.4632538750115));
#47923=CARTESIAN_POINT('Ctrl Pts',(6.2267385857704,8.56178829857455,-12.4638514563262));
#47924=CARTESIAN_POINT('Ctrl Pts',(6.21512033143819,8.56681821124616,-12.4644462123286));
#47925=CARTESIAN_POINT('Ctrl Pts',(5.96034508265897,8.67711853826633,-12.4774885424538));
#47926=CARTESIAN_POINT('Ctrl Pts',(5.70090661232431,8.78193286041189,-12.4891713191083));
#47927=CARTESIAN_POINT('Ctrl Pts',(5.43691813523151,8.88068309765021,-12.4996529176594));
#47928=CARTESIAN_POINT('Ctrl Pts',(5.2551888702222,8.9486626103564,-12.506868434116));
#47929=CARTESIAN_POINT('Ctrl Pts',(5.07130391006201,9.01376755359675,-12.5135149435913));
#47930=CARTESIAN_POINT('Ctrl Pts',(4.88530796602069,9.07579763495134,-12.5196473374325));
#47931=CARTESIAN_POINT('Ctrl Pts',(4.73779955267249,9.1249920350101,-12.5245107751285));
#47932=CARTESIAN_POINT('Ctrl Pts',(4.58896565423665,9.17225657896646,-12.529047255444));
#47933=CARTESIAN_POINT('Ctrl Pts',(4.4388298703262,9.21750139379221,-12.5332750896649));
#47934=CARTESIAN_POINT('Ctrl Pts',(4.35054152314884,9.24410790834369,-12.535761295723));
#47935=CARTESIAN_POINT('Ctrl Pts',(4.26180298671814,9.27001589812941,-12.5381407888862));
#47936=CARTESIAN_POINT('Ctrl Pts',(4.17262217431499,9.29520771022481,-12.540416752993));
#47937=CARTESIAN_POINT('Ctrl Pts',(4.05220505027363,9.32922316130868,-12.5434898922118));
#47938=CARTESIAN_POINT('Ctrl Pts',(3.93097978551739,9.36193304379587,-12.5463746310616));
#47939=CARTESIAN_POINT('Ctrl Pts',(3.80896296004634,9.39329538834622,-12.5490775242258));
#47940=CARTESIAN_POINT('Ctrl Pts',(3.74795454731081,9.4089765606214,-12.5504289708079));
#47941=CARTESIAN_POINT('Ctrl Pts',(3.68674824151337,9.42432084095514,-12.5517349456858));
#47942=CARTESIAN_POINT('Ctrl Pts',(3.62534627981748,9.43932314297662,-12.5529960128517));
#47943=CARTESIAN_POINT('Ctrl Pts',(3.59464529896954,9.44682429398735,-12.5536265464346));
#47944=CARTESIAN_POINT('Ctrl Pts',(3.56389540398993,9.45423994993378,-12.5542458524347));
#47945=CARTESIAN_POINT('Ctrl Pts',(3.53309687884755,9.46156947861001,-12.5548539913524));
#47946=CARTESIAN_POINT('Ctrl Pts',(3.51769761627636,9.46523424294812,-12.5551580608113));
#47947=CARTESIAN_POINT('Ctrl Pts',(3.50228619615571,9.46887747543691,-12.5554593384574));
#47948=CARTESIAN_POINT('Ctrl Pts',(3.48686265457938,9.47249909762948,-12.5557578308906));
#47949=CARTESIAN_POINT('Ctrl Pts',(3.47297546939743,9.47575996594551,-12.5560265901554));
#47950=CARTESIAN_POINT('Ctrl Pts',(3.46073395674727,9.47861878456373,-12.5562615773165));
#47951=CARTESIAN_POINT('Ctrl Pts',(3.44566639845783,9.4821143160989,-12.5565479383032));
#47952=CARTESIAN_POINT('Ctrl Pts',(3.44399945593332,9.48250103105628,-12.5565796187717));
#47953=CARTESIAN_POINT('Ctrl Pts',(3.4422979120268,9.48289548860676,-12.5566119220753));
#47954=CARTESIAN_POINT('Ctrl Pts',(3.44055570174106,9.48329905498223,-12.5566449587627));
#47955=CARTESIAN_POINT('Ctrl Pts',(3.14723349105595,9.55124434400876,-12.5622070853754));
#47956=CARTESIAN_POINT('Ctrl Pts',(2.85165500750086,9.61079217192647,-12.5667997901614));
#47957=CARTESIAN_POINT('Ctrl Pts',(2.55408711751812,9.66164092414786,-12.5705995014848));
#47958=CARTESIAN_POINT('Ctrl Pts',(2.47950005199353,9.67438644993023,-12.5715519205024));
#47959=CARTESIAN_POINT('Ctrl Pts',(2.40478795778839,9.68658517669469,-12.5724545017186));
#47960=CARTESIAN_POINT('Ctrl Pts',(2.32995497501033,9.69823183993254,-12.573309998081));
#47961=CARTESIAN_POINT('Ctrl Pts',(2.03343027723976,9.74438158792375,-12.5766998910251));
#47962=CARTESIAN_POINT('Ctrl Pts',(1.73500731960175,9.78186721768321,-12.5793506939259));
#47963=CARTESIAN_POINT('Ctrl Pts',(1.4350481173723,9.81050424466312,-12.5813273931514));
#47964=CARTESIAN_POINT('Ctrl Pts',(1.1412105272793,9.83855684292536,-12.5832637516042));
#47965=CARTESIAN_POINT('Ctrl Pts',(0.845898280575693,9.85811831741548,-12.5845531625828));
#47966=CARTESIAN_POINT('Ctrl Pts',(0.549457528734541,9.86896603464892,-12.5852549836228));
#47967=CARTESIAN_POINT('Ctrl Pts',(0.367266766940093,9.8756329785634,-12.5856863187518));
#47968=CARTESIAN_POINT('Ctrl Pts',(0.184649881599701,9.87900754648283,-12.5858956765151));
#47969=CARTESIAN_POINT('Ctrl Pts',(0.00168954384257825,9.87902850122962,
-12.5858966915729));
#47970=CARTESIAN_POINT('Ctrl Pts',(0.00126856427520073,9.8790285494451,
-12.5858966939085));
#47971=CARTESIAN_POINT('Ctrl Pts',(0.000847582890492026,9.87902857990227,
-12.585896695141));
#47972=CARTESIAN_POINT('Ctrl Pts',(0.000426599689475151,9.87902859260107,
-12.5858966952703));
#47973=CARTESIAN_POINT('Ctrl Pts',(-0.295036707193534,9.87903750513702,
-12.5858967859643));
#47974=CARTESIAN_POINT('Ctrl Pts',(-0.589594666757916,9.87037163946821,
-12.5852999029506));
#47975=CARTESIAN_POINT('Ctrl Pts',(-0.88292067783907,9.85320318925631,-12.5841083605291));
#47976=CARTESIAN_POINT('Ctrl Pts',(-1.16919227118,9.83644763600947,-12.5829454744071));
#47977=CARTESIAN_POINT('Ctrl Pts',(-1.45429085808452,9.81159306700723,-12.581216271102));
#47978=CARTESIAN_POINT('Ctrl Pts',(-1.73790621418847,9.77875217866173,-12.5789214638339));
#47979=CARTESIAN_POINT('Ctrl Pts',(-1.93498547871474,9.75593162969559,-12.5773268430953));
#47980=CARTESIAN_POINT('Ctrl Pts',(-2.13135422339377,9.72927182221161,-12.5754444582432));
#47981=CARTESIAN_POINT('Ctrl Pts',(-2.32690904026969,9.69884145796004,-12.5732400127974));
#47982=CARTESIAN_POINT('Ctrl Pts',(-2.41624320815342,9.68494013191632,-12.5722329688253));
#47983=CARTESIAN_POINT('Ctrl Pts',(-2.50540756274993,9.6702518021163,-12.5711587074841));
#47984=CARTESIAN_POINT('Ctrl Pts',(-2.5943952822042,9.65478713090383,-12.5700110627634));
#47985=CARTESIAN_POINT('Ctrl Pts',(-2.73628735805807,9.6301285115551,-12.5681811283324));
#47986=CARTESIAN_POINT('Ctrl Pts',(-2.87772704193816,9.60349283140064,-12.5661676436363));
#47987=CARTESIAN_POINT('Ctrl Pts',(-3.01867923181154,9.57491812838071,-12.5639494070577));
#47988=CARTESIAN_POINT('Ctrl Pts',(-3.08915532674823,9.56063077687074,-12.5628402887685));
#47989=CARTESIAN_POINT('Ctrl Pts',(-3.15950954702942,9.54585865784176,-12.5616799674469));
#47990=CARTESIAN_POINT('Ctrl Pts',(-3.2297376354622,9.53060698018096,-12.5604652815848));
#47991=CARTESIAN_POINT('Ctrl Pts',(-3.26485167967859,9.52298114135057,-12.5598579386538));
#47992=CARTESIAN_POINT('Ctrl Pts',(-3.29993419083247,9.51523541215242,-12.5592370036778));
#47993=CARTESIAN_POINT('Ctrl Pts',(-3.33498464004132,9.50737045297991,-12.5586020651489));
#47994=CARTESIAN_POINT('Ctrl Pts',(-3.35250986464574,9.50343797339365,-12.5582845958845));
#47995=CARTESIAN_POINT('Ctrl Pts',(-3.37002707375541,9.49947568627104,-12.5579636256764));
#47996=CARTESIAN_POINT('Ctrl Pts',(-3.38753620170862,9.49548367571953,-12.5576391012899));
#47997=CARTESIAN_POINT('Ctrl Pts',(-3.40305444461023,9.49194557892969,-12.5573514771278));
#47998=CARTESIAN_POINT('Ctrl Pts',(-3.42017127190382,9.48801362514177,-12.557030768135));
#47999=CARTESIAN_POINT('Ctrl Pts',(-3.43461926460173,9.48467283034959,-12.5567574607883));
#48000=CARTESIAN_POINT('Ctrl Pts',(-3.43647284382912,9.4842442290927,-12.556722397314));
#48001=CARTESIAN_POINT('Ctrl Pts',(-3.43828251345007,9.48382542630385,-12.5566881220856));
#48002=CARTESIAN_POINT('Ctrl Pts',(-3.44003927655192,9.48341855825448,-12.556654811709));
#48003=CARTESIAN_POINT('Ctrl Pts',(-3.71842562677252,9.41894400777795,-12.5513762660949));
#48004=CARTESIAN_POINT('Ctrl Pts',(-3.99291251944306,9.34736366168737,-12.5452387374728));
#48005=CARTESIAN_POINT('Ctrl Pts',(-4.26326703213689,9.26922774175394,-12.5381261540744));
#48006=CARTESIAN_POINT('Ctrl Pts',(-4.32118012884348,9.25249011439838,-12.5366025555737));
#48007=CARTESIAN_POINT('Ctrl Pts',(-4.37890370453842,9.23545151592402,-12.5350342529378));
#48008=CARTESIAN_POINT('Ctrl Pts',(-4.43643562971827,9.21811709981191,-12.5334201657359));
#48009=CARTESIAN_POINT('Ctrl Pts',(-4.71170121329105,9.13517935434142,-12.52569745084));
#48010=CARTESIAN_POINT('Ctrl Pts',(-4.9825779915345,9.04547352247087,-12.5169256906687));
#48011=CARTESIAN_POINT('Ctrl Pts',(-5.24893249317413,8.94957453395467,-12.5069723932165));
#48012=CARTESIAN_POINT('Ctrl Pts',(-5.52135149042552,8.85149206818748,-12.4967924739937));
#48013=CARTESIAN_POINT('Ctrl Pts',(-5.78904005213231,8.74693116129152,-12.4853766661013));
#48014=CARTESIAN_POINT('Ctrl Pts',(-6.05187470201982,8.6364575226633,-12.4725949241842));
#48015=CARTESIAN_POINT('Ctrl Pts',(-6.10592217001445,8.61374050095188,-12.4699665767138));
#48016=CARTESIAN_POINT('Ctrl Pts',(-6.15976445112939,8.5907732983932,-12.4672805075813));
#48017=CARTESIAN_POINT('Ctrl Pts',(-6.21340056281147,8.56756058651678,-12.4645356415522));
#48018=CARTESIAN_POINT('Ctrl Pts',(-6.22559309888096,8.5622838836025,-12.4639116798776));
#48019=CARTESIAN_POINT('Ctrl Pts',(-6.23777498143661,8.55699449386147,-12.4632846799959));
#48020=CARTESIAN_POINT('Ctrl Pts',(-6.24994620285641,8.55169246976548,-12.4626546312706));
#48021=CARTESIAN_POINT('Ctrl Pts',(-6.25018914864656,8.43438870834341,-13.9525601584504));
#48022=CARTESIAN_POINT('Ctrl Pts',(-6.29333242017986,8.41575013829568,-13.9497867189065));
#48023=CARTESIAN_POINT('Ctrl Pts',(-6.42498143684504,8.35057692490983,-13.9456631289492));
#48024=CARTESIAN_POINT('Ctrl Pts',(-6.63295097649907,8.20289362203243,-13.9624206396854));
#48025=CARTESIAN_POINT('Ctrl Pts',(-6.84635576793911,7.97012311971574,-14.0212942505881));
#48026=CARTESIAN_POINT('Ctrl Pts',(-7.00591486456679,7.69498486605711,-14.116453013348));
#48027=CARTESIAN_POINT('Ctrl Pts',(-7.09166336529848,7.41671876496553,-14.2329315229147));
#48028=CARTESIAN_POINT('Ctrl Pts',(-7.10675912386536,7.23705082250496,-14.3187568141423));
#48029=CARTESIAN_POINT('Ctrl Pts',(-7.10558341805161,7.15962818133564,-14.3578004370417));
#48030=CARTESIAN_POINT('Ctrl Pts',(-6.05187975179145,8.02971242238399,-13.49040582652));
#48031=CARTESIAN_POINT('Ctrl Pts',(-6.09005575691405,8.01339292600982,-13.487733176703));
#48032=CARTESIAN_POINT('Ctrl Pts',(-6.20676090005671,7.95627696143004,-13.4832682945061));
#48033=CARTESIAN_POINT('Ctrl Pts',(-6.39210913002687,7.82639664193588,-13.4962238277183));
#48034=CARTESIAN_POINT('Ctrl Pts',(-6.58337525180673,7.6207808979233,-13.545973170834));
#48035=CARTESIAN_POINT('Ctrl Pts',(-6.72695588659178,7.37705576592004,-13.628332337738));
#48036=CARTESIAN_POINT('Ctrl Pts',(-6.80424094438363,7.13044673300983,-13.7304209520421));
#48037=CARTESIAN_POINT('Ctrl Pts',(-6.81779957153361,6.97168361388838,-13.8060530499948));
#48038=CARTESIAN_POINT('Ctrl Pts',(-6.8167458887583,6.90348311857466,-13.8404623489865));
#48039=CARTESIAN_POINT('Ctrl Pts',(-6.03996297048261,8.08823314275827,-12.8475667646262));
#48040=CARTESIAN_POINT('Ctrl Pts',(-6.09254474875977,8.06608626798415,-12.8440967086183));
#48041=CARTESIAN_POINT('Ctrl Pts',(-6.25234888527267,7.98904341043708,-12.8387609712559));
#48042=CARTESIAN_POINT('Ctrl Pts',(-6.50181215036969,7.81693078662947,-12.8579363116836));
#48043=CARTESIAN_POINT('Ctrl Pts',(-6.75454537743524,7.54979157659601,-12.9254977297776));
#48044=CARTESIAN_POINT('Ctrl Pts',(-6.94177187240725,7.23734865246623,-13.0337722950875));
#48045=CARTESIAN_POINT('Ctrl Pts',(-7.04201525985038,6.9229090033521,-13.1655797489763));
#48046=CARTESIAN_POINT('Ctrl Pts',(-7.05980554193481,6.71930667450342,-13.2628609438922));
#48047=CARTESIAN_POINT('Ctrl Pts',(-7.05841299846996,6.63112648395583,-13.3073277280787));
#48048=CARTESIAN_POINT('Ctrl Pts',(-6.22264956594464,8.57067337177415,-12.4592145762074));
#48049=CARTESIAN_POINT('Ctrl Pts',(-6.29926973334839,8.53849259776433,-12.4545882139428));
#48050=CARTESIAN_POINT('Ctrl Pts',(-6.53107452795,8.42701132075841,-12.4484413705606));
#48051=CARTESIAN_POINT('Ctrl Pts',(-6.8880383586651,8.18118390664653,-12.4796540523942));
#48052=CARTESIAN_POINT('Ctrl Pts',(-7.24428436794399,7.80543742918326,-12.579922561284));
#48053=CARTESIAN_POINT('Ctrl Pts',(-7.50527072104853,7.37060329974535,-12.7353078198852));
#48054=CARTESIAN_POINT('Ctrl Pts',(-7.6443714140547,6.93470257276648,-12.9208516737137));
#48055=CARTESIAN_POINT('Ctrl Pts',(-7.66930097473565,6.65083078671604,-13.0569883447064));
#48056=CARTESIAN_POINT('Ctrl Pts',(-7.66733780264737,6.52697650901137,-13.1194049655982));
#48057=CARTESIAN_POINT('',(-7.00000855064648,6.97711954492367,-13.9487143138293));
#48058=CARTESIAN_POINT('',(-7.00000022782178,8.04447854521813,-12.5220639276637));
#48059=CARTESIAN_POINT('Ctrl Pts',(-7.,6.97711954482011,-13.9487143139614));
#48060=CARTESIAN_POINT('Ctrl Pts',(-7.,7.0212653751252,-13.8464534547224));
#48061=CARTESIAN_POINT('Ctrl Pts',(-7.,7.0628914752741,-13.7557906231791));
#48062=CARTESIAN_POINT('Ctrl Pts',(-7.,7.10101355047009,-13.67816421703));
#48063=CARTESIAN_POINT('Ctrl Pts',(-7.,7.12007458806808,-13.6393510139554));
#48064=CARTESIAN_POINT('Ctrl Pts',(-7.,7.13821566025969,-13.6037726540019));
#48065=CARTESIAN_POINT('Ctrl Pts',(-7.,7.15514766559505,-13.5714749226967));
#48066=CARTESIAN_POINT('Ctrl Pts',(-7.,7.16361366826273,-13.5553260570441));
#48067=CARTESIAN_POINT('Ctrl Pts',(-7.,7.17177624969455,-13.5399962417611));
#48068=CARTESIAN_POINT('Ctrl Pts',(-7.,7.17959497271063,-13.5254856024994));
#48069=CARTESIAN_POINT('Ctrl Pts',(-7.,7.18350433421868,-13.5182302828686));
#48070=CARTESIAN_POINT('Ctrl Pts',(-7.,7.18732773112278,-13.5111797572431));
#48071=CARTESIAN_POINT('Ctrl Pts',(-7.,7.19106003063175,-13.5043337119964));
#48072=CARTESIAN_POINT('Ctrl Pts',(-7.,7.19292618038623,-13.5009106893731));
#48073=CARTESIAN_POINT('Ctrl Pts',(-7.,7.19476955579192,-13.4975387868444));
#48074=CARTESIAN_POINT('Ctrl Pts',(-7.,7.19658952368337,-13.4942179595918));
#48075=CARTESIAN_POINT('Ctrl Pts',(-7.,7.19840949157481,-13.4908971323391));
#48076=CARTESIAN_POINT('Ctrl Pts',(-7.,7.19937899854009,-13.4891292310517));
#48077=CARTESIAN_POINT('Ctrl Pts',(-7.,7.20197857287697,-13.4844086544396));
#48078=CARTESIAN_POINT('Ctrl Pts',(-7.,7.24357176226704,-13.4088794286459));
#48079=CARTESIAN_POINT('Ctrl Pts',(-7.,7.28584553318823,-13.3376348089185));
#48080=CARTESIAN_POINT('Ctrl Pts',(-7.,7.328409342137,-13.2711767253503));
#48081=CARTESIAN_POINT('Ctrl Pts',(-7.,7.37097315108578,-13.2047186417821));
#48082=CARTESIAN_POINT('Ctrl Pts',(-7.,7.41284927480191,-13.1443363888025));
#48083=CARTESIAN_POINT('Ctrl Pts',(-7.,7.45600956171151,-13.0863542604578));
#48084=CARTESIAN_POINT('Ctrl Pts',(-7.,7.54233013553071,-12.9703900037684));
#48085=CARTESIAN_POINT('Ctrl Pts',(-7.,7.63589384217129,-12.8624384607559));
#48086=CARTESIAN_POINT('Ctrl Pts',(-7.,7.73524795321228,-12.7671719736965));
#48087=CARTESIAN_POINT('Ctrl Pts',(-7.,7.83460206425328,-12.6719054866371));
#48088=CARTESIAN_POINT('Ctrl Pts',(-7.,7.93956557936649,-12.5894601405347));
#48089=CARTESIAN_POINT('Ctrl Pts',(-7.,8.04447792928004,-12.5220637837759));
#48090=CARTESIAN_POINT('Ctrl Pts',(-6.249946127087,8.5516923215059,-12.4626544152073));
#48091=CARTESIAN_POINT('Ctrl Pts',(-6.343321450661,8.51101931861056,-12.4578186829295));
#48092=CARTESIAN_POINT('Ctrl Pts',(-6.523278504857,8.41889547577619,-12.4561262975012));
#48093=CARTESIAN_POINT('Ctrl Pts',(-6.77486797283079,8.24886074280407,-12.4762415338865));
#48094=CARTESIAN_POINT('Ctrl Pts',(-6.92747242449811,8.11608195573808,-12.5042843754154));
#48095=CARTESIAN_POINT('Ctrl Pts',(-7.00000066044537,8.04447888856054,-12.5220635455847));
#48096=CARTESIAN_POINT('Ctrl Pts',(-6.26385630696103,8.42070038979626,-13.9442695742879));
#48097=CARTESIAN_POINT('Ctrl Pts',(-6.29796810587027,8.39841656325678,-13.9355204336375));
#48098=CARTESIAN_POINT('Ctrl Pts',(-6.33179731289198,8.3741284883213,-13.9274976168449));
#48099=CARTESIAN_POINT('Ctrl Pts',(-6.36511664972141,8.34783587785705,-13.9202482699668));
#48100=CARTESIAN_POINT('Ctrl Pts',(-6.40970979856333,8.31264699346006,-13.9105460599258));
#48101=CARTESIAN_POINT('Ctrl Pts',(-6.45339109876207,8.2738663583666,-13.9022291972004));
#48102=CARTESIAN_POINT('Ctrl Pts',(-6.49565120757311,8.23161769795669,-13.8953353174991));
#48103=CARTESIAN_POINT('Ctrl Pts',(-6.51581268517414,8.21146168216562,-13.892046381311));
#48104=CARTESIAN_POINT('Ctrl Pts',(-6.53565002992448,8.19051657626437,-13.8890814791457));
#48105=CARTESIAN_POINT('Ctrl Pts',(-6.55510400910515,8.16879693701786,-13.8864458658826));
#48106=CARTESIAN_POINT('Ctrl Pts',(-6.56563072135863,8.15704425698905,-13.8850197133112));
#48107=CARTESIAN_POINT('Ctrl Pts',(-6.5760451534477,8.14506479690131,-13.8836899976213));
#48108=CARTESIAN_POINT('Ctrl Pts',(-6.58633757720893,8.13286091933527,-13.8824576824069));
#48109=CARTESIAN_POINT('Ctrl Pts',(-6.620385417617,8.09248989639961,-13.8783811235005));
#48110=CARTESIAN_POINT('Ctrl Pts',(-6.65310005362638,8.04966218117982,-13.8753698816525));
#48111=CARTESIAN_POINT('Ctrl Pts',(-6.68417663523944,8.00453222416122,-13.8734110619505));
#48112=CARTESIAN_POINT('Ctrl Pts',(-6.70441204256171,7.97514601064269,-13.8721355833592));
#48113=CARTESIAN_POINT('Ctrl Pts',(-6.72395244136366,7.94478389648954,-13.8713064535031));
#48114=CARTESIAN_POINT('Ctrl Pts',(-6.74270685114769,7.91349062623327,-13.8709224019828));
#48115=CARTESIAN_POINT('Ctrl Pts',(-6.75208405603971,7.89784399110514,-13.8707303762227));
#48116=CARTESIAN_POINT('Ctrl Pts',(-6.7612647072571,7.8819645336667,-13.870649656644));
#48117=CARTESIAN_POINT('Ctrl Pts',(-6.77023679072211,7.86585803887211,-13.8706803006051));
#48118=CARTESIAN_POINT('Ctrl Pts',(-6.77026987473812,7.86579864714513,-13.8706804136029));
#48119=CARTESIAN_POINT('Ctrl Pts',(-6.77030295591783,7.86573925233098,-13.8706805281151));
#48120=CARTESIAN_POINT('Ctrl Pts',(-6.77033603426063,7.86567985442995,-13.8706806441417));
#48121=CARTESIAN_POINT('Ctrl Pts',(-6.77478822838955,7.8576851677607,-13.8706962607982));
#48122=CARTESIAN_POINT('Ctrl Pts',(-6.77918903097313,7.84963455861528,-13.8707393125092));
#48123=CARTESIAN_POINT('Ctrl Pts',(-6.78353730413754,7.84152899674416,-13.870809592925));
#48124=CARTESIAN_POINT('Ctrl Pts',(-6.7857275938418,7.83744610497488,-13.8708449942132));
#48125=CARTESIAN_POINT('Ctrl Pts',(-6.78790455515289,7.83334927001429,-13.8708873043198));
#48126=CARTESIAN_POINT('Ctrl Pts',(-6.79006804053141,7.82923861688294,-13.8709364975064));
#48127=CARTESIAN_POINT('Ctrl Pts',(-6.7918685580019,7.82581760796298,-13.8709774375529));
#48128=CARTESIAN_POINT('Ctrl Pts',(-6.79402626678841,7.82168086079407,-13.8710331174161));
#48129=CARTESIAN_POINT('Ctrl Pts',(-6.79562563784836,7.81859131291439,-13.8710788063686));
#48130=CARTESIAN_POINT('Ctrl Pts',(-6.79594805647374,7.81796848822701,-13.8710880168449));
#48131=CARTESIAN_POINT('Ctrl Pts',(-6.79624792436415,7.81738830838156,-13.8710967474167));
#48132=CARTESIAN_POINT('Ctrl Pts',(-6.79651792025364,7.81686532799675,-13.8711047010087));
#48133=CARTESIAN_POINT('Ctrl Pts',(-6.81286579182502,7.78519960085733,-13.8715862798252));
#48134=CARTESIAN_POINT('Ctrl Pts',(-6.82902715496191,7.75152418985998,-13.8724615233629));
#48135=CARTESIAN_POINT('Ctrl Pts',(-6.84471562482565,7.71578378911281,-13.8738230072937));
#48136=CARTESIAN_POINT('Ctrl Pts',(-6.85958196904654,7.68191629886587,-13.8751131451428));
#48137=CARTESIAN_POINT('Ctrl Pts',(-6.87402383564703,7.64619448323108,-13.8768398510351));
#48138=CARTESIAN_POINT('Ctrl Pts',(-6.88775763634137,7.60859545149307,-13.8790826824863));
#48139=CARTESIAN_POINT('Ctrl Pts',(-6.89385972568219,7.59188975902672,-13.8800791989056));
#48140=CARTESIAN_POINT('Ctrl Pts',(-6.89982147569496,7.57481381720393,-13.88117762011));
#48141=CARTESIAN_POINT('Ctrl Pts',(-6.90561511753872,7.55736734222936,-13.8823850238945));
#48142=CARTESIAN_POINT('Ctrl Pts',(-6.91636947920041,7.52498258206334,-13.8846262492447));
#48143=CARTESIAN_POINT('Ctrl Pts',(-6.92654558933561,7.49131984950804,-13.887243193891));
#48144=CARTESIAN_POINT('Ctrl Pts',(-6.93597071590286,7.45640380866853,-13.8902697151454));
#48145=CARTESIAN_POINT('Ctrl Pts',(-6.9464108772029,7.41772750063998,-13.8936221762342));
#48146=CARTESIAN_POINT('Ctrl Pts',(-6.95593049190132,7.37751271587397,-13.8974771800602));
#48147=CARTESIAN_POINT('Ctrl Pts',(-6.96426462120672,7.33582224075069,-13.9018779416159));
#48148=CARTESIAN_POINT('Ctrl Pts',(-6.97143755969684,7.29994048241401,-13.9056655468704));
#48149=CARTESIAN_POINT('Ctrl Pts',(-6.97773208677669,7.26296598840208,-13.9098573515925));
#48150=CARTESIAN_POINT('Ctrl Pts',(-6.98295592997464,7.22495918651961,-13.9144796278969));
#48151=CARTESIAN_POINT('Ctrl Pts',(-6.98861460540534,7.1837887019047,-13.9194866620605));
#48152=CARTESIAN_POINT('Ctrl Pts',(-6.99301684031462,7.14140573016511,-13.924999197015));
#48153=CARTESIAN_POINT('Ctrl Pts',(-6.99593359400257,7.09794539883662,-13.9310276109909));
#48154=CARTESIAN_POINT('Ctrl Pts',(-6.99857998209795,7.05851357985103,-13.9364972271074));
#48155=CARTESIAN_POINT('Ctrl Pts',(-7.00000359100067,7.01819516235357,-13.9423914043819));
#48156=CARTESIAN_POINT('Ctrl Pts',(-7.00000966473096,6.97711954509652,-13.948714313882));
#48157=CARTESIAN_POINT('Ctrl Pts',(-6.2341298497682,11.870031945894,-24.393391026367));
#48158=CARTESIAN_POINT('Ctrl Pts',(-6.23490515007836,11.9504778000158,-23.8924703860421));
#48159=CARTESIAN_POINT('Ctrl Pts',(-6.23649294537174,12.0627648225871,-22.7260279240694));
#48160=CARTESIAN_POINT('Ctrl Pts',(-6.23803980036877,11.9701373820371,-20.8893409247744));
#48161=CARTESIAN_POINT('Ctrl Pts',(-6.23759260730665,11.5416382094031,-18.9411611420578));
#48162=CARTESIAN_POINT('Ctrl Pts',(-6.23570343585033,10.7961451762139,-17.0892587092505));
#48163=CARTESIAN_POINT('Ctrl Pts',(-6.23204961282645,9.75631588910903,-15.3875854443724));
#48164=CARTESIAN_POINT('Ctrl Pts',(-6.22726106267534,8.6169945866861,-14.0755190620509));
#48165=CARTESIAN_POINT('Ctrl Pts',(-6.22400151927379,7.81350031894818,-13.3673833063685));
#48166=CARTESIAN_POINT('Ctrl Pts',(-6.2226659932316,7.49367920211764,-13.1134096388249));
#48167=CARTESIAN_POINT('Ctrl Pts',(-6.72598992820685,11.7530860140233,-24.3745661708325));
#48168=CARTESIAN_POINT('Ctrl Pts',(-6.72668308530094,11.8323454549326,-23.8785347072491));
#48169=CARTESIAN_POINT('Ctrl Pts',(-6.72805134751943,11.9427141750406,-22.7235345581661));
#48170=CARTESIAN_POINT('Ctrl Pts',(-6.729418896676,11.8502318240213,-20.9054832492773));
#48171=CARTESIAN_POINT('Ctrl Pts',(-6.72902389879382,11.4262602892439,-18.9767992205318));
#48172=CARTESIAN_POINT('Ctrl Pts',(-6.7273678414525,10.6891576732562,-17.1431693745882));
#48173=CARTESIAN_POINT('Ctrl Pts',(-6.72416416502884,9.66125588094435,-15.4573959672442));
#48174=CARTESIAN_POINT('Ctrl Pts',(-6.71993329975334,8.53485935179034,-14.1564667453737));
#48175=CARTESIAN_POINT('Ctrl Pts',(-6.71707878522504,7.74006810589514,-13.4537901142132));
#48176=CARTESIAN_POINT('Ctrl Pts',(-6.7158900664978,7.42368987088072,-13.2016824589374));
#48177=CARTESIAN_POINT('Ctrl Pts',(-7.02718522726892,11.3520762594696,-24.3100157521472));
#48178=CARTESIAN_POINT('Ctrl Pts',(-7.02756392150913,11.4283599553699,-23.8309254769524));
#48179=CARTESIAN_POINT('Ctrl Pts',(-7.0282488325563,11.5344320553921,-22.7152040882476));
#48180=CARTESIAN_POINT('Ctrl Pts',(-7.02897715467319,11.4446324857795,-20.9601377668576));
#48181=CARTESIAN_POINT('Ctrl Pts',(-7.02876723083941,11.0353400441858,-19.0974452680292));
#48182=CARTESIAN_POINT('Ctrl Pts',(-7.0279026933489,10.3242146467833,-17.3268263925021));
#48183=CARTESIAN_POINT('Ctrl Pts',(-7.02622933623767,9.33267263994042,-15.6982356130382));
#48184=CARTESIAN_POINT('Ctrl Pts',(-7.02397930980613,8.24599547250213,-14.4407047902092));
#48185=CARTESIAN_POINT('Ctrl Pts',(-7.02249263040784,7.47887540073063,-13.7610260286471));
#48186=CARTESIAN_POINT('Ctrl Pts',(-7.02184967286603,7.17356126230332,-13.5171517118445));
#48187=CARTESIAN_POINT('Ctrl Pts',(-6.9983806254281,10.8539091305164,-24.2298260443849));
#48188=CARTESIAN_POINT('Ctrl Pts',(-6.99835912984722,10.9268138861166,-23.7718327253704));
#48189=CARTESIAN_POINT('Ctrl Pts',(-6.99821532188652,11.0282119309624,-22.7049190930737));
#48190=CARTESIAN_POINT('Ctrl Pts',(-6.99814245125572,10.9423807638968,-21.027831107362));
#48191=CARTESIAN_POINT('Ctrl Pts',(-6.99816421464904,10.5510777398404,-19.2468686040926));
#48192=CARTESIAN_POINT('Ctrl Pts',(-6.99828068956064,9.871410767818,-17.5546300609639));
#48193=CARTESIAN_POINT('Ctrl Pts',(-6.9985045686866,8.92371735875945,-15.9978504404111));
#48194=CARTESIAN_POINT('Ctrl Pts',(-6.99873523493892,7.88504484531634,-14.7957477722731));
#48195=CARTESIAN_POINT('Ctrl Pts',(-6.99894167920566,7.1516684994886,-14.1458833200365));
#48196=CARTESIAN_POINT('Ctrl Pts',(-6.99898903107869,6.85988337428983,-13.9127708060056));
#48197=CARTESIAN_POINT('',(-7.0000030891987,10.927769589406,-24.1259430621516));
#48198=CARTESIAN_POINT('Origin',(-5.99998370357436,10.9277595201359,-24.1259473086588));
#48199=CARTESIAN_POINT('Ctrl Pts',(-7.00001101651665,10.9277661762093,-24.1259401091756));
#48200=CARTESIAN_POINT('Ctrl Pts',(-7.0000178689439,10.9560764183263,-23.9375950050149));
#48201=CARTESIAN_POINT('Ctrl Pts',(-7.00001802523654,10.9791078956897,-23.7511663574579));
#48202=CARTESIAN_POINT('Ctrl Pts',(-7.00001556833325,10.997240350625,-23.566999236078));
#48203=CARTESIAN_POINT('Ctrl Pts',(-7.00001306404682,11.0157225030191,-23.37928031906));
#48204=CARTESIAN_POINT('Ctrl Pts',(-7.00000784335913,11.0291149028731,-23.1939109094671));
#48205=CARTESIAN_POINT('Ctrl Pts',(-7.00000354817103,11.0378133555915,-23.0112026941266));
#48206=CARTESIAN_POINT('Ctrl Pts',(-7.00000225617205,11.0404298631314,-22.9562437906837));
#48207=CARTESIAN_POINT('Ctrl Pts',(-7.00000104339744,11.0426216093023,-22.9015253189936));
#48208=CARTESIAN_POINT('Ctrl Pts',(-6.99999999753975,11.044399246237,-22.8470548569864));
#48209=CARTESIAN_POINT('Ctrl Pts',(-6.99999887667119,11.0463043786159,-22.7886776716144));
#48210=CARTESIAN_POINT('Ctrl Pts',(-6.99999794691843,11.0477338782397,-22.7305853426262));
#48211=CARTESIAN_POINT('Ctrl Pts',(-6.99999718088468,11.0487021581796,-22.6727848889157));
#48212=CARTESIAN_POINT('Ctrl Pts',(-6.99999462213086,11.0519364673514,-22.4797162009707));
#48213=CARTESIAN_POINT('Ctrl Pts',(-6.99999387749935,11.0500263119686,-22.2899077654462));
#48214=CARTESIAN_POINT('Ctrl Pts',(-6.99999403436533,11.0434957469855,-22.1035888577242));
#48215=CARTESIAN_POINT('Ctrl Pts',(-6.99999406718763,11.0421293056716,-22.064603891838));
#48216=CARTESIAN_POINT('Ctrl Pts',(-6.99999414005194,11.0405605105098,-22.0257715309591));
#48217=CARTESIAN_POINT('Ctrl Pts',(-6.99999424550212,11.0387940509543,-21.9870936125725));
#48218=CARTESIAN_POINT('Ctrl Pts',(-6.99999432423836,11.0374750927492,-21.9582140621436));
#48219=CARTESIAN_POINT('Ctrl Pts',(-6.99999441864869,11.0360814529893,-21.9301065592141));
#48220=CARTESIAN_POINT('Ctrl Pts',(-6.99999453140857,11.0345337169244,-21.9011843449435));
#48221=CARTESIAN_POINT('Ctrl Pts',(-6.99999463684067,11.0330865616108,-21.8741416617535));
#48222=CARTESIAN_POINT('Ctrl Pts',(-6.99999475849192,11.0315045688866,-21.846386673071));
#48223=CARTESIAN_POINT('Ctrl Pts',(-6.9999949035284,11.029681939679,-21.8166247929757));
#48224=CARTESIAN_POINT('Ctrl Pts',(-6.99999520368176,11.0259100041799,-21.755032511024));
#48225=CARTESIAN_POINT('Ctrl Pts',(-6.9999955626785,11.0216269151297,-21.6935868226501));
#48226=CARTESIAN_POINT('Ctrl Pts',(-6.9999959537239,11.0168388651946,-21.6322954802246));
#48227=CARTESIAN_POINT('Ctrl Pts',(-6.99999673581471,11.0072627653243,-21.5097127953737));
#48228=CARTESIAN_POINT('Ctrl Pts',(-6.99999764539611,10.9956668219142,-21.387747494317));
#48229=CARTESIAN_POINT('Ctrl Pts',(-6.99999847634374,10.9821001708853,-21.2664589704134));
#48230=CARTESIAN_POINT('Ctrl Pts',(-6.99999902467265,10.9731477573094,-21.1864226353089));
#48231=CARTESIAN_POINT('Ctrl Pts',(-6.99999953898542,10.9633371968182,-21.1066809430449));
#48232=CARTESIAN_POINT('Ctrl Pts',(-6.99999996276672,10.9526825043711,-21.0272502934151));
#48233=CARTESIAN_POINT('Ctrl Pts',(-7.00000126736559,10.9198823315757,-20.7827252593973));
#48234=CARTESIAN_POINT('Ctrl Pts',(-7.00000171384871,10.8790835251978,-20.5411517571741));
#48235=CARTESIAN_POINT('Ctrl Pts',(-7.00000170643162,10.8307721803972,-20.3030233611526));
#48236=CARTESIAN_POINT('Ctrl Pts',(-7.00000169893522,10.7819442740525,-20.0623488142742));
#48237=CARTESIAN_POINT('Ctrl Pts',(-7.00000122941415,10.7254423237568,-19.8251933968343));
#48238=CARTESIAN_POINT('Ctrl Pts',(-7.0000007234276,10.6617526620477,-19.5920156367625));
#48239=CARTESIAN_POINT('Ctrl Pts',(-7.00000046988901,10.6298391901355,-19.4751754511354));
#48240=CARTESIAN_POINT('Ctrl Pts',(-7.00000020716685,10.5961207929503,-19.3593331797781));
#48241=CARTESIAN_POINT('Ctrl Pts',(-6.99999998766517,10.5606572076705,-19.2445418256472));
#48242=CARTESIAN_POINT('Ctrl Pts',(-6.99999993928869,10.5528413054783,-19.219242691639));
#48243=CARTESIAN_POINT('Ctrl Pts',(-6.9999998930055,10.5449406310664,-19.1939945917012));
#48244=CARTESIAN_POINT('Ctrl Pts',(-6.99999984878303,10.5369559371202,-19.1687979951081));
#48245=CARTESIAN_POINT('Ctrl Pts',(-6.99999965374478,10.5017403435686,-19.0576712430394));
#48246=CARTESIAN_POINT('Ctrl Pts',(-6.99999949863674,10.4648905474801,-18.9475464970961));
#48247=CARTESIAN_POINT('Ctrl Pts',(-6.99999938184587,10.4264702932223,-18.8384625308438));
#48248=CARTESIAN_POINT('Ctrl Pts',(-6.99999932345044,10.4072601660933,-18.7839205477176));
#48249=CARTESIAN_POINT('Ctrl Pts',(-6.99999927466561,10.3876574244221,-18.7296387595141));
#48250=CARTESIAN_POINT('Ctrl Pts',(-6.99999923547375,10.3676698878029,-18.6756217474293));
#48251=CARTESIAN_POINT('Ctrl Pts',(-6.99999921587781,10.3576761194934,-18.6486132413869));
#48252=CARTESIAN_POINT('Ctrl Pts',(-6.99999919868214,10.3475861524468,-18.6216709293742));
#48253=CARTESIAN_POINT('Ctrl Pts',(-6.9999991838965,10.3374009596986,-18.5947953762306));
#48254=CARTESIAN_POINT('Ctrl Pts',(-6.99999917283138,10.3297786753504,-18.5746825405544));
#48255=CARTESIAN_POINT('Ctrl Pts',(-6.99999916268833,10.3217399609405,-18.5536617176207));
#48256=CARTESIAN_POINT('Ctrl Pts',(-6.99999915445986,10.31409937907,-18.5338560146091));
#48257=CARTESIAN_POINT('Ctrl Pts',(-6.99999915169312,10.3115303183315,-18.5271965670869));
#48258=CARTESIAN_POINT('Ctrl Pts',(-6.99999914913282,10.3090066899196,-18.5206743351133));
#48259=CARTESIAN_POINT('Ctrl Pts',(-6.99999914678744,10.3065606748726,-18.5143695537774));
#48260=CARTESIAN_POINT('Ctrl Pts',(-6.99999907529418,10.2319997646018,-18.3221833952997));
#48261=CARTESIAN_POINT('Ctrl Pts',(-6.99999912491849,10.1510712733243,-18.1296184689333));
#48262=CARTESIAN_POINT('Ctrl Pts',(-6.99999933315943,10.0634928197255,-17.9371558145606));
#48263=CARTESIAN_POINT('Ctrl Pts',(-6.99999947285716,10.0047411118898,-17.8080428972351));
#48264=CARTESIAN_POINT('Ctrl Pts',(-6.99999968443218,9.94299688374547,-17.678977014169));
#48265=CARTESIAN_POINT('Ctrl Pts',(-6.99999998816759,9.87817756885076,-17.5501163140756));
#48266=CARTESIAN_POINT('Ctrl Pts',(-7.00000042903653,9.78409297605115,-17.3630762857159));
#48267=CARTESIAN_POINT('Ctrl Pts',(-7.0000010678068,9.68352878376437,-17.1764663552485));
#48268=CARTESIAN_POINT('Ctrl Pts',(-7.00000153331188,9.57627842588298,-16.9908082299143));
#48269=CARTESIAN_POINT('Ctrl Pts',(-7.00000199134791,9.47074890515542,-16.8081289981363));
#48270=CARTESIAN_POINT('Ctrl Pts',(-7.00000228132013,9.35874600671699,-16.6263712423838));
#48271=CARTESIAN_POINT('Ctrl Pts',(-7.00000202662856,9.24008894373901,-16.4460793865259));
#48272=CARTESIAN_POINT('Ctrl Pts',(-7.000001812094,9.14014044338894,-16.2942140009678));
#48273=CARTESIAN_POINT('Ctrl Pts',(-7.0000012106318,9.03547091581878,-16.1433894613444));
#48274=CARTESIAN_POINT('Ctrl Pts',(-6.99999998662418,8.92598177928851,-15.9939582849167));
#48275=CARTESIAN_POINT('Ctrl Pts',(-6.99999852881463,8.7955787440933,-15.8159837426334));
#48276=CARTESIAN_POINT('Ctrl Pts',(-6.99999617286889,8.65833776962605,-15.639985120766));
#48277=CARTESIAN_POINT('Ctrl Pts',(-6.99999449845809,8.51417826060077,-15.4665284038773));
#48278=CARTESIAN_POINT('Ctrl Pts',(-6.99999284826976,8.37210420131663,-15.295580957919));
#48279=CARTESIAN_POINT('Ctrl Pts',(-6.99999186158911,8.22331027668761,-15.1271023856721));
#48280=CARTESIAN_POINT('Ctrl Pts',(-6.99999320067939,8.06774699367314,-14.9616765568042));
#48281=CARTESIAN_POINT('Ctrl Pts',(-6.99999413395892,7.95932709874448,-14.8463829564328));
#48282=CARTESIAN_POINT('Ctrl Pts',(-6.99999620011753,7.84761962633808,-14.7325730635345));
#48283=CARTESIAN_POINT('Ctrl Pts',(-6.99999999965478,7.73261617693726,-14.6204570168772));
#48284=CARTESIAN_POINT('Ctrl Pts',(-7.00000506883503,7.57918348853654,-14.4708765778458));
#48285=CARTESIAN_POINT('Ctrl Pts',(-7.0000132984882,7.41988233836246,-14.3243094370825));
#48286=CARTESIAN_POINT('Ctrl Pts',(-7.00001657716769,7.25479675802074,-14.1813267045858));
#48287=CARTESIAN_POINT('Ctrl Pts',(-7.00001838080306,7.16398147886925,-14.1026704298303));
#48288=CARTESIAN_POINT('Ctrl Pts',(-7.00001867122436,7.07141628639037,-14.0250995594017));
#48289=CARTESIAN_POINT('Ctrl Pts',(-7.00001598720849,6.97711954487508,-13.9487143136413));
#48290=CARTESIAN_POINT('Origin',(-5.999994980806,10.9277770011849,-24.1259380084193));
#48291=CARTESIAN_POINT('Origin',(-6.,10.9277790621896,-24.1259427055443));
#48292=CARTESIAN_POINT('Ctrl Pts',(-7.10365375325716,5.08556213759161,-15.2124200606729));
#48293=CARTESIAN_POINT('Ctrl Pts',(-7.10425940579783,5.03547652135492,-15.2289541394246));
#48294=CARTESIAN_POINT('Ctrl Pts',(-7.09698248863266,4.87479892200809,-15.2843333495191));
#48295=CARTESIAN_POINT('Ctrl Pts',(-7.03475514727946,4.61092148639726,-15.3877970248073));
#48296=CARTESIAN_POINT('Ctrl Pts',(-6.88260033893558,4.32655598757909,-15.5206346518419));
#48297=CARTESIAN_POINT('Ctrl Pts',(-6.66949670496425,4.10048277670444,-15.649982801355));
#48298=CARTESIAN_POINT('Ctrl Pts',(-6.45007050561619,3.96694228146696,-15.7511248346751));
#48299=CARTESIAN_POINT('Ctrl Pts',(-6.30610234990484,3.91682262999853,-15.8056261738581));
#48300=CARTESIAN_POINT('Ctrl Pts',(-6.25371803308994,3.90293324094133,-15.8240946813389));
#48301=CARTESIAN_POINT('Ctrl Pts',(-6.81817564339306,4.90140851365106,-14.6657612012878));
#48302=CARTESIAN_POINT('Ctrl Pts',(-6.8187209234073,4.8571674745428,-14.6803578801389));
#48303=CARTESIAN_POINT('Ctrl Pts',(-6.81217849063633,4.71506404703517,-14.7294286095061));
#48304=CARTESIAN_POINT('Ctrl Pts',(-6.75596877441542,4.48132758213125,-14.8218932719452));
#48305=CARTESIAN_POINT('Ctrl Pts',(-6.61862718319516,4.23005438056527,-14.9412123965516));
#48306=CARTESIAN_POINT('Ctrl Pts',(-6.42697177765079,4.03134800350222,-15.057457108221));
#48307=CARTESIAN_POINT('Ctrl Pts',(-6.23069936786126,3.91487721740648,-15.1480748819103));
#48308=CARTESIAN_POINT('Ctrl Pts',(-6.1026337152333,3.87149278153041,-15.1966642579316));
#48309=CARTESIAN_POINT('Ctrl Pts',(-6.05613610180907,3.85950522648497,-15.2130939828674));
#48310=CARTESIAN_POINT('Ctrl Pts',(-7.06073274467296,4.7170686558441,-14.098996840888));
#48311=CARTESIAN_POINT('Ctrl Pts',(-7.06144827708986,4.65990256849783,-14.1178698225721));
#48312=CARTESIAN_POINT('Ctrl Pts',(-7.05282245267813,4.47706838045324,-14.1808763385047));
#48313=CARTESIAN_POINT('Ctrl Pts',(-6.97988948335629,4.17817855160872,-14.2979140353396));
#48314=CARTESIAN_POINT('Ctrl Pts',(-6.80124511423192,3.85488795162216,-14.4486451526198));
#48315=CARTESIAN_POINT('Ctrl Pts',(-6.54883128807966,3.59536050662941,-14.5970203599067));
#48316=CARTESIAN_POINT('Ctrl Pts',(-6.28555951712999,3.43993495535892,-14.71508158883));
#48317=CARTESIAN_POINT('Ctrl Pts',(-6.11058332363383,3.38094754188304,-14.7799070207993));
#48318=CARTESIAN_POINT('Ctrl Pts',(-6.04660001229308,3.36455643057283,-14.8020435974322));
#48319=CARTESIAN_POINT('Ctrl Pts',(-7.66739167259926,4.65664426237229,-13.8937090025063));
#48320=CARTESIAN_POINT('Ctrl Pts',(-7.66839318582775,4.57650762421567,-13.9201855750848));
#48321=CARTESIAN_POINT('Ctrl Pts',(-7.65627208602678,4.32113029813062,-14.0079657876853));
#48322=CARTESIAN_POINT('Ctrl Pts',(-7.55516094421515,3.90577067771103,-14.1685624456636));
#48323=CARTESIAN_POINT('Ctrl Pts',(-7.30697159306207,3.45396377815488,-14.3744344773038));
#48324=CARTESIAN_POINT('Ctrl Pts',(-6.95259600190474,3.08648007996775,-14.5784884618108));
#48325=CARTESIAN_POINT('Ctrl Pts',(-6.57738617026409,2.86236823778828,-14.7434394142203));
#48326=CARTESIAN_POINT('Ctrl Pts',(-6.32434354928332,2.77597093213413,-14.8356916710563));
#48327=CARTESIAN_POINT('Ctrl Pts',(-6.23130215550449,2.7518430695664,-14.8674293899488));
#48328=CARTESIAN_POINT('',(-6.26386059950783,3.90573753004527,-15.8144217560873));
#48329=CARTESIAN_POINT('',(-6.24994547032252,2.76546740288181,-14.8593848470608));
#48330=CARTESIAN_POINT('Ctrl Pts',(-6.26385524237826,3.90575711203162,-15.8144219713711));
#48331=CARTESIAN_POINT('Ctrl Pts',(-6.25431842670559,3.90347140179835,-15.7850251932568));
#48332=CARTESIAN_POINT('Ctrl Pts',(-6.24496510276104,3.89974753513886,-15.7549999297834));
#48333=CARTESIAN_POINT('Ctrl Pts',(-6.23589623365663,3.89443541490935,-15.7245193832421));
#48334=CARTESIAN_POINT('Ctrl Pts',(-6.22705377181037,3.88925591348405,-15.6947997934297));
#48335=CARTESIAN_POINT('Ctrl Pts',(-6.21848203426885,3.88256579299046,-15.6646476750876));
#48336=CARTESIAN_POINT('Ctrl Pts',(-6.21028075854689,3.87425393748282,-15.6342636592137));
#48337=CARTESIAN_POINT('Ctrl Pts',(-6.2022059505754,3.86607025492093,-15.6043481799758));
#48338=CARTESIAN_POINT('Ctrl Pts',(-6.19449059505007,3.85631385047443,-15.5742083486252));
#48339=CARTESIAN_POINT('Ctrl Pts',(-6.18723134420193,3.8449157925931,-15.5440695413971));
#48340=CARTESIAN_POINT('Ctrl Pts',(-6.18009971140207,3.83371811322622,-15.5144605761369));
#48341=CARTESIAN_POINT('Ctrl Pts',(-6.17340862814906,3.82093556240753,-15.4848532328916));
#48342=CARTESIAN_POINT('Ctrl Pts',(-6.16724621350028,3.80654661238053,-15.4554861432826));
#48343=CARTESIAN_POINT('Ctrl Pts',(-6.16645007886344,3.8046876752338,-15.4516921504156));
#48344=CARTESIAN_POINT('Ctrl Pts',(-6.16566275894613,3.80280199211259,-15.447902194074));
#48345=CARTESIAN_POINT('Ctrl Pts',(-6.16488443472348,3.80088957628181,-15.4441168105991));
#48346=CARTESIAN_POINT('Ctrl Pts',(-6.15895241115861,3.78631403636689,-15.4152663864167));
#48347=CARTESIAN_POINT('Ctrl Pts',(-6.15354382259298,3.77018160286767,-15.3866810289208));
#48348=CARTESIAN_POINT('Ctrl Pts',(-6.14873326440852,3.752526237599,-15.3586037373115));
#48349=CARTESIAN_POINT('Ctrl Pts',(-6.14398433495375,3.73509705766934,-15.3308861477885));
#48350=CARTESIAN_POINT('Ctrl Pts',(-6.13981848386434,3.71618373826285,-15.3036644956293));
#48351=CARTESIAN_POINT('Ctrl Pts',(-6.13629421425756,3.69586792599309,-15.277173486802));
#48352=CARTESIAN_POINT('Ctrl Pts',(-6.13279064028137,3.67567141462606,-15.250838041593));
#48353=CARTESIAN_POINT('Ctrl Pts',(-6.12992135457027,3.65408904541089,-15.2252254892552));
#48354=CARTESIAN_POINT('Ctrl Pts',(-6.12772694082186,3.63124809294815,-15.2005553078385));
#48355=CARTESIAN_POINT('Ctrl Pts',(-6.12553997337744,3.60848464668758,-15.1759688397464));
#48356=CARTESIAN_POINT('Ctrl Pts',(-6.12402344438827,3.58447157299373,-15.152319103387));
#48357=CARTESIAN_POINT('Ctrl Pts',(-6.12319799097326,3.5593769534127,-15.1298006183463));
#48358=CARTESIAN_POINT('Ctrl Pts',(-6.12237328082849,3.5343049299996,-15.1073024098221));
#48359=CARTESIAN_POINT('Ctrl Pts',(-6.12223844696652,3.50815392308848,-15.0859340393127));
#48360=CARTESIAN_POINT('Ctrl Pts',(-6.12279314210064,3.48112581360472,-15.0658564449281));
#48361=CARTESIAN_POINT('Ctrl Pts',(-6.12335053997515,3.45396601022447,-15.045681022886));
#48362=CARTESIAN_POINT('Ctrl Pts',(-6.12460415940122,3.42592128542679,-15.0268094621603));
#48363=CARTESIAN_POINT('Ctrl Pts',(-6.12653245965907,3.39722080139595,-15.009363286171));
#48364=CARTESIAN_POINT('Ctrl Pts',(-6.12846822014428,3.36840928064495,-14.9918496142414));
#48365=CARTESIAN_POINT('Ctrl Pts',(-6.13108374049619,3.3389377607077,-14.9757726162461));
#48366=CARTESIAN_POINT('Ctrl Pts',(-6.13433741011253,3.30905041842281,-14.9612078107311));
#48367=CARTESIAN_POINT('Ctrl Pts',(-6.13762846464348,3.27881966827212,-14.9464756544786));
#48368=CARTESIAN_POINT('Ctrl Pts',(-6.14157219435981,3.24816435165046,-14.9332906905176));
#48369=CARTESIAN_POINT('Ctrl Pts',(-6.14610811724841,3.21733673198634,-14.9216803414444));
#48370=CARTESIAN_POINT('Ctrl Pts',(-6.14941180669293,3.19488377496189,-14.9132240716572));
#48371=CARTESIAN_POINT('Ctrl Pts',(-6.15302925331993,3.17233943514232,-14.9056019936076));
#48372=CARTESIAN_POINT('Ctrl Pts',(-6.15693255119853,3.14979720314684,-14.8988083887852));
#48373=CARTESIAN_POINT('Ctrl Pts',(-6.16238723402997,3.11829545009785,-14.8893146322898));
#48374=CARTESIAN_POINT('Ctrl Pts',(-6.16840043529369,3.08679919654159,-14.8814403581585));
#48375=CARTESIAN_POINT('Ctrl Pts',(-6.17488786719185,3.05554401213897,-14.8751293194312));
#48376=CARTESIAN_POINT('Ctrl Pts',(-6.1815237056771,3.0235738336803,-14.8686739092895));
#48377=CARTESIAN_POINT('Ctrl Pts',(-6.18865536712829,2.99185651849639,-14.8638535662064));
#48378=CARTESIAN_POINT('Ctrl Pts',(-6.19618723020727,2.9606107284726,-14.8605653101527));
#48379=CARTESIAN_POINT('Ctrl Pts',(-6.20383065418149,2.92890213020723,-14.8572283489135));
#48380=CARTESIAN_POINT('Ctrl Pts',(-6.21188586975053,2.89767951081031,-14.8554684804184));
#48381=CARTESIAN_POINT('Ctrl Pts',(-6.2202528897936,2.86712951671446,-14.8551440416511));
#48382=CARTESIAN_POINT('Ctrl Pts',(-6.22882057895255,2.83584683161588,-14.8548118217573));
#48383=CARTESIAN_POINT('Ctrl Pts',(-6.23771488179524,2.80526963802762,-14.8559839371986));
#48384=CARTESIAN_POINT('Ctrl Pts',(-6.24683365328605,2.77555001402948,-14.85848431103));
#48385=CARTESIAN_POINT('Ctrl Pts',(-6.24786821957997,2.77217818688287,-14.8587679898667));
#48386=CARTESIAN_POINT('Ctrl Pts',(-6.24890568355812,2.76881734680998,-14.8590687484887));
#48387=CARTESIAN_POINT('Ctrl Pts',(-6.24994590287157,2.76546767660005,-14.8593863177582));
#48388=CARTESIAN_POINT('',(-7.00000030631414,3.1661281488063,-14.5427419373966));
#48389=CARTESIAN_POINT('Ctrl Pts',(-7.00000091797045,3.16612715294925,-14.5427414491965));
#48390=CARTESIAN_POINT('Ctrl Pts',(-6.9770948764676,3.14616537143328,-14.5547620427858));
#48391=CARTESIAN_POINT('Ctrl Pts',(-6.9538163142397,3.12684702049389,-14.5666755023522));
#48392=CARTESIAN_POINT('Ctrl Pts',(-6.93017491231045,3.10816085848109,-14.5784854676487));
#48393=CARTESIAN_POINT('Ctrl Pts',(-6.88947876003189,3.07599462328698,-14.5988150634802));
#48394=CARTESIAN_POINT('Ctrl Pts',(-6.84770978866817,3.04569988961234,-14.6188379878143));
#48395=CARTESIAN_POINT('Ctrl Pts',(-6.80491841661944,3.01722957302793,-14.6385688721317));
#48396=CARTESIAN_POINT('Ctrl Pts',(-6.76163570292131,2.98843235287302,-14.6585263115882));
#48397=CARTESIAN_POINT('Ctrl Pts',(-6.71730648856817,2.96150123974364,-14.6781851761215));
#48398=CARTESIAN_POINT('Ctrl Pts',(-6.67194315514633,2.93642225616261,-14.6975594142133));
#48399=CARTESIAN_POINT('Ctrl Pts',(-6.66414019379478,2.93210841225261,-14.7008919830446));
#48400=CARTESIAN_POINT('Ctrl Pts',(-6.65630655130121,2.92784946010201,-14.7042161232254));
#48401=CARTESIAN_POINT('Ctrl Pts',(-6.64844218978448,2.92364544595408,-14.7075318951735));
#48402=CARTESIAN_POINT('Ctrl Pts',(-6.60349501531205,2.89961824972342,-14.7264825219913));
#48403=CARTESIAN_POINT('Ctrl Pts',(-6.55756813993438,2.87738307797186,-14.7451532943523));
#48404=CARTESIAN_POINT('Ctrl Pts',(-6.51063098898213,2.85696654565969,-14.7635563543032));
#48405=CARTESIAN_POINT('Ctrl Pts',(-6.50668245189925,2.85524902695004,-14.7651044918271));
#48406=CARTESIAN_POINT('Ctrl Pts',(-6.50272675016091,2.85354440476764,-14.7666507309458));
#48407=CARTESIAN_POINT('Ctrl Pts',(-6.4987638575357,2.85185270971999,-14.7681950766425));
#48408=CARTESIAN_POINT('Ctrl Pts',(-6.45236637950589,2.83204637348299,-14.7862762492376));
#48409=CARTESIAN_POINT('Ctrl Pts',(-6.40498461823921,2.81400816695435,-14.8040986136675));
#48410=CARTESIAN_POINT('Ctrl Pts',(-6.35660284408077,2.79778989501982,-14.8216604597072));
#48411=CARTESIAN_POINT('Ctrl Pts',(-6.32157843143683,2.78604920426411,-14.8343737872605));
#48412=CARTESIAN_POINT('Ctrl Pts',(-6.2860294977681,2.77526317253696,-14.8469504427215));
#48413=CARTESIAN_POINT('Ctrl Pts',(-6.24994590287805,2.76546767660181,-14.8593863177559));
#48414=CARTESIAN_POINT('',(-7.000003179836,4.92966193726001,-14.7967990013279));
#48415=CARTESIAN_POINT('Ctrl Pts',(-7.,4.92966193726001,-14.7967990013279));
#48416=CARTESIAN_POINT('Ctrl Pts',(-7.,4.77605682881269,-14.7360009948777));
#48417=CARTESIAN_POINT('Ctrl Pts',(-7.,4.63248720373973,-14.6852063747094));
#48418=CARTESIAN_POINT('Ctrl Pts',(-7.,4.49895306204113,-14.6444151408229));
#48419=CARTESIAN_POINT('Ctrl Pts',(-7.,4.47987675608419,-14.6385878216963));
#48420=CARTESIAN_POINT('Ctrl Pts',(-7.,4.46218562630564,-14.6333073196583));
#48421=CARTESIAN_POINT('Ctrl Pts',(-7.,4.44233856151975,-14.6275456356643));
#48422=CARTESIAN_POINT('Ctrl Pts',(-7.,4.28356204323264,-14.5814521637125));
#48423=CARTESIAN_POINT('Ctrl Pts',(-7.,4.12817410523823,-14.5472790797429));
#48424=CARTESIAN_POINT('Ctrl Pts',(-7.,3.98124764966623,-14.5257690562941));
#48425=CARTESIAN_POINT('Ctrl Pts',(-7.,3.68739473852224,-14.4827490093966));
#48426=CARTESIAN_POINT('Ctrl Pts',(-7.,3.41568850431818,-14.4884065002489));
#48427=CARTESIAN_POINT('Ctrl Pts',(-7.,3.16612894705406,-14.5427415288511));
#48428=CARTESIAN_POINT('Ctrl Pts',(-6.99999286694104,4.92966193658926,-14.7967990014538));
#48429=CARTESIAN_POINT('Ctrl Pts',(-6.99999564996434,4.89205532347658,-14.8244082330937));
#48430=CARTESIAN_POINT('Ctrl Pts',(-6.99822284827502,4.85539428974177,-14.8517940861305));
#48431=CARTESIAN_POINT('Ctrl Pts',(-6.99489375804626,4.81982245813974,-14.878828057977));
#48432=CARTESIAN_POINT('Ctrl Pts',(-6.99462619840172,4.81696354295125,-14.881000783677));
#48433=CARTESIAN_POINT('Ctrl Pts',(-6.9943485697214,4.81411164574981,-14.8831712499741));
#48434=CARTESIAN_POINT('Ctrl Pts',(-6.99406097763697,4.81126683193698,-14.8853393971188));
#48435=CARTESIAN_POINT('Ctrl Pts',(-6.99033942241299,4.7744538169769,-14.9133960779864));
#48436=CARTESIAN_POINT('Ctrl Pts',(-6.9849529474007,4.73882903512714,-14.9410624452149));
#48437=CARTESIAN_POINT('Ctrl Pts',(-6.9781797927941,4.70446949083707,-14.9682300007031));
#48438=CARTESIAN_POINT('Ctrl Pts',(-6.97105384631412,4.6683202682209,-14.9968126269157));
#48439=CARTESIAN_POINT('Ctrl Pts',(-6.96239262273182,4.63357165756106,-15.0248431548408));
#48440=CARTESIAN_POINT('Ctrl Pts',(-6.95247705584319,4.60028408585532,-15.0522212395062));
#48441=CARTESIAN_POINT('Ctrl Pts',(-6.94757952211403,4.58384256445549,-15.0657439250566));
#48442=CARTESIAN_POINT('Ctrl Pts',(-6.94237537208527,4.56775702816083,-15.0791078258971));
#48443=CARTESIAN_POINT('Ctrl Pts',(-6.93689528828872,4.55203217545746,-15.0923029711967));
#48444=CARTESIAN_POINT('Ctrl Pts',(-6.93467726086207,4.54566764603222,-15.0976436183947));
#48445=CARTESIAN_POINT('Ctrl Pts',(-6.93241400773592,4.53936217946447,-15.1029566354528));
#48446=CARTESIAN_POINT('Ctrl Pts',(-6.93010747891385,4.5331160093562,-15.1082414213626));
#48447=CARTESIAN_POINT('Ctrl Pts',(-6.91797461530297,4.50025974097198,-15.1360405912857));
#48448=CARTESIAN_POINT('Ctrl Pts',(-6.90464803705654,4.46904585533628,-15.1630568165268));
#48449=CARTESIAN_POINT('Ctrl Pts',(-6.89043334783286,4.43945534086122,-15.1892214494785));
#48450=CARTESIAN_POINT('Ctrl Pts',(-6.88415593696834,4.42638774479002,-15.2007761270781));
#48451=CARTESIAN_POINT('Ctrl Pts',(-6.87770473235698,4.41363646979168,-15.2121650142821));
#48452=CARTESIAN_POINT('Ctrl Pts',(-6.87110345805848,4.40119860659756,-15.2233834948398));
#48453=CARTESIAN_POINT('Ctrl Pts',(-6.8589079386848,4.37822028533836,-15.2441090685394));
#48454=CARTESIAN_POINT('Ctrl Pts',(-6.84620107686014,4.35631215709294,-15.2642525838018));
#48455=CARTESIAN_POINT('Ctrl Pts',(-6.83312021232246,4.33544918998589,-15.2837912532757));
#48456=CARTESIAN_POINT('Ctrl Pts',(-6.82657978005362,4.32501770643236,-15.2935605880126));
#48457=CARTESIAN_POINT('Ctrl Pts',(-6.81994561022378,4.31484737937306,-15.3031788347256));
#48458=CARTESIAN_POINT('Ctrl Pts',(-6.81323353961138,4.30493429434116,-15.3126438440873));
#48459=CARTESIAN_POINT('Ctrl Pts',(-6.80987750430517,4.2999777518252,-15.3173763487682));
#48460=CARTESIAN_POINT('Ctrl Pts',(-6.80650198885739,4.2950855234087,-15.3220705443057));
#48461=CARTESIAN_POINT('Ctrl Pts',(-6.80310888496519,4.29025705555333,-15.3267262121182));
#48462=CARTESIAN_POINT('Ctrl Pts',(-6.80264177898385,4.28959235258884,-15.3273671268533));
#48463=CARTESIAN_POINT('Ctrl Pts',(-6.80218983720927,4.28895089234423,-15.3279861090097));
#48464=CARTESIAN_POINT('Ctrl Pts',(-6.80174677252703,4.28832348630925,-15.3285919214149));
#48465=CARTESIAN_POINT('Ctrl Pts',(-6.79969749752605,4.28542159059405,-15.3313939416772));
#48466=CARTESIAN_POINT('Ctrl Pts',(-6.79784094933337,4.28281805980717,-15.3339144164748));
#48467=CARTESIAN_POINT('Ctrl Pts',(-6.79553303480481,4.27962145346957,-15.3370189588579));
#48468=CARTESIAN_POINT('Ctrl Pts',(-6.79471526443204,4.27848879022579,-15.3381190008008));
#48469=CARTESIAN_POINT('Ctrl Pts',(-6.79384050039992,4.27728192903732,-15.3392923513023));
#48470=CARTESIAN_POINT('Ctrl Pts',(-6.79287881305449,4.27596226696631,-15.3405774256209));
#48471=CARTESIAN_POINT('Ctrl Pts',(-6.76344871351334,4.23557722260151,-15.3799039960427));
#48472=CARTESIAN_POINT('Ctrl Pts',(-6.73147738565455,4.19791990254157,-15.4183236940747));
#48473=CARTESIAN_POINT('Ctrl Pts',(-6.69741369430494,4.16317486975606,-15.4556739695271));
#48474=CARTESIAN_POINT('Ctrl Pts',(-6.6723851532128,4.13764570816594,-15.4831173518185));
#48475=CARTESIAN_POINT('Ctrl Pts',(-6.64622571368188,4.11368903830416,-15.5099838815156));
#48476=CARTESIAN_POINT('Ctrl Pts',(-6.61909739248669,4.09137864535545,-15.53621638348));
#48477=CARTESIAN_POINT('Ctrl Pts',(-6.58048856707105,4.05962665966812,-15.5735502856139));
#48478=CARTESIAN_POINT('Ctrl Pts',(-6.53991979868992,4.03120839444587,-15.6095992241468));
#48479=CARTESIAN_POINT('Ctrl Pts',(-6.4979261990087,4.00620592936192,-15.6442274537135));
#48480=CARTESIAN_POINT('Ctrl Pts',(-6.46405457048637,3.98603918452713,-15.6721582464336));
#48481=CARTESIAN_POINT('Ctrl Pts',(-6.4292547471293,3.9680951187726,-15.6991651680106));
#48482=CARTESIAN_POINT('Ctrl Pts',(-6.39378500341098,3.95241730850598,-15.72518648339));
#48483=CARTESIAN_POINT('Ctrl Pts',(-6.35127484432409,3.93362759821485,-15.7563727886877));
#48484=CARTESIAN_POINT('Ctrl Pts',(-6.30780377631186,3.91809224092562,-15.7861432724349));
#48485=CARTESIAN_POINT('Ctrl Pts',(-6.26385524237827,3.90575711203162,-15.8144219713711));
#48486=CARTESIAN_POINT('Ctrl Pts',(-6.22266644339182,3.97375010659389,-14.571407576345));
#48487=CARTESIAN_POINT('Ctrl Pts',(-6.22400197463445,3.9271886321768,-14.9771430893856));
#48488=CARTESIAN_POINT('Ctrl Pts',(-6.22726156144324,3.85975967588295,-16.0460292272317));
#48489=CARTESIAN_POINT('Ctrl Pts',(-6.23205009249213,3.98190899774585,-17.7794229322491));
#48490=CARTESIAN_POINT('Ctrl Pts',(-6.2357039221351,4.44990335836682,-19.7179581688241));
#48491=CARTESIAN_POINT('Ctrl Pts',(-6.23759309150179,5.23225296824271,-21.5545940964061));
#48492=CARTESIAN_POINT('Ctrl Pts',(-6.23804028505047,6.30682939060215,-23.2351598502083));
#48493=CARTESIAN_POINT('Ctrl Pts',(-6.23649343327119,7.54006311272245,-24.5993882837727));
#48494=CARTESIAN_POINT('Ctrl Pts',(-6.23490564632112,8.44425758305475,-25.3447862637746));
#48495=CARTESIAN_POINT('Ctrl Pts',(-6.23413035365508,8.85534224317308,-25.6421049454179));
#48496=CARTESIAN_POINT('Ctrl Pts',(-6.7158893426021,4.08565830959416,-14.5843360049734));
#48497=CARTESIAN_POINT('Ctrl Pts',(-6.71707806185619,4.04021185391681,-14.986317551748));
#48498=CARTESIAN_POINT('Ctrl Pts',(-6.71993259305533,3.97507670179734,-16.0451895055534));
#48499=CARTESIAN_POINT('Ctrl Pts',(-6.72416345393324,4.09849003995885,-17.7615688573897));
#48500=CARTESIAN_POINT('Ctrl Pts',(-6.7273671322325,4.56367551651715,-19.6804271855846));
#48501=CARTESIAN_POINT('Ctrl Pts',(-6.72902318958527,5.33903737570472,-21.498209528469));
#48502=CARTESIAN_POINT('Ctrl Pts',(-6.72941818465536,6.40302974530858,-23.1617881848097));
#48503=CARTESIAN_POINT('Ctrl Pts',(-6.72805064861496,7.62318866866407,-24.5127366297367));
#48504=CARTESIAN_POINT('Ctrl Pts',(-6.72668237271919,8.51793580395378,-25.251400142793));
#48505=CARTESIAN_POINT('Ctrl Pts',(-6.72598922608832,8.92472441076612,-25.5461005895199));
#48506=CARTESIAN_POINT('Ctrl Pts',(-7.02184868340148,4.48559520701657,-14.6305388743154));
#48507=CARTESIAN_POINT('Ctrl Pts',(-7.0224916377447,4.44215040628042,-15.0188750689058));
#48508=CARTESIAN_POINT('Ctrl Pts',(-7.02397830295891,4.38031978877979,-16.0419185664938));
#48509=CARTESIAN_POINT('Ctrl Pts',(-7.02622834797599,4.50113166000826,-17.6995249602702));
#48510=CARTESIAN_POINT('Ctrl Pts',(-7.0279017053608,4.95159320929153,-19.5522389867469));
#48511=CARTESIAN_POINT('Ctrl Pts',(-7.02876624731174,5.70076832635135,-21.307097360822));
#48512=CARTESIAN_POINT('Ctrl Pts',(-7.02897616615894,6.72847743169267,-22.913633439955));
#48513=CARTESIAN_POINT('Ctrl Pts',(-7.02824786192413,7.90599646240988,-24.2181479833785));
#48514=CARTESIAN_POINT('Ctrl Pts',(-7.02756291581688,8.76993137994633,-24.9320755587743));
#48515=CARTESIAN_POINT('Ctrl Pts',(-7.0271842308215,9.16263674770637,-25.2169010333086));
#48516=CARTESIAN_POINT('Ctrl Pts',(-6.99898915857891,4.98714290566693,-14.6884801835189));
#48517=CARTESIAN_POINT('Ctrl Pts',(-6.99894180139976,4.94565482841703,-15.0596401545356));
#48518=CARTESIAN_POINT('Ctrl Pts',(-6.99873531968,4.88660272557302,-16.0377412505386));
#48519=CARTESIAN_POINT('Ctrl Pts',(-6.99850468875347,5.00216540786785,-17.622209754351));
#48520=CARTESIAN_POINT('Ctrl Pts',(-6.99828080922558,5.43285448097263,-19.3931401195663));
#48521=CARTESIAN_POINT('Ctrl Pts',(-6.99816434197815,6.14885086491948,-21.0703309166242));
#48522=CARTESIAN_POINT('Ctrl Pts',(-6.99814257319851,7.13148866687968,-22.6063548637163));
#48523=CARTESIAN_POINT('Ctrl Pts',(-6.99821546038094,8.25667497594392,-23.8529245372788));
#48524=CARTESIAN_POINT('Ctrl Pts',(-6.99835922376522,9.08279278767221,-24.5356450620554));
#48525=CARTESIAN_POINT('Ctrl Pts',(-6.99838072452425,9.45819126329241,-24.8079421081757));
#48526=CARTESIAN_POINT('',(-7.00000355772625,9.33251603084022,-24.7867164850604));
#48527=CARTESIAN_POINT('Ctrl Pts',(-7.00001601631093,4.92966193678578,-14.796799000993));
#48528=CARTESIAN_POINT('Ctrl Pts',(-7.00002088956044,4.90663940121656,-15.0161851012847));
#48529=CARTESIAN_POINT('Ctrl Pts',(-7.00001598261872,4.89043246190617,-15.2342927807288));
#48530=CARTESIAN_POINT('Ctrl Pts',(-7.00000988115456,4.88069442451672,-15.450630170061));
#48531=CARTESIAN_POINT('Ctrl Pts',(-7.00000652438509,4.87533696510621,-15.5696499207533));
#48532=CARTESIAN_POINT('Ctrl Pts',(-7.00000279083273,4.87193754627854,-15.6881347839494));
#48533=CARTESIAN_POINT('Ctrl Pts',(-6.99999999965565,4.87043898511339,-15.8060095302866));
#48534=CARTESIAN_POINT('Ctrl Pts',(-6.99999455428889,4.86751541025449,-16.035973880696));
#48535=CARTESIAN_POINT('Ctrl Pts',(-6.99999266088529,4.87182596457363,-16.2636132173433));
#48536=CARTESIAN_POINT('Ctrl Pts',(-6.99999257352099,4.88291847944131,-16.4885165155108));
#48537=CARTESIAN_POINT('Ctrl Pts',(-6.99999248489166,4.89417161290698,-16.7166763928098));
#48538=CARTESIAN_POINT('Ctrl Pts',(-6.99999425322773,4.91240450885411,-16.9420204741633));
#48539=CARTESIAN_POINT('Ctrl Pts',(-6.99999619758933,4.93715565208034,-17.1641725428281));
#48540=CARTESIAN_POINT('Ctrl Pts',(-6.9999975442523,4.95429827007814,-17.3180348519641));
#48541=CARTESIAN_POINT('Ctrl Pts',(-6.99999897835725,4.97456787013135,-17.4703670834906));
#48542=CARTESIAN_POINT('Ctrl Pts',(-6.99999998662342,4.99781411395893,-17.6210585462649));
#48543=CARTESIAN_POINT('Ctrl Pts',(-7.00000143707765,5.03125529598881,-17.8378376816109));
#48544=CARTESIAN_POINT('Ctrl Pts',(-7.00000201440503,5.07085505448822,-18.0512192862196));
#48545=CARTESIAN_POINT('Ctrl Pts',(-7.00000210874351,5.11608568717109,-18.2609089713827));
#48546=CARTESIAN_POINT('Ctrl Pts',(-7.00000220459618,5.16204229772174,-18.4739642975174));
#48547=CARTESIAN_POINT('Ctrl Pts',(-7.00000180216116,5.21381197632272,-18.6832082948446));
#48548=CARTESIAN_POINT('Ctrl Pts',(-7.00000129011628,5.27086486939416,-18.8883810460748));
#48549=CARTESIAN_POINT('Ctrl Pts',(-7.00000086166913,5.31860316431548,-19.0600567803058));
#48550=CARTESIAN_POINT('Ctrl Pts',(-7.00000035619187,5.37004082573362,-19.2288830308296));
#48551=CARTESIAN_POINT('Ctrl Pts',(-6.9999999881669,5.42487991567195,-19.3947325990114));
#48552=CARTESIAN_POINT('Ctrl Pts',(-6.99999970373616,5.46726269967022,-19.522910627355));
#48553=CARTESIAN_POINT('Ctrl Pts',(-6.99999950020192,5.51167736194704,-19.649311172218));
#48554=CARTESIAN_POINT('Ctrl Pts',(-6.99999936067801,5.55798420729282,-19.7738901766392));
#48555=CARTESIAN_POINT('Ctrl Pts',(-6.99999924479304,5.59644547829981,-19.8773622835177));
#48556=CARTESIAN_POINT('Ctrl Pts',(-6.99999917321881,5.63621216193175,-19.9795779269211));
#48557=CARTESIAN_POINT('Ctrl Pts',(-6.99999913936905,5.67720658810105,-20.0805154986122));
#48558=CARTESIAN_POINT('Ctrl Pts',(-6.99999912244417,5.69770380118571,-20.1309842844577));
#48559=CARTESIAN_POINT('Ctrl Pts',(-6.99999911499176,5.71850794990473,-20.1811335523751));
#48560=CARTESIAN_POINT('Ctrl Pts',(-6.99999911640478,5.73960956204947,-20.230960959118));
#48561=CARTESIAN_POINT('Ctrl Pts',(-6.99999911711129,5.75016036812184,-20.2558746624894));
#48562=CARTESIAN_POINT('Ctrl Pts',(-6.99999912003637,5.76078554005064,-20.2807079005672));
#48563=CARTESIAN_POINT('Ctrl Pts',(-6.99999912511632,5.77148390014131,-20.3054603897257));
#48564=CARTESIAN_POINT('Ctrl Pts',(-6.9999991276563,5.77683308018664,-20.3178366343049));
#48565=CARTESIAN_POINT('Ctrl Pts',(-6.99999913073513,5.78220055727244,-20.3301926916542));
#48566=CARTESIAN_POINT('Ctrl Pts',(-6.99999913434553,5.78758618501739,-20.3425285275642));
#48567=CARTESIAN_POINT('Ctrl Pts',(-6.99999913750175,5.79229430807622,-20.3533125320013));
#48568=CARTESIAN_POINT('Ctrl Pts',(-6.9999991405722,5.79641055093021,-20.3627040187471));
#48569=CARTESIAN_POINT('Ctrl Pts',(-6.99999914483738,5.8015232455565,-20.3743145538044));
#48570=CARTESIAN_POINT('Ctrl Pts',(-6.99999914545115,5.80225896858769,-20.375985324048));
#48571=CARTESIAN_POINT('Ctrl Pts',(-6.9999991460916,5.80301540493209,-20.3777020105704));
#48572=CARTESIAN_POINT('Ctrl Pts',(-6.99999914676467,5.80379737409617,-20.379475337135));
#48573=CARTESIAN_POINT('Ctrl Pts',(-6.99999923697453,5.90860230533353,-20.6171488634125));
#48574=CARTESIAN_POINT('Ctrl Pts',(-6.9999995214453,6.02101278168188,-20.8492787963373));
#48575=CARTESIAN_POINT('Ctrl Pts',(-6.99999999018456,6.14041872174611,-21.0754662956648));
#48576=CARTESIAN_POINT('Ctrl Pts',(-7.00000044364536,6.25593264860106,-21.2942812577912));
#48577=CARTESIAN_POINT('Ctrl Pts',(-7.00000106797376,6.37799274547658,-21.5075353975042));
#48578=CARTESIAN_POINT('Ctrl Pts',(-7.00000142593565,6.50595991927143,-21.7149354344823));
#48579=CARTESIAN_POINT('Ctrl Pts',(-7.00000178766098,6.63527247524171,-21.9245159706046));
#48580=CARTESIAN_POINT('Ctrl Pts',(-7.00000187627602,6.77061697952042,-22.1281187040794));
#48581=CARTESIAN_POINT('Ctrl Pts',(-7.00000131558935,6.91136695665694,-22.3254829114096));
#48582=CARTESIAN_POINT('Ctrl Pts',(-7.00000103872994,6.98086737080238,-22.4229386583022));
#48583=CARTESIAN_POINT('Ctrl Pts',(-7.00000060480719,7.05168627710489,-22.5188739333697));
#48584=CARTESIAN_POINT('Ctrl Pts',(-6.99999997635806,7.12375115357989,-22.6132610028137));
#48585=CARTESIAN_POINT('Ctrl Pts',(-6.99999887928565,7.24955351900321,-22.7780308210977));
#48586=CARTESIAN_POINT('Ctrl Pts',(-6.99999719588034,7.37915178875968,-22.938081812605));
#48587=CARTESIAN_POINT('Ctrl Pts',(-6.99999590265529,7.51215857783395,-23.0933374643164));
#48588=CARTESIAN_POINT('Ctrl Pts',(-6.99999568173125,7.53488037422716,-23.1198600751669));
#48589=CARTESIAN_POINT('Ctrl Pts',(-6.99999546003663,7.55895243512824,-23.1476964012996));
#48590=CARTESIAN_POINT('Ctrl Pts',(-6.99999525389908,7.58352724378226,-23.1758128231261));
#48591=CARTESIAN_POINT('Ctrl Pts',(-6.99999512031325,7.5994527562614,-23.1940334503127));
#48592=CARTESIAN_POINT('Ctrl Pts',(-6.99999499325438,7.61558863734904,-23.2123723370691));
#48593=CARTESIAN_POINT('Ctrl Pts',(-6.99999487632633,7.63169526645205,-23.2305558840532));
#48594=CARTESIAN_POINT('Ctrl Pts',(-6.99999457896547,7.67265618698126,-23.2767986340535));
#48595=CARTESIAN_POINT('Ctrl Pts',(-6.9999943432934,7.71387538342522,-23.3225491432378));
#48596=CARTESIAN_POINT('Ctrl Pts',(-6.99999419422085,7.75533955273339,-23.3678076333183));
#48597=CARTESIAN_POINT('Ctrl Pts',(-6.99999365475326,7.90539115674498,-23.5315902230827));
#48598=CARTESIAN_POINT('Ctrl Pts',(-6.99999426201921,8.05865167046422,-23.6889299522383));
#48599=CARTESIAN_POINT('Ctrl Pts',(-6.99999708882611,8.21454310880251,-23.8398765708448));
#48600=CARTESIAN_POINT('Ctrl Pts',(-6.99999738657627,8.23096329713509,-23.8557759167749));
#48601=CARTESIAN_POINT('Ctrl Pts',(-6.99999770879859,8.2474127126713,-23.8716043620776));
#48602=CARTESIAN_POINT('Ctrl Pts',(-6.9999980566388,8.26389070674912,-23.8873619847489));
#48603=CARTESIAN_POINT('Ctrl Pts',(-6.99999863108762,8.29110367429903,-23.913385278142));
#48604=CARTESIAN_POINT('Ctrl Pts',(-6.99999927541382,8.31839458405079,-23.9392154108886));
#48605=CARTESIAN_POINT('Ctrl Pts',(-6.99999999465517,8.34576054507866,-23.964852756693));
#48606=CARTESIAN_POINT('Ctrl Pts',(-7.00000393353144,8.49562836482666,-24.1052539330275));
#48607=CARTESIAN_POINT('Ctrl Pts',(-7.0000100648746,8.64774332432774,-24.2398711438475));
#48608=CARTESIAN_POINT('Ctrl Pts',(-7.00001375756538,8.801556306293,-24.3687673244932));
#48609=CARTESIAN_POINT('Ctrl Pts',(-7.00001750474233,8.95763882034422,-24.4995653863326));
#48610=CARTESIAN_POINT('Ctrl Pts',(-7.00001874207225,9.11546988079917,-24.6244724111923));
#48611=CARTESIAN_POINT('Ctrl Pts',(-7.00001328548767,9.27452274288354,-24.7435795241592));
#48612=CARTESIAN_POINT('Ctrl Pts',(-7.00001262288462,9.29383682270603,-24.7580429186377));
#48613=CARTESIAN_POINT('Ctrl Pts',(-7.00001186234282,9.31316897447241,-24.7724208189439));
#48614=CARTESIAN_POINT('Ctrl Pts',(-7.00001099700068,9.33251830079054,-24.78671341245));
#48615=CARTESIAN_POINT('',(-6.271594443024,8.76071211955143,-25.5608538793675));
#48616=CARTESIAN_POINT('Origin',(-5.99998362343976,9.33252812935656,-24.7867137526282));
#48617=CARTESIAN_POINT('Ctrl Pts',(-6.26386059972761,3.90573753010371,-15.8144217562401));
#48618=CARTESIAN_POINT('Ctrl Pts',(-6.26455151911071,3.90327937979186,-16.055503426337));
#48619=CARTESIAN_POINT('Ctrl Pts',(-6.26520985433926,3.90810428962811,-16.2942778967187));
#48620=CARTESIAN_POINT('Ctrl Pts',(-6.26583560602987,3.91978334776613,-16.530318334847));
#48621=CARTESIAN_POINT('Ctrl Pts',(-6.26647065912245,3.93163600769524,-16.7698673643654));
#48622=CARTESIAN_POINT('Ctrl Pts',(-6.26707215281053,3.95054807030025,-17.0066005232977));
#48623=CARTESIAN_POINT('Ctrl Pts',(-6.26764008773865,3.97607950396293,-17.2401251768554));
#48624=CARTESIAN_POINT('Ctrl Pts',(-6.26812467974631,3.99786426852748,-17.439380716712));
#48625=CARTESIAN_POINT('Ctrl Pts',(-6.26858483962897,4.02446833721895,-17.6363012859027));
#48626=CARTESIAN_POINT('Ctrl Pts',(-6.26902056778702,4.05562321087888,-17.8306725452879));
#48627=CARTESIAN_POINT('Ctrl Pts',(-6.26953467283132,4.09238208773099,-18.060006461558));
#48628=CARTESIAN_POINT('Ctrl Pts',(-6.27001476631168,4.13547469852272,-18.2857906056929));
#48629=CARTESIAN_POINT('Ctrl Pts',(-6.27046084888574,4.18435716611124,-18.5077346484473));
#48630=CARTESIAN_POINT('Ctrl Pts',(-6.27062083230447,4.2018884142141,-18.5873328412233));
#48631=CARTESIAN_POINT('Ctrl Pts',(-6.27077644113038,4.22016459485154,-18.6664375452147));
#48632=CARTESIAN_POINT('Ctrl Pts',(-6.27092767539381,4.23916135873699,-18.7450368123693));
#48633=CARTESIAN_POINT('Ctrl Pts',(-6.2713681556663,4.29449074999043,-18.9739626247259));
#48634=CARTESIAN_POINT('Ctrl Pts',(-6.27177152526386,4.35593088785102,-19.1985969560212));
#48635=CARTESIAN_POINT('Ctrl Pts',(-6.27213778418647,4.42289857276513,-19.418679907426));
#48636=CARTESIAN_POINT('Ctrl Pts',(-6.27250404310909,4.48986625767925,-19.6387628588308));
#48637=CARTESIAN_POINT('Ctrl Pts',(-6.27283319135677,4.56236154960823,-19.8542946369576));
#48638=CARTESIAN_POINT('Ctrl Pts',(-6.27312522892951,4.63982794512282,-20.0650654344146));
#48639=CARTESIAN_POINT('Ctrl Pts',(-6.27334042228337,4.69691050921155,-20.2203758431918));
#48640=CARTESIAN_POINT('Ctrl Pts',(-6.27353526484726,4.75658564368513,-20.372823737172));
#48641=CARTESIAN_POINT('Ctrl Pts',(-6.27370997834722,4.81874467904067,-20.5226549488179));
#48642=CARTESIAN_POINT('Ctrl Pts',(-6.27388469184718,4.8809037143962,-20.6724861604638));
#48643=CARTESIAN_POINT('Ctrl Pts',(-6.27403927628321,4.9455469204707,-20.8197010220538));
#48644=CARTESIAN_POINT('Ctrl Pts',(-6.27417395338137,5.01262254914156,-20.964537762537));
#48645=CARTESIAN_POINT('Ctrl Pts',(-6.27427013810291,5.06052713539966,-21.06797837525));
#48646=CARTESIAN_POINT('Ctrl Pts',(-6.2743561688078,5.10967355132922,-21.1702058670971));
#48647=CARTESIAN_POINT('Ctrl Pts',(-6.27443212626672,5.16004860092251,-21.2713083696084));
#48648=CARTESIAN_POINT('Ctrl Pts',(-6.27457884535597,5.25735282228214,-21.4665975130196));
#48649=CARTESIAN_POINT('Ctrl Pts',(-6.27469165518935,5.361220077299,-21.6616515214675));
#48650=CARTESIAN_POINT('Ctrl Pts',(-6.27477055576686,5.47186344552789,-21.8559685725165));
#48651=CARTESIAN_POINT('Ctrl Pts',(-6.2748486289147,5.5813464977181,-22.048247822344));
#48652=CARTESIAN_POINT('Ctrl Pts',(-6.27489350028957,5.69746436261258,-22.2398055710169));
#48653=CARTESIAN_POINT('Ctrl Pts',(-6.27490516989148,5.82040565000112,-22.4301086125228));
#48654=CARTESIAN_POINT('Ctrl Pts',(-6.27491664590315,5.94130743047287,-22.6172546643983));
#48655=CARTESIAN_POINT('Ctrl Pts',(-6.27489601259132,6.06880817075117,-22.8031873173268));
#48656=CARTESIAN_POINT('Ctrl Pts',(-6.274843269956,6.20306900142315,-22.9873530700936));
#48657=CARTESIAN_POINT('Ctrl Pts',(-6.27479056739024,6.33722783162172,-23.1713789086809));
#48658=CARTESIAN_POINT('Ctrl Pts',(-6.27470580427057,6.47813658315848,-23.3536406777549));
#48659=CARTESIAN_POINT('Ctrl Pts',(-6.27458898059699,6.62593646339166,-23.5335379663002));
#48660=CARTESIAN_POINT('Ctrl Pts',(-6.27454781430459,6.67801814255145,-23.5969301209417));
#48661=CARTESIAN_POINT('Ctrl Pts',(-6.2745026670527,6.73095531727352,-23.6600282253355));
#48662=CARTESIAN_POINT('Ctrl Pts',(-6.27445353882921,6.78475355174986,-23.7228045290797));
#48663=CARTESIAN_POINT('Ctrl Pts',(-6.2743162411642,6.9351024031862,-23.8982442113896));
#48664=CARTESIAN_POINT('Ctrl Pts',(-6.27414785116967,7.09217882866916,-24.0711732887822));
#48665=CARTESIAN_POINT('Ctrl Pts',(-6.27394836858148,7.25599619752528,-24.2410355074747));
#48666=CARTESIAN_POINT('Ctrl Pts',(-6.27375072704948,7.41830167010394,-24.4093300410193));
#48667=CARTESIAN_POINT('Ctrl Pts',(-6.27352256419231,7.58722431676834,-24.5746141115647));
#48668=CARTESIAN_POINT('Ctrl Pts',(-6.27326387975308,7.7627444823766,-24.7363080568393));
#48669=CARTESIAN_POINT('Ctrl Pts',(-6.27300884328111,7.93578946308133,-24.8957217945323));
#48670=CARTESIAN_POINT('Ctrl Pts',(-6.27272413998789,8.11524724760931,-25.0516459606413));
#48671=CARTESIAN_POINT('Ctrl Pts',(-6.27240976962724,8.30106617556184,-25.2034869209588));
#48672=CARTESIAN_POINT('Ctrl Pts',(-6.27215746663657,8.45019814572994,-25.3253493265483));
#48673=CARTESIAN_POINT('Ctrl Pts',(-6.27188605472208,8.60342680986372,-25.4445809859663));
#48674=CARTESIAN_POINT('Ctrl Pts',(-6.27159553375651,8.76070944735753,-25.5608567073952));
#48675=CARTESIAN_POINT('Origin',(-5.999994993362,9.33250915082854,-24.7867196013936));
#48676=CARTESIAN_POINT('',(-5.98852246669543,9.69456809148957,-25.7188096068238));
#48677=CARTESIAN_POINT('Origin',(-5.999994993362,9.33250915082854,-24.7867196013936));
#48678=CARTESIAN_POINT('Origin',(-6.,9.33251101023601,-24.7867243682982));
#48679=CARTESIAN_POINT('Ctrl Pts',(-5.9884183312965,9.69410641344453,-25.7189877462122));
#48680=CARTESIAN_POINT('Ctrl Pts',(-5.98810627248762,9.81679904525013,-25.6713270163599));
#48681=CARTESIAN_POINT('Ctrl Pts',(-5.9872640505538,10.2439466077869,-25.5029619472033));
#48682=CARTESIAN_POINT('Ctrl Pts',(-5.98726405055286,10.7897532290078,-25.2768814422167));
#48683=CARTESIAN_POINT('Ctrl Pts',(-5.98810627251012,11.2108442522874,-25.0938945847795));
#48684=CARTESIAN_POINT('Ctrl Pts',(-5.98841833133919,11.3313022744201,-25.0408390158645));
#48685=CARTESIAN_POINT('Ctrl Pts',(-6.58019637133009,9.69658812787628,-25.7253769286093));
#48686=CARTESIAN_POINT('Ctrl Pts',(-6.57988216396863,9.81936872043664,-25.6778801575558));
#48687=CARTESIAN_POINT('Ctrl Pts',(-6.57903377270813,10.2467760977028,-25.5099484803168));
#48688=CARTESIAN_POINT('Ctrl Pts',(-6.57903377270728,10.7926927024447,-25.2838224186652));
#48689=CARTESIAN_POINT('Ctrl Pts',(-6.57988216399013,11.2136609881125,-25.1003453900946));
#48690=CARTESIAN_POINT('Ctrl Pts',(-6.5801963713722,11.3340652715104,-25.0471116871477));
#48691=CARTESIAN_POINT('Ctrl Pts',(-7.00079676886773,9.54584602334702,-25.3372908808639));
#48692=CARTESIAN_POINT('Ctrl Pts',(-7.00061248422704,9.66739289539033,-25.2904141386208));
#48693=CARTESIAN_POINT('Ctrl Pts',(-7.00011448375567,10.0904742433784,-25.1245686185404));
#48694=CARTESIAN_POINT('Ctrl Pts',(-7.00011448375563,10.6307100898621,-24.9007956040115));
#48695=CARTESIAN_POINT('Ctrl Pts',(-7.0006124842397,11.04714427498,-24.7189024042084));
#48696=CARTESIAN_POINT('Ctrl Pts',(-7.00079676889193,11.1662377596005,-24.666102646838));
#48697=CARTESIAN_POINT('Ctrl Pts',(-6.99999917319659,9.33157252936654,-24.7856430600347));
#48698=CARTESIAN_POINT('Ctrl Pts',(-6.99999957777432,9.45129807495918,-24.7394735073194));
#48699=CARTESIAN_POINT('Ctrl Pts',(-7.00000004362305,9.86804157465028,-24.576125664719));
#48700=CARTESIAN_POINT('Ctrl Pts',(-7.00000004362386,10.4001860063983,-24.3557042239056));
#48701=CARTESIAN_POINT('Ctrl Pts',(-6.99999957777458,10.810372531279,-24.1765264349544));
#48702=CARTESIAN_POINT('Ctrl Pts',(-6.99999917319582,10.9276780850348,-24.1245144913973));
#48703=CARTESIAN_POINT('Origin',(-5.9885235341522,-4.75229019723222,11.4730434407793));
#48704=CARTESIAN_POINT('Origin',(-7.00021006962832,-4.74293597589513,11.4504603050761));
#48705=CARTESIAN_POINT('Ctrl Pts',(-6.05505067660194,9.37215177151571,-25.8432012822673));
#48706=CARTESIAN_POINT('Ctrl Pts',(-4.03670045106797,8.81554919752502,-26.0304401291589));
#48707=CARTESIAN_POINT('Ctrl Pts',(7.61017729489916E-7,8.27058403888204,
-26.2482623545472));
#48708=CARTESIAN_POINT('Ctrl Pts',(4.03670197310351,8.81554940300285,-26.030440047027));
#48709=CARTESIAN_POINT('Ctrl Pts',(6.05505295965479,9.37215240111522,-25.8432010704704));
#48710=CARTESIAN_POINT('Ctrl Pts',(-6.05505067660194,10.1400029312564,-25.5527891512987));
#48711=CARTESIAN_POINT('Ctrl Pts',(-4.03670045106797,9.95059815166984,-25.6069178790708));
#48712=CARTESIAN_POINT('Ctrl Pts',(7.61017729489916E-7,9.8134122476049,
-25.7964932163722));
#48713=CARTESIAN_POINT('Ctrl Pts',(4.03670197310351,9.95059820339512,-25.6069178075902));
#48714=CARTESIAN_POINT('Ctrl Pts',(6.05505295965479,10.1400031454992,-25.552789090066));
#48715=CARTESIAN_POINT('Ctrl Pts',(-6.05505067660194,10.8990942198713,-25.2383558203596));
#48716=CARTESIAN_POINT('Ctrl Pts',(-4.03670045106797,11.0715877475132,-25.1425762612566));
#48717=CARTESIAN_POINT('Ctrl Pts',(7.61017729489916E-7,11.302923524876,
-25.1794671417429));
#48718=CARTESIAN_POINT('Ctrl Pts',(4.03670197310351,11.0715876602892,-25.1425762473493));
#48719=CARTESIAN_POINT('Ctrl Pts',(6.05505295965479,10.8990940247534,-25.2383559286956));
#48720=CARTESIAN_POINT('Ctrl Pts',(-6.05505067660194,11.6473935737486,-24.9007429977581));
#48721=CARTESIAN_POINT('Ctrl Pts',(-4.03670045106797,12.1736538531869,-24.6394300651268));
#48722=CARTESIAN_POINT('Ctrl Pts',(7.61017729489916E-7,12.7132743263768,
-24.4078888772065));
#48723=CARTESIAN_POINT('Ctrl Pts',(4.03670197310351,12.1736536497231,-24.6394301524292));
#48724=CARTESIAN_POINT('Ctrl Pts',(6.05505295965479,11.6473929784695,-24.9007432933403));
#48725=CARTESIAN_POINT('Ctrl Pts',(-5.98852262888393,9.6945676509312,-25.7188097476035));
#48726=CARTESIAN_POINT('Ctrl Pts',(-5.93914474573397,9.67822396126561,-25.7245504584746));
#48727=CARTESIAN_POINT('Ctrl Pts',(-5.88279573294254,9.65973790752962,-25.731062674358));
#48728=CARTESIAN_POINT('Ctrl Pts',(-5.8194048475461,9.63929488404148,-25.7382945464948));
#48729=CARTESIAN_POINT('Ctrl Pts',(-5.75829929143766,9.61958885988725,-25.7452656996167));
#48730=CARTESIAN_POINT('Ctrl Pts',(-5.69065018696235,9.59806460605636,-25.7529056167575));
#48731=CARTESIAN_POINT('Ctrl Pts',(-5.61638362499844,9.57493013737895,-25.7611526723746));
#48732=CARTESIAN_POINT('Ctrl Pts',(-5.54072805329341,9.55136298403837,-25.7695539729209));
#48733=CARTESIAN_POINT('Ctrl Pts',(-5.4582049597275,9.52612458268054,-25.7785855835354));
#48734=CARTESIAN_POINT('Ctrl Pts',(-5.36872850624103,9.49948016899468,-25.7881637857989));
#48735=CARTESIAN_POINT('Ctrl Pts',(-5.3239902794978,9.48615796215175,-25.7929528869306));
#48736=CARTESIAN_POINT('Ctrl Pts',(-5.27751361368163,9.47248497632851,-25.7978783252447));
#48737=CARTESIAN_POINT('Ctrl Pts',(-5.22928736188671,9.45849880618232,-25.8029276205075));
#48738=CARTESIAN_POINT('Ctrl Pts',(-5.20517423598925,9.45150572110923,-25.8054522681389));
#48739=CARTESIAN_POINT('Ctrl Pts',(-5.18062371361782,9.44443433851998,-25.8080078762341));
#48740=CARTESIAN_POINT('Ctrl Pts',(-5.1556343858912,9.43728971218247,-25.8105927199721));
#48741=CARTESIAN_POINT('Ctrl Pts',(-5.13189984629429,9.43050383868607,-25.8130477710532));
#48742=CARTESIAN_POINT('Ctrl Pts',(-5.10666091353175,9.42333916306116,-25.8156425536409));
#48743=CARTESIAN_POINT('Ctrl Pts',(-5.08307503285008,9.41669114214869,-25.8180525556873));
#48744=CARTESIAN_POINT('Ctrl Pts',(-5.08182810396034,9.41633967724275,-25.8181799667098));
#48745=CARTESIAN_POINT('Ctrl Pts',(-5.08058579897438,9.4159896453358,-25.8183068646897));
#48746=CARTESIAN_POINT('Ctrl Pts',(-5.0793485856463,9.41564117510416,-25.8184332028057));
#48747=CARTESIAN_POINT('Ctrl Pts',(-5.06433554013984,9.41141264043952,-25.8199662608815));
#48748=CARTESIAN_POINT('Ctrl Pts',(-5.04943318284293,9.40723478799857,-25.8214818625031));
#48749=CARTESIAN_POINT('Ctrl Pts',(-5.03464184081241,9.40310682556614,-25.8229802157136));
#48750=CARTESIAN_POINT('Ctrl Pts',(-4.91702209302933,9.37028154851154,-25.834895018734));
#48751=CARTESIAN_POINT('Ctrl Pts',(-4.80642474277852,9.34060758757959,-25.8457196403818));
#48752=CARTESIAN_POINT('Ctrl Pts',(-4.70298901843753,9.31371271080518,-25.8555634948917));
#48753=CARTESIAN_POINT('Ctrl Pts',(-4.59988946245336,9.28690524296602,-25.86537535666));
#48754=CARTESIAN_POINT('Ctrl Pts',(-4.50390474764424,9.26285864773517,-25.8742130202874));
#48755=CARTESIAN_POINT('Ctrl Pts',(-4.41514468579301,9.24124704046678,-25.8821770968963));
#48756=CARTESIAN_POINT('Ctrl Pts',(-4.38360632789255,9.23356797185621,-25.8850069045057));
#48757=CARTESIAN_POINT('Ctrl Pts',(-4.35297986988857,9.22619673491393,-25.8877263331032));
#48758=CARTESIAN_POINT('Ctrl Pts',(-4.32326948852073,9.21912007669597,-25.8903395887858));
#48759=CARTESIAN_POINT('Ctrl Pts',(-4.2886422544966,9.21087228286294,-25.8933853193325));
#48760=CARTESIAN_POINT('Ctrl Pts',(-4.25525940683351,9.20302460535569,-25.8962868365517));
#48761=CARTESIAN_POINT('Ctrl Pts',(-4.22312693641565,9.19555734174392,-25.8990504778776));
#48762=CARTESIAN_POINT('Ctrl Pts',(-4.20706070120673,9.19182370993804,-25.9004322985405));
#48763=CARTESIAN_POINT('Ctrl Pts',(-4.19130706030953,9.18818518239483,-25.9017796523655));
#48764=CARTESIAN_POINT('Ctrl Pts',(-4.17586669145764,9.18463945126438,-25.9030932880816));
#48765=CARTESIAN_POINT('Ctrl Pts',(-4.1681465070317,9.18286658569916,-25.9037501059396));
#48766=CARTESIAN_POINT('Ctrl Pts',(-4.16050464061708,9.18111691928206,-25.9043984943918));
#48767=CARTESIAN_POINT('Ctrl Pts',(-4.15294117518514,9.17939016816571,-25.9050385461194));
#48768=CARTESIAN_POINT('Ctrl Pts',(-4.14915944246918,9.17852679260754,-25.9053585719832));
#48769=CARTESIAN_POINT('Ctrl Pts',(-4.14539730999889,9.17766914587717,-25.9056765136729));
#48770=CARTESIAN_POINT('Ctrl Pts',(-4.14165478791372,9.17681719302608,-25.9059923826253));
#48771=CARTESIAN_POINT('Ctrl Pts',(-4.13978352687113,9.17639121660053,-25.9061503171014));
#48772=CARTESIAN_POINT('Ctrl Pts',(-4.13791716842483,9.17596666364496,-25.9063077333937));
#48773=CARTESIAN_POINT('Ctrl Pts',(-4.13605571382735,9.1755435298259,-25.9064646329216));
#48774=CARTESIAN_POINT('Ctrl Pts',(-4.13419425922987,9.17512039600684,-25.9066215324495));
#48775=CARTESIAN_POINT('Ctrl Pts',(-4.1340901684656,9.17509646730814,-25.9066303970282));
#48776=CARTESIAN_POINT('Ctrl Pts',(-4.13048606282949,9.17427838145572,-25.9069337826298));
#48777=CARTESIAN_POINT('Ctrl Pts',(-4.08691193609688,9.16438761236891,-25.9106017557657));
#48778=CARTESIAN_POINT('Ctrl Pts',(-4.04447551159814,9.15491120120482,-25.9141211943608));
#48779=CARTESIAN_POINT('Ctrl Pts',(-4.00318382525737,9.1458261516899,-25.9174993986425));
#48780=CARTESIAN_POINT('Ctrl Pts',(-3.90005318180312,9.12313521592729,-25.9259368448254));
#48781=CARTESIAN_POINT('Ctrl Pts',(-3.80406510638285,9.10288246048144,-25.9334941271089));
#48782=CARTESIAN_POINT('Ctrl Pts',(-3.71531264401003,9.08473979632614,-25.9402797321664));
#48783=CARTESIAN_POINT('Ctrl Pts',(-3.62707651135985,9.06670267962835,-25.9470258610281));
#48784=CARTESIAN_POINT('Ctrl Pts',(-3.54599178209802,9.05075106996483,-25.9530093831139));
#48785=CARTESIAN_POINT('Ctrl Pts',(-3.4721292247771,9.03660782871565,-25.9583241854749));
#48786=CARTESIAN_POINT('Ctrl Pts',(-3.4138364983745,9.02544590686393,-25.9625186560044));
#48787=CARTESIAN_POINT('Ctrl Pts',(-3.36004163323143,9.01541118372412,-25.9662963853087));
#48788=CARTESIAN_POINT('Ctrl Pts',(-3.31077175302537,9.00638811719138,-25.9696972084536));
#48789=CARTESIAN_POINT('Ctrl Pts',(-3.27749897070262,9.00029468795283,-25.9719938417668));
#48790=CARTESIAN_POINT('Ctrl Pts',(-3.2462896846622,8.99466300700617,-25.9741184688898));
#48791=CARTESIAN_POINT('Ctrl Pts',(-3.21715071744293,8.98946236732531,-25.9760817903242));
#48792=CARTESIAN_POINT('Ctrl Pts',(-3.20258123383329,8.98686204748487,-25.9770634510415));
#48793=CARTESIAN_POINT('Ctrl Pts',(-3.18852932993462,8.98436948858393,-25.9780047870712));
#48794=CARTESIAN_POINT('Ctrl Pts',(-3.17499573175916,8.98198129761811,-25.9789069868615));
#48795=CARTESIAN_POINT('Ctrl Pts',(-3.16822893267142,8.98078720213521,-25.9793580867567));
#48796=CARTESIAN_POINT('Ctrl Pts',(-3.16159171001477,8.97961919866815,-25.9797994026812));
#48797=CARTESIAN_POINT('Ctrl Pts',(-3.15508415158759,8.97847687591692,-25.980231079151));
#48798=CARTESIAN_POINT('Ctrl Pts',(-3.15183037237399,8.97790571454131,-25.9804469173859));
#48799=CARTESIAN_POINT('Ctrl Pts',(-3.14860900921778,8.97734097334633,-25.9806603457618));
#48800=CARTESIAN_POINT('Ctrl Pts',(-3.14542007266562,8.97678260251498,-25.9808713818034));
#48801=CARTESIAN_POINT('Ctrl Pts',(-3.14223113611345,8.97622423168362,-25.9810824178449));
#48802=CARTESIAN_POINT('Ctrl Pts',(-3.13737712858202,8.97537573052988,-25.9814031398511));
#48803=CARTESIAN_POINT('Ctrl Pts',(-3.13595055324389,8.97512655178081,-25.9814973302948));
#48804=CARTESIAN_POINT('Ctrl Pts',(-3.12014621626011,8.97236602114898,-25.982540820585));
#48805=CARTESIAN_POINT('Ctrl Pts',(-3.09726105140332,8.96836944993973,-25.9840516043252));
#48806=CARTESIAN_POINT('Ctrl Pts',(-3.06727915898629,8.96321423979775,-25.9860020089781));
#48807=CARTESIAN_POINT('Ctrl Pts',(-3.03741246016798,8.95807883651785,-25.9879449199702));
#48808=CARTESIAN_POINT('Ctrl Pts',(-3.00050338114547,8.9517936639778,-25.9903241089074));
#48809=CARTESIAN_POINT('Ctrl Pts',(-2.95652740131304,8.94448308321903,-25.9930947938812));
#48810=CARTESIAN_POINT('Ctrl Pts',(-2.93861217939317,8.94150485107604,-25.9942235336243));
#48811=CARTESIAN_POINT('Ctrl Pts',(-2.91952401304476,8.93835699328653,-25.9954170434176));
#48812=CARTESIAN_POINT('Ctrl Pts',(-2.89926087786538,8.93505022264859,-25.9966714405561));
#48813=CARTESIAN_POINT('Ctrl Pts',(-2.84967927921722,8.92695892911775,-25.9997408083968));
#48814=CARTESIAN_POINT('Ctrl Pts',(-2.79306320428941,8.91791283508941,-26.0031759944465));
#48815=CARTESIAN_POINT('Ctrl Pts',(-2.72937889204199,8.90810252116344,-26.0069075036621));
#48816=CARTESIAN_POINT('Ctrl Pts',(-2.66611328203675,8.89835670664544,-26.0106144795002));
#48817=CARTESIAN_POINT('Ctrl Pts',(-2.59587189772266,8.88785667520502,-26.0146139373803));
#48818=CARTESIAN_POINT('Ctrl Pts',(-2.51861771041027,8.87683697547256,-26.0188193598197));
#48819=CARTESIAN_POINT('Ctrl Pts',(-2.46588274151833,8.86931474861592,-26.0216900498009));
#48820=CARTESIAN_POINT('Ctrl Pts',(-2.40987996642888,8.86155135889636,-26.0246563335322));
#48821=CARTESIAN_POINT('Ctrl Pts',(-2.35059722894411,8.85363439251256,-26.0276855409131));
#48822=CARTESIAN_POINT('Ctrl Pts',(-2.31881048549239,8.84938940332962,-26.0293097681665));
#48823=CARTESIAN_POINT('Ctrl Pts',(-2.28608075625419,8.84510044232466,-26.03095201316));
#48824=CARTESIAN_POINT('Ctrl Pts',(-2.25240618731547,8.84078228822473,-26.0326067213317));
#48825=CARTESIAN_POINT('Ctrl Pts',(-2.23556890284611,8.83862321117477,-26.0334340754176));
#48826=CARTESIAN_POINT('Ctrl Pts',(-2.21849540844796,8.83645683557932,-26.034264544514));
#48827=CARTESIAN_POINT('Ctrl Pts',(-2.20118547662363,8.8342851098282,-26.0350973937513));
#48828=CARTESIAN_POINT('Ctrl Pts',(-2.19253051071147,8.83319924695263,-26.03551381837));
#48829=CARTESIAN_POINT('Ctrl Pts',(-2.18381643544252,8.83211204652001,-26.0359308379717));
#48830=CARTESIAN_POINT('Ctrl Pts',(-2.175043222636,8.83102375488626,-26.0363483593618));
#48831=CARTESIAN_POINT('Ctrl Pts',(-2.16846331303111,8.83020753616095,-26.0366615004044));
#48832=CARTESIAN_POINT('Ctrl Pts',(-2.16185013856133,8.82939070363346,-26.0369749236986));
#48833=CARTESIAN_POINT('Ctrl Pts',(-2.15520368740763,8.82857336242411,-26.0372885894234));
#48834=CARTESIAN_POINT('Ctrl Pts',(-2.15298820368973,8.82830091535433,-26.0373931446651));
#48835=CARTESIAN_POINT('Ctrl Pts',(-2.14946255515765,8.82786822056567,-26.0375592085574));
#48836=CARTESIAN_POINT('Ctrl Pts',(-2.14854614359539,8.82775585565574,-26.0376023344423));
#48837=CARTESIAN_POINT('Ctrl Pts',(-2.0128572772243,8.81111849764294,-26.0439877868723));
#48838=CARTESIAN_POINT('Ctrl Pts',(-1.87311902758234,8.79563658753315,-26.0499557569825));
#48839=CARTESIAN_POINT('Ctrl Pts',(-1.72934488860467,8.78158234860393,-26.055398450122));
#48840=CARTESIAN_POINT('Ctrl Pts',(-1.55033452067602,8.76408369064244,-26.0621750408801));
#48841=CARTESIAN_POINT('Ctrl Pts',(-1.36506673402777,8.74879789740494,-26.0681381321527));
#48842=CARTESIAN_POINT('Ctrl Pts',(-1.17358540971037,8.73625506698945,-26.0730583965713));
#48843=CARTESIAN_POINT('Ctrl Pts',(-0.995034403883234,8.72455922670536,
-26.0776464062063));
#48844=CARTESIAN_POINT('Ctrl Pts',(-0.811080758346082,8.7152487315044,-26.0813275280306));
#48845=CARTESIAN_POINT('Ctrl Pts',(-0.621784930566627,8.7087784386549,-26.0838952427685));
#48846=CARTESIAN_POINT('Ctrl Pts',(-0.437450969383238,8.70247774663777,
-26.086395651966));
#48847=CARTESIAN_POINT('Ctrl Pts',(-0.248049563901548,8.69887060590274,
-26.0878396659788));
#48848=CARTESIAN_POINT('Ctrl Pts',(-0.0537262494172971,8.69839152673885,
-26.0880418643833));
#48849=CARTESIAN_POINT('Ctrl Pts',(0.0580379594840133,8.69811598644203,
-26.0881581579159));
#48850=CARTESIAN_POINT('Ctrl Pts',(0.171429490699651,8.69887554117705,-26.0878634374378));
#48851=CARTESIAN_POINT('Ctrl Pts',(0.286413558273367,8.70075569448962,-26.0871205175796));
#48852=CARTESIAN_POINT('Ctrl Pts',(0.308600630279844,8.7011184847249,-26.0869771654027));
#48853=CARTESIAN_POINT('Ctrl Pts',(0.330846980306243,8.70152300397326,-26.0868171213266));
#48854=CARTESIAN_POINT('Ctrl Pts',(0.353152334505659,8.70196987549253,-26.086640112036));
#48855=CARTESIAN_POINT('Ctrl Pts',(0.48453063270388,8.70460194397212,-26.0855975292031));
#48856=CARTESIAN_POINT('Ctrl Pts',(0.617956407365337,8.70870289305593,-26.0839663359402));
#48857=CARTESIAN_POINT('Ctrl Pts',(0.753387312203915,8.71441095614992,-26.081705841676));
#48858=CARTESIAN_POINT('Ctrl Pts',(0.832599466679027,8.71774954401577,-26.080383701644));
#48859=CARTESIAN_POINT('Ctrl Pts',(0.912497509964033,8.72163786730543,-26.0788463388806));
#48860=CARTESIAN_POINT('Ctrl Pts',(0.993071857462417,8.72610454453892,-26.0770856585089));
#48861=CARTESIAN_POINT('Ctrl Pts',(1.03335903121161,8.72833788315566,-26.076205318323));
#48862=CARTESIAN_POINT('Ctrl Pts',(1.07381528101382,8.73071581154904,-26.0752691526353));
#48863=CARTESIAN_POINT('Ctrl Pts',(1.11443933439587,8.73324193498107,-26.0742761670545));
#48864=CARTESIAN_POINT('Ctrl Pts',(1.1347513610869,8.73450499669708,-26.073779674264));
#48865=CARTESIAN_POINT('Ctrl Pts',(1.15510533867405,8.73580510725891,-26.0732689767542));
#48866=CARTESIAN_POINT('Ctrl Pts',(1.17550110474873,8.73714272111241,-26.0727439506748));
#48867=CARTESIAN_POINT('Ctrl Pts',(1.18569898778607,8.73781152803917,-26.0724814376351));
#48868=CARTESIAN_POINT('Ctrl Pts',(1.19590731794535,8.73848971079429,-26.0722153424692));
#48869=CARTESIAN_POINT('Ctrl Pts',(1.20612607461619,8.73917732641975,-26.0719456497258));
#48870=CARTESIAN_POINT('Ctrl Pts',(1.21003384007692,8.73944027823257,-26.0718425162408));
#48871=CARTESIAN_POINT('Ctrl Pts',(1.21394313029209,8.73970460947776,-26.0717388566579));
#48872=CARTESIAN_POINT('Ctrl Pts',(1.21785394410087,8.7399703233597,-26.071634670111));
#48873=CARTESIAN_POINT('Ctrl Pts',(1.21905649432309,8.74005202867819,-26.0716026334144));
#48874=CARTESIAN_POINT('Ctrl Pts',(1.22025918860458,8.7401338647282,-26.0715705468922));
#48875=CARTESIAN_POINT('Ctrl Pts',(1.22146202691165,8.74021583159409,-26.0715384105174));
#48876=CARTESIAN_POINT('Ctrl Pts',(1.22401932140998,8.74039009725719,-26.0714700869745));
#48877=CARTESIAN_POINT('Ctrl Pts',(1.2265772669166,8.74056495423914,-26.0714015380865));
#48878=CARTESIAN_POINT('Ctrl Pts',(1.22913586310785,8.7407404033154,-26.0713327636059));
#48879=CARTESIAN_POINT('Ctrl Pts',(1.2316944592991,8.74091585239167,-26.0712639891253));
#48880=CARTESIAN_POINT('Ctrl Pts',(1.23563112013739,8.741186935779,-26.0711577403777));
#48881=CARTESIAN_POINT('Ctrl Pts',(1.23681360340992,8.74126852767454,-26.0711257631143));
#48882=CARTESIAN_POINT('Ctrl Pts',(1.30415700015864,8.74591525335826,-26.0693046316134));
#48883=CARTESIAN_POINT('Ctrl Pts',(1.37864975928608,8.75145208437293,-26.0671401719801));
#48884=CARTESIAN_POINT('Ctrl Pts',(1.46026019920768,8.75813439531587,-26.0645364370334));
#48885=CARTESIAN_POINT('Ctrl Pts',(1.54192310568886,8.76482100225165,-26.0619310281708));
#48886=CARTESIAN_POINT('Ctrl Pts',(1.63071306962372,8.7726546079288,-26.058885709424));
#48887=CARTESIAN_POINT('Ctrl Pts',(1.72658512627508,8.78193883475825,-26.0552879837732));
#48888=CARTESIAN_POINT('Ctrl Pts',(1.81123511500212,8.79013631923811,-26.0521113810548));
#48889=CARTESIAN_POINT('Ctrl Pts',(1.90140620465113,8.79946541363449,-26.0485038513462));
#48890=CARTESIAN_POINT('Ctrl Pts',(1.99705663527059,8.81016555726613,-26.0443780748945));
#48891=CARTESIAN_POINT('Ctrl Pts',(2.10633112278669,8.82238978567916,-26.0396646396862));
#48892=CARTESIAN_POINT('Ctrl Pts',(2.22275768465182,8.83640277908269,-26.0342749055327));
#48893=CARTESIAN_POINT('Ctrl Pts',(2.34625422416244,8.85260251429612,-26.0280670817374));
#48894=CARTESIAN_POINT('Ctrl Pts',(2.46249286483808,8.86785019012556,-26.0222240921089));
#48895=CARTESIAN_POINT('Ctrl Pts',(2.58499495411797,8.88503560594046,-26.0156561357011));
#48896=CARTESIAN_POINT('Ctrl Pts',(2.71367114820033,8.90452607693472,-26.0082356891927));
#48897=CARTESIAN_POINT('Ctrl Pts',(2.74257980920367,8.90890484662702,-26.006568596269));
#48898=CARTESIAN_POINT('Ctrl Pts',(2.77180000596921,8.91340009384957,-26.0048584431687));
#48899=CARTESIAN_POINT('Ctrl Pts',(2.80133057639793,8.91801616406612,-26.0031037454239));
#48900=CARTESIAN_POINT('Ctrl Pts',(2.82674886760609,8.92198942348165,-26.0015933980919));
#48901=CARTESIAN_POINT('Ctrl Pts',(2.85519251276494,8.92649299991863,-25.9998825579851));
#48902=CARTESIAN_POINT('Ctrl Pts',(2.88386923276027,8.93110569654494,-25.9981317011542));
#48903=CARTESIAN_POINT('Ctrl Pts',(2.89904594651544,8.93354689541107,-25.9972050870591));
#48904=CARTESIAN_POINT('Ctrl Pts',(2.91428808430034,8.93601787623561,-25.9962675472531));
#48905=CARTESIAN_POINT('Ctrl Pts',(2.92918279413114,8.93845060795178,-25.9953448837206));
#48906=CARTESIAN_POINT('Ctrl Pts',(3.02452062843766,8.95402200047323,-25.989439112881));
#48907=CARTESIAN_POINT('Ctrl Pts',(3.11288301577595,8.96919620282964,-25.9836990070561));
#48908=CARTESIAN_POINT('Ctrl Pts',(3.1943190206272,8.98368049199339,-25.9782314355906));
#48909=CARTESIAN_POINT('Ctrl Pts',(3.25134055044255,8.99382239824129,-25.9744030394174));
#48910=CARTESIAN_POINT('Ctrl Pts',(3.30496622924687,9.0036270924581,-25.9707078341751));
#48911=CARTESIAN_POINT('Ctrl Pts',(3.35521234116732,9.01300818178171,-25.9671769151241));
#48912=CARTESIAN_POINT('Ctrl Pts',(3.42777531237928,9.02655589101746,-25.9620777349557));
#48913=CARTESIAN_POINT('Ctrl Pts',(3.49329027393557,9.03921804241095,-25.9573219778677));
#48914=CARTESIAN_POINT('Ctrl Pts',(3.5518024689862,9.05077578986301,-25.9529875386592));
#48915=CARTESIAN_POINT('Ctrl Pts',(3.6106020683201,9.06239030746564,-25.9486318092498));
#48916=CARTESIAN_POINT('Ctrl Pts',(3.66233009124901,9.07288959914803,-25.9447014803238));
#48917=CARTESIAN_POINT('Ctrl Pts',(3.70702540622173,9.08210053382569,-25.9412572827147));
#48918=CARTESIAN_POINT('Ctrl Pts',(3.75194675858638,9.09135805091702,-25.9377956667823));
#48919=CARTESIAN_POINT('Ctrl Pts',(3.78976421224823,9.09931417924152,-25.9348250627982));
#48920=CARTESIAN_POINT('Ctrl Pts',(3.82050805513342,9.10584182648722,-25.9323895408546));
#48921=CARTESIAN_POINT('Ctrl Pts',(3.82703720645496,9.10722812021764,-25.9318723026104));
#48922=CARTESIAN_POINT('Ctrl Pts',(3.83324728642847,9.10855015939838,-25.9313791362946));
#48923=CARTESIAN_POINT('Ctrl Pts',(3.83913852491444,9.10980700565233,-25.9309103654691));
#48924=CARTESIAN_POINT('Ctrl Pts',(3.85140011662712,9.11242291326637,-25.9299347002532));
#48925=CARTESIAN_POINT('Ctrl Pts',(3.86228053968236,9.11475629400514,-25.9290647547988));
#48926=CARTESIAN_POINT('Ctrl Pts',(3.87178155207577,9.11680004991352,-25.928302970545));
#48927=CARTESIAN_POINT('Ctrl Pts',(3.87653205827248,9.11782192786771,-25.9279220784181));
#48928=CARTESIAN_POINT('Ctrl Pts',(3.88093771180439,9.118771399769,-25.9275682270146));
#48929=CARTESIAN_POINT('Ctrl Pts',(3.88499868405716,9.11964778216551,-25.9272416501901));
#48930=CARTESIAN_POINT('Ctrl Pts',(3.88702917018354,9.12008597336377,-25.9270783617778));
#48931=CARTESIAN_POINT('Ctrl Pts',(3.88897348599018,9.12050589219657,-25.9269218920397));
#48932=CARTESIAN_POINT('Ctrl Pts',(3.89083165147538,9.12090745887444,-25.9267722683545));
#48933=CARTESIAN_POINT('Ctrl Pts',(3.89176073421798,9.12110824221338,-25.9266974565119));
#48934=CARTESIAN_POINT('Ctrl Pts',(3.89266827938022,9.1213044375143,-25.9266243561845));
#48935=CARTESIAN_POINT('Ctrl Pts',(3.89355428929539,9.12149603549233,-25.9265529705566));
#48936=CARTESIAN_POINT('Ctrl Pts',(3.89399729425297,9.12159183448135,-25.9265172777426));
#48937=CARTESIAN_POINT('Ctrl Pts',(3.89443491538337,9.12168648420069,-25.9264820135827));
#48938=CARTESIAN_POINT('Ctrl Pts',(3.89486446310959,9.12177940075376,-25.926447395576));
#48939=CARTESIAN_POINT('Ctrl Pts',(3.89529401083581,9.12187231730682,-25.9264127775693));
#48940=CARTESIAN_POINT('Ctrl Pts',(3.89572088354979,9.12196459230373,-25.9263783968016));
#48941=CARTESIAN_POINT('Ctrl Pts',(3.89744543978842,9.12233787339604,-25.9262393301259));
#48942=CARTESIAN_POINT('Ctrl Pts',(3.90615289557581,9.12422260671741,-25.925537168664));
#48943=CARTESIAN_POINT('Ctrl Pts',(3.91484190872599,9.12610953954907,-25.9248343676433));
#48944=CARTESIAN_POINT('Ctrl Pts',(3.92351248770352,9.12799859659242,-25.9241309558179));
#48945=CARTESIAN_POINT('Ctrl Pts',(4.08352426246704,9.16286032507885,-25.9111497956376));
#48946=CARTESIAN_POINT('Ctrl Pts',(4.23725682874554,9.19844174260805,-25.8979626235783));
#48947=CARTESIAN_POINT('Ctrl Pts',(4.38477077120115,9.23429180559824,-25.884741517799));
#48948=CARTESIAN_POINT('Ctrl Pts',(4.40473563112835,9.2391438316106,-25.8829521443976));
#48949=CARTESIAN_POINT('Ctrl Pts',(4.42458659941958,9.24400084552466,-25.881162113865));
#48950=CARTESIAN_POINT('Ctrl Pts',(4.44432384241613,9.2488617915148,-25.8793718199261));
#48951=CARTESIAN_POINT('Ctrl Pts',(4.59308111662287,9.28549816852476,-25.8658785855147));
#48952=CARTESIAN_POINT('Ctrl Pts',(4.7353774875914,9.32235418178061,-25.8523724581803));
#48953=CARTESIAN_POINT('Ctrl Pts',(4.87128883464031,9.35900449074716,-25.839012128568));
#48954=CARTESIAN_POINT('Ctrl Pts',(4.89544337741269,9.36551808563659,-25.836637693614));
#48955=CARTESIAN_POINT('Ctrl Pts',(4.91939626929584,9.37202529808466,-25.834267800704));
#48956=CARTESIAN_POINT('Ctrl Pts',(4.94314796326917,9.37852388795739,-25.8319032604887));
#48957=CARTESIAN_POINT('Ctrl Pts',(5.07995159413634,9.41595408940341,-25.8182841187488));
#48958=CARTESIAN_POINT('Ctrl Pts',(5.21008001283661,9.45309456680969,-25.8048447024304));
#48959=CARTESIAN_POINT('Ctrl Pts',(5.33362132246346,9.48954685475107,-25.791729222239));
#48960=CARTESIAN_POINT('Ctrl Pts',(5.36980640846317,9.50022368161998,-25.787887715458));
#48961=CARTESIAN_POINT('Ctrl Pts',(5.40542642866001,9.51084176427358,-25.7840738287903));
#48962=CARTESIAN_POINT('Ctrl Pts',(5.44048367932467,9.52139181573028,-25.7802907760697));
#48963=CARTESIAN_POINT('Ctrl Pts',(5.56340767817423,9.55838429199524,-25.7670259603906));
#48964=CARTESIAN_POINT('Ctrl Pts',(5.67941229471595,9.59453689009802,-25.7541423866658));
#48965=CARTESIAN_POINT('Ctrl Pts',(5.78859480714337,9.62948272158884,-25.7417662950012));
#48966=CARTESIAN_POINT('Ctrl Pts',(5.8424005745087,9.6467042274672,-25.7356672861563));
#48967=CARTESIAN_POINT('Ctrl Pts',(5.89454960227653,9.66363335678642,-25.7296910961071));
#48968=CARTESIAN_POINT('Ctrl Pts',(5.94505368243246,9.68023019451297,-25.7238505128447));
#48969=CARTESIAN_POINT('Ctrl Pts',(5.95968231208978,9.68503750892865,-25.7221587736968));
#48970=CARTESIAN_POINT('Ctrl Pts',(5.97417293278927,9.68981696133266,-25.7204784027516));
#48971=CARTESIAN_POINT('Ctrl Pts',(5.98852581858903,9.69456763489497,-25.7188097024601));
#48972=CARTESIAN_POINT('Ctrl Pts',(-6.39567215510559,8.78352119285945,-25.5334667703321));
#48973=CARTESIAN_POINT('Ctrl Pts',(-6.35564925586518,8.77012419979114,-25.5378748134888));
#48974=CARTESIAN_POINT('Ctrl Pts',(-5.98524940728022,8.64740171180838,-25.5783537688208));
#48975=CARTESIAN_POINT('Ctrl Pts',(-5.25616631877878,8.42856364545493,-25.6522248402877));
#48976=CARTESIAN_POINT('Ctrl Pts',(-4.17576145259447,8.16491258504182,-25.7436218164382));
#48977=CARTESIAN_POINT('Ctrl Pts',(-3.01936948320032,7.95089104185876,-25.8195372431799));
#48978=CARTESIAN_POINT('Ctrl Pts',(-1.83578686325012,7.80507999288669,-25.8725333135281));
#48979=CARTESIAN_POINT('Ctrl Pts',(-0.697923544185256,7.73463099532804,
-25.8989854355906));
#48980=CARTESIAN_POINT('Ctrl Pts',(0.331409741547889,7.72744130935177,-25.90178757463));
#48981=CARTESIAN_POINT('Ctrl Pts',(1.24580985109183,7.76509280122674,-25.8874719190707));
#48982=CARTESIAN_POINT('Ctrl Pts',(2.07030115244264,7.83520333598814,-25.8615912407003));
#48983=CARTESIAN_POINT('Ctrl Pts',(2.81706942622759,7.92875537879263,-25.8276638258317));
#48984=CARTESIAN_POINT('Ctrl Pts',(3.49018596874702,8.03787927094033,-25.7886683317855));
#48985=CARTESIAN_POINT('Ctrl Pts',(4.09497305491957,8.15592276052121,-25.7470116842076));
#48986=CARTESIAN_POINT('Ctrl Pts',(4.65005393611137,8.2809286723435,-25.7034074146544));
#48987=CARTESIAN_POINT('Ctrl Pts',(5.18050287184726,8.41545116246433,-25.657033997868));
#48988=CARTESIAN_POINT('Ctrl Pts',(5.70542267267832,8.56333394897149,-25.6067231591697));
#48989=CARTESIAN_POINT('Ctrl Pts',(6.10978283777007,8.68890996549213,-25.5646822403335));
#48990=CARTESIAN_POINT('Ctrl Pts',(6.34031611218397,8.76499221874828,-25.5395631156537));
#48991=CARTESIAN_POINT('Ctrl Pts',(6.39541677132646,8.78343680508604,-25.5334956871243));
#48992=CARTESIAN_POINT('Ctrl Pts',(-6.33018795411181,9.06735642773491,-25.77671820803));
#48993=CARTESIAN_POINT('Ctrl Pts',(-6.29063921470765,9.05404079125888,-25.7811588809681));
#48994=CARTESIAN_POINT('Ctrl Pts',(-5.92460030554049,8.932053466397,-25.8219404051921));
#48995=CARTESIAN_POINT('Ctrl Pts',(-5.20363640342463,8.71436008085963,-25.8964088150044));
#48996=CARTESIAN_POINT('Ctrl Pts',(-4.13466319807682,8.45189348050018,-25.9886127972182));
#48997=CARTESIAN_POINT('Ctrl Pts',(-2.99013101605859,8.23872192023846,-26.0652383022213));
#48998=CARTESIAN_POINT('Ctrl Pts',(-1.81835018684379,8.09342931773288,-26.1187427457967));
#48999=CARTESIAN_POINT('Ctrl Pts',(-0.691526419404934,8.02320305496896,
-26.1454435066478));
#49000=CARTESIAN_POINT('Ctrl Pts',(0.328410955095827,8.01603333520191,-26.1482705905495));
#49001=CARTESIAN_POINT('Ctrl Pts',(1.23410624358473,8.0535706645095,-26.1338226905678));
#49002=CARTESIAN_POINT('Ctrl Pts',(2.05052545172647,8.12344568133579,-26.1076952637506));
#49003=CARTESIAN_POINT('Ctrl Pts',(2.78983578864226,8.21666094545048,-26.0734438046011));
#49004=CARTESIAN_POINT('Ctrl Pts',(3.45611831449841,8.3253655430678,-26.0340802931943));
#49005=CARTESIAN_POINT('Ctrl Pts',(4.05467056746315,8.4429263129846,-25.9920389686468));
#49006=CARTESIAN_POINT('Ctrl Pts',(4.60393606387575,8.5673882161268,-25.948043276697));
#49007=CARTESIAN_POINT('Ctrl Pts',(5.1287201730569,8.70128514681539,-25.9012677464719));
#49008=CARTESIAN_POINT('Ctrl Pts',(5.64789136107948,8.84842606812645,-25.8505389176693));
#49009=CARTESIAN_POINT('Ctrl Pts',(6.04766215292126,8.97331108817879,-25.8081672346917));
#49010=CARTESIAN_POINT('Ctrl Pts',(6.27548786339907,9.04894002582314,-25.7828596868889));
#49011=CARTESIAN_POINT('Ctrl Pts',(6.3299352734096,9.06727244757323,-25.7767473024571));
#49012=CARTESIAN_POINT('Ctrl Pts',(-6.21932913978971,9.42526200359147,-25.836655617584));
#49013=CARTESIAN_POINT('Ctrl Pts',(-6.18048424923994,9.41215947646683,-25.8411253051844));
#49014=CARTESIAN_POINT('Ctrl Pts',(-5.82094614614534,9.2921196376942,-25.882174891286));
#49015=CARTESIAN_POINT('Ctrl Pts',(-5.11256398435598,9.07782589043016,-25.9571561089932));
#49016=CARTESIAN_POINT('Ctrl Pts',(-4.06219748980148,8.81943183420526,-26.0500334124317));
#49017=CARTESIAN_POINT('Ctrl Pts',(-2.93773430956758,8.60957997072274,-26.1272375575012));
#49018=CARTESIAN_POINT('Ctrl Pts',(-1.7866100482536,8.46655698550872,-26.1811436018126));
#49019=CARTESIAN_POINT('Ctrl Pts',(-0.679627595369357,8.39741828659515,
-26.208029917519));
#49020=CARTESIAN_POINT('Ctrl Pts',(0.322792418129926,8.39035713706467,-26.2108741294564));
#49021=CARTESIAN_POINT('Ctrl Pts',(1.21265278059722,8.42731721331204,-26.1963301004562));
#49022=CARTESIAN_POINT('Ctrl Pts',(2.01469390800156,8.4961038334689,-26.17001268345));
#49023=CARTESIAN_POINT('Ctrl Pts',(2.74097574438404,8.58786425206803,-26.1355046756559));
#49024=CARTESIAN_POINT('Ctrl Pts',(3.39554807850959,8.69487403657257,-26.0958440499998));
#49025=CARTESIAN_POINT('Ctrl Pts',(3.98362077402804,8.81060581083193,-26.0534876926084));
#49026=CARTESIAN_POINT('Ctrl Pts',(4.52330256827803,8.93313438616758,-26.0091675497922));
#49027=CARTESIAN_POINT('Ctrl Pts',(5.0389473427338,9.06495108380986,-25.9620546712903));
#49028=CARTESIAN_POINT('Ctrl Pts',(5.549066646743,9.20979810657306,-25.9109701561731));
#49029=CARTESIAN_POINT('Ctrl Pts',(5.94181973557236,9.33271765448443,-25.8683114791919));
#49030=CARTESIAN_POINT('Ctrl Pts',(6.16560267800382,9.40714039589557,-25.8428372330143));
#49031=CARTESIAN_POINT('Ctrl Pts',(6.2190806635456,9.42517926284858,-25.8366848568002));
#49032=CARTESIAN_POINT('Ctrl Pts',(-6.0947810190966,9.75500160844674,-25.6963174977319));
#49033=CARTESIAN_POINT('Ctrl Pts',(-6.056668542277,9.7421829968728,-25.7008043046412));
#49034=CARTESIAN_POINT('Ctrl Pts',(-5.70391349769015,9.62474600415793,-25.7420109467264));
#49035=CARTESIAN_POINT('Ctrl Pts',(-5.00898011869918,9.41513447437917,-25.817274113052));
#49036=CARTESIAN_POINT('Ctrl Pts',(-3.97907763476271,9.16253604844767,-25.9104989403831));
#49037=CARTESIAN_POINT('Ctrl Pts',(-2.87715661780143,8.95752386402045,-25.9879852028307));
#49038=CARTESIAN_POINT('Ctrl Pts',(-1.74963938183232,8.81787230129108,-26.0420715124369));
#49039=CARTESIAN_POINT('Ctrl Pts',(-0.665628470734567,8.75037480882317,
-26.0690273778441));
#49040=CARTESIAN_POINT('Ctrl Pts',(0.316160263875782,8.74347976631618,-26.0718760176018));
#49041=CARTESIAN_POINT('Ctrl Pts',(1.18758201208621,8.77956467271151,-26.0572993887014));
#49042=CARTESIAN_POINT('Ctrl Pts',(1.97304891123421,8.8467214319318,-26.0309029323584));
#49043=CARTESIAN_POINT('Ctrl Pts',(2.68445564142065,8.93632518388317,-25.9962790566787));
#49044=CARTESIAN_POINT('Ctrl Pts',(3.32578864567077,9.04084951748645,-25.9564769830062));
#49045=CARTESIAN_POINT('Ctrl Pts',(3.90213225627446,9.15392926544206,-25.9139651165193));
#49046=CARTESIAN_POINT('Ctrl Pts',(4.4312010877471,9.27368825933768,-25.8694800648335));
#49047=CARTESIAN_POINT('Ctrl Pts',(4.93684397707394,9.40256510806607,-25.8221908574905));
#49048=CARTESIAN_POINT('Ctrl Pts',(5.4371949782222,9.54422233392443,-25.7709144512917));
#49049=CARTESIAN_POINT('Ctrl Pts',(5.82250744905633,9.66446408245599,-25.7280944465767));
#49050=CARTESIAN_POINT('Ctrl Pts',(6.04206764945495,9.7372727096129,-25.7025227985368));
#49051=CARTESIAN_POINT('Ctrl Pts',(6.09453704716581,9.75492058441964,-25.6963468075841));
#49052=CARTESIAN_POINT('',(6.27159454904661,8.76071457496506,-25.5608537658249));
#49053=CARTESIAN_POINT('Origin',(5.999999949022,9.3325096643222,-24.7867247244474));
#49054=CARTESIAN_POINT('Ctrl Pts',(-6.27159387327987,8.76070928018864,-25.5608571664728));
#49055=CARTESIAN_POINT('Ctrl Pts',(-6.13239664126094,8.71504798036057,-25.5759656499857));
#49056=CARTESIAN_POINT('Ctrl Pts',(-5.98564490954805,8.66855402099739,-25.5914802279663));
#49057=CARTESIAN_POINT('Ctrl Pts',(-5.8313286216121,8.62173959728843,-25.6072278247019));
#49058=CARTESIAN_POINT('Ctrl Pts',(-5.67907406993691,8.57555063571428,-25.6227650263352));
#49059=CARTESIAN_POINT('Ctrl Pts',(-5.51945544863095,8.52904985474282,-25.6385292465986));
#49060=CARTESIAN_POINT('Ctrl Pts',(-5.35247240281457,8.48276840590744,-25.654323233739));
#49061=CARTESIAN_POINT('Ctrl Pts',(-5.32566690280835,8.47533892484259,-25.6568586152223));
#49062=CARTESIAN_POINT('Ctrl Pts',(-5.29867165164591,8.46791517640557,-25.6593946946507));
#49063=CARTESIAN_POINT('Ctrl Pts',(-5.27148667846808,8.46049945000971,-25.6619305752687));
#49064=CARTESIAN_POINT('Ctrl Pts',(-5.14595415524353,8.42625572131715,-25.6736405552818));
#49065=CARTESIAN_POINT('Ctrl Pts',(-5.01637573562252,8.39218193845674,-25.6853469322197));
#49066=CARTESIAN_POINT('Ctrl Pts',(-4.88275739116987,8.35851824273555,-25.6969639519717));
#49067=CARTESIAN_POINT('Ctrl Pts',(-4.71106407780363,8.31526197068548,-25.711891278162));
#49068=CARTESIAN_POINT('Ctrl Pts',(-4.53269550838595,8.27268031541968,-25.726672510368));
#49069=CARTESIAN_POINT('Ctrl Pts',(-4.34764549623653,8.23131618000222,-25.7411115978377));
#49070=CARTESIAN_POINT('Ctrl Pts',(-4.29584052381524,8.21973624077584,-25.7451538376596));
#49071=CARTESIAN_POINT('Ctrl Pts',(-4.24351201014023,8.20825197500909,-25.7491691109346));
#49072=CARTESIAN_POINT('Ctrl Pts',(-4.1906600681287,8.19687588895432,-25.7531527551433));
#49073=CARTESIAN_POINT('Ctrl Pts',(-4.14338502789855,8.18670019993642,-25.7567160478637));
#49074=CARTESIAN_POINT('Ctrl Pts',(-4.09569119417892,8.176611068498,-25.7602540308525));
#49075=CARTESIAN_POINT('Ctrl Pts',(-4.04757899551552,8.16661761811045,-25.7637634419695));
#49076=CARTESIAN_POINT('Ctrl Pts',(-3.90056247756111,8.13608061670243,-25.7744871548081));
#49077=CARTESIAN_POINT('Ctrl Pts',(-3.74963597646617,8.10643537187603,-25.7849451006779));
#49078=CARTESIAN_POINT('Ctrl Pts',(-3.59479966784943,8.07795017664252,-25.7950405856412));
#49079=CARTESIAN_POINT('Ctrl Pts',(-3.51738151354106,8.06370757902576,-25.8000883281229));
#49080=CARTESIAN_POINT('Ctrl Pts',(-3.43898589874054,8.04975523833549,-25.8050453460868));
#49081=CARTESIAN_POINT('Ctrl Pts',(-3.35961279608689,8.03612821158824,-25.8098988461251));
#49082=CARTESIAN_POINT('Ctrl Pts',(-3.31992624476006,8.02931469821461,-25.8123255961442));
#49083=CARTESIAN_POINT('Ctrl Pts',(-3.27999531907876,8.02258252322768,-25.814726454219));
#49084=CARTESIAN_POINT('Ctrl Pts',(-3.23982001507201,8.0159361753693,-25.8170997778563));
#49085=CARTESIAN_POINT('Ctrl Pts',(-3.21973236306863,8.01261300144011,-25.8182864396749));
#49086=CARTESIAN_POINT('Ctrl Pts',(-3.1995836163341,8.00931128494159,-25.8194662170694));
#49087=CARTESIAN_POINT('Ctrl Pts',(-3.17937377388052,8.00603159219767,-25.8206389007071));
#49088=CARTESIAN_POINT('Ctrl Pts',(-3.16169016173364,8.00316186104674,-25.82166499889));
#49089=CARTESIAN_POINT('Ctrl Pts',(-3.14395977316815,8.00030899187142,-25.8226856658672));
#49090=CARTESIAN_POINT('Ctrl Pts',(-3.12618260742901,7.99747336662541,-25.823700759923));
#49091=CARTESIAN_POINT('Ctrl Pts',(-3.12364301232342,7.99706827730455,-25.8238457733596));
#49092=CARTESIAN_POINT('Ctrl Pts',(-3.11986203701007,7.9964661730716,-25.8240613381855));
#49093=CARTESIAN_POINT('Ctrl Pts',(-3.11856095820616,7.99625915556182,-25.8241354586248));
#49094=CARTESIAN_POINT('Ctrl Pts',(-3.0916130474862,7.99197141422406,-25.8256706392563));
#49095=CARTESIAN_POINT('Ctrl Pts',(-3.06343997656186,7.98754605048026,-25.8272572377435));
#49096=CARTESIAN_POINT('Ctrl Pts',(-3.03404177226685,7.98299895427487,-25.8288895746158));
#49097=CARTESIAN_POINT('Ctrl Pts',(-2.96197570914269,7.97185231011659,-25.8328910466411));
#49098=CARTESIAN_POINT('Ctrl Pts',(-2.88254755643339,7.95997076361514,-25.8371686199672));
#49099=CARTESIAN_POINT('Ctrl Pts',(-2.79575694848145,7.94762209438742,-25.8416264233191));
#49100=CARTESIAN_POINT('Ctrl Pts',(-2.70929659493284,7.93532041414254,-25.8460672639003));
#49101=CARTESIAN_POINT('Ctrl Pts',(-2.61552946386812,7.92255516446984,-25.850687011103));
#49102=CARTESIAN_POINT('Ctrl Pts',(-2.51445628760933,7.90963948626493,-25.8553726467872));
#49103=CARTESIAN_POINT('Ctrl Pts',(-2.50259531789646,7.90812382727726,-25.8559225076404));
#49104=CARTESIAN_POINT('Ctrl Pts',(-2.49063373971749,7.90660615169088,-25.85647325465));
#49105=CARTESIAN_POINT('Ctrl Pts',(-2.47857155780431,7.90508700946898,-25.8570246881376));
#49106=CARTESIAN_POINT('Ctrl Pts',(-2.37688575047032,7.89228043729151,-25.8616733462153));
#49107=CARTESIAN_POINT('Ctrl Pts',(-2.2680499546683,7.87936601812897,-25.8663725574763));
#49108=CARTESIAN_POINT('Ctrl Pts',(-2.15206296372362,7.86670052544834,-25.8709938979129));
#49109=CARTESIAN_POINT('Ctrl Pts',(-2.11969750004126,7.86316629682463,-25.8722834548265));
#49110=CARTESIAN_POINT('Ctrl Pts',(-2.08677525064872,7.85965173629575,-25.8735668334012));
#49111=CARTESIAN_POINT('Ctrl Pts',(-2.05329630949648,7.85616526106339,-25.8748409727839));
#49112=CARTESIAN_POINT('Ctrl Pts',(-1.976568178131,7.84817484319402,-25.8777610870577));
#49113=CARTESIAN_POINT('Ctrl Pts',(-1.89691556848977,7.8403313974129,-25.8806329572634));
#49114=CARTESIAN_POINT('Ctrl Pts',(-1.81433843535376,7.83274216582671,-25.8834176170251));
#49115=CARTESIAN_POINT('Ctrl Pts',(-1.81240162542855,7.83256416377575,-25.8834829299812));
#49116=CARTESIAN_POINT('Ctrl Pts',(-1.81046320669852,7.83238630180687,-25.8835481946928));
#49117=CARTESIAN_POINT('Ctrl Pts',(-1.80852317914455,7.83220858138765,-25.8836134106612));
#49118=CARTESIAN_POINT('Ctrl Pts',(-1.76910604729783,7.82859768978881,-25.8849384570088));
#49119=CARTESIAN_POINT('Ctrl Pts',(-1.7290247580196,7.82504520050363,-25.8862433971052));
#49120=CARTESIAN_POINT('Ctrl Pts',(-1.68827933459894,7.82156332561972,-25.8875239403802));
#49121=CARTESIAN_POINT('Ctrl Pts',(-1.66690392126586,7.81973670293257,-25.8881957248285));
#49122=CARTESIAN_POINT('Ctrl Pts',(-1.64534572750955,7.81792951796679,-25.8888607900245));
#49123=CARTESIAN_POINT('Ctrl Pts',(-1.62360475418917,7.81614356986812,-25.8895184929336));
#49124=CARTESIAN_POINT('Ctrl Pts',(-1.61273426752898,7.81525059581879,-25.8898473443881));
#49125=CARTESIAN_POINT('Ctrl Pts',(-1.60181808594281,7.81436293126474,-25.890174354927));
#49126=CARTESIAN_POINT('Ctrl Pts',(-1.59085620953321,7.81348080406847,-25.8904994431246));
#49127=CARTESIAN_POINT('Ctrl Pts',(-1.58537527132841,7.81303974047034,-25.8906619872234));
#49128=CARTESIAN_POINT('Ctrl Pts',(-1.57988290941558,7.81260006122919,-25.8908240507153));
#49129=CARTESIAN_POINT('Ctrl Pts',(-1.57437912380769,7.81216179501792,-25.8909856233591));
#49130=CARTESIAN_POINT('Ctrl Pts',(-1.56887533819979,7.81172352880665,-25.891147196003));
#49131=CARTESIAN_POINT('Ctrl Pts',(-1.562059610469,7.81118421530923,-25.8913460653726));
#49132=CARTESIAN_POINT('Ctrl Pts',(-1.55783349590704,7.81085126424264,-25.8914688584386));
#49133=CARTESIAN_POINT('Ctrl Pts',(-1.33210040385418,7.79306706254572,-25.8980277100902));
#49134=CARTESIAN_POINT('Ctrl Pts',(-1.11005394165783,7.77943811713524,-25.9030588902186));
#49135=CARTESIAN_POINT('Ctrl Pts',(-0.891697167770649,7.76958904750523,
-25.9066954197387));
#49136=CARTESIAN_POINT('Ctrl Pts',(-0.848420846838444,7.76763705173884,
-25.9074161467204));
#49137=CARTESIAN_POINT('Ctrl Pts',(-0.805289349939968,7.76583365319063,
-25.9080820794156));
#49138=CARTESIAN_POINT('Ctrl Pts',(-0.76230254880461,7.76417611307551,-25.908694233414));
#49139=CARTESIAN_POINT('Ctrl Pts',(-0.72471610697533,7.76272680692871,-25.9092294835382));
#49140=CARTESIAN_POINT('Ctrl Pts',(-0.687240273846953,7.76138898873381,
-25.9097235975349));
#49141=CARTESIAN_POINT('Ctrl Pts',(-0.649875247235843,7.76016076114611,
-25.9101771549314));
#49142=CARTESIAN_POINT('Ctrl Pts',(-0.558064354964064,7.75714284088841,
-25.911291606413));
#49143=CARTESIAN_POINT('Ctrl Pts',(-0.466922504495176,7.7547865017556,-25.9121612187759));
#49144=CARTESIAN_POINT('Ctrl Pts',(-0.37644893037311,7.75306363496773,-25.91279674608));
#49145=CARTESIAN_POINT('Ctrl Pts',(-0.312801759636325,7.75185161700925,
-25.9132438325937));
#49146=CARTESIAN_POINT('Ctrl Pts',(-0.249485476869291,7.75095306674767,
-25.9135750126042));
#49147=CARTESIAN_POINT('Ctrl Pts',(-0.186500082391666,7.7503583420325,-25.9137938241309));
#49148=CARTESIAN_POINT('Ctrl Pts',(-0.155007385152853,7.75006097967492,
-25.9139032298942));
#49149=CARTESIAN_POINT('Ctrl Pts',(-0.123597409863337,7.74983957563556,
-25.9139845411683));
#49150=CARTESIAN_POINT('Ctrl Pts',(-0.0922701561442512,7.74969293819765,
-25.9140381881211));
#49151=CARTESIAN_POINT('Ctrl Pts',(-0.0647193029049692,7.74956397743501,
-25.9140853681049));
#49152=CARTESIAN_POINT('Ctrl Pts',(-0.0383382266194984,7.74949397646208,
-25.9141107435945));
#49153=CARTESIAN_POINT('Ctrl Pts',(-0.0102094372121516,7.74947894116212,
-25.9141157541827));
#49154=CARTESIAN_POINT('Ctrl Pts',(-0.00635381891635554,7.74947688027082,
-25.9141164409849));
#49155=CARTESIAN_POINT('Ctrl Pts',(-0.00246536406951166,7.7494759265866,
-25.9141167169437));
#49156=CARTESIAN_POINT('Ctrl Pts',(0.00146344075487862,7.74947614256322,
-25.9141165581924));
#49157=CARTESIAN_POINT('Ctrl Pts',(0.123997928647954,7.7494828786027,-25.9141116069383));
#49158=CARTESIAN_POINT('Ctrl Pts',(0.246529019799171,7.75063927878568,-25.9136952103562));
#49159=CARTESIAN_POINT('Ctrl Pts',(0.369061817166272,7.75293711554216,-25.9128591305864));
#49160=CARTESIAN_POINT('Ctrl Pts',(0.644876546180536,7.75810942235248,-25.9109771600438));
#49161=CARTESIAN_POINT('Ctrl Pts',(0.920699733188535,7.76906181808629,-25.9069698715593));
#49162=CARTESIAN_POINT('Ctrl Pts',(1.19652079068848,7.78581224103914,-25.9008590747492));
#49163=CARTESIAN_POINT('Ctrl Pts',(1.22211852106872,7.78736677358422,-25.9002919587698));
#49164=CARTESIAN_POINT('Ctrl Pts',(1.24771623489009,7.78897127892905,-25.8997067137304));
#49165=CARTESIAN_POINT('Ctrl Pts',(1.27331392445554,7.79062579306484,-25.8991033499562));
#49166=CARTESIAN_POINT('Ctrl Pts',(1.37082860575515,7.79692868295047,-25.8968048289902));
#49167=CARTESIAN_POINT('Ctrl Pts',(1.4683429363519,7.80395726080187,-25.8942433811165));
#49168=CARTESIAN_POINT('Ctrl Pts',(1.56585686940457,7.81170938476352,-25.8914183109224));
#49169=CARTESIAN_POINT('Ctrl Pts',(1.74018067032872,7.82556770912729,-25.886367986741));
#49170=CARTESIAN_POINT('Ctrl Pts',(1.91450485622957,7.84173917716822,-25.8804762009628));
#49171=CARTESIAN_POINT('Ctrl Pts',(2.08882858930538,7.86022412687243,-25.873742229202));
#49172=CARTESIAN_POINT('Ctrl Pts',(2.17523695511336,7.86938670197223,-25.8704043503889));
#49173=CARTESIAN_POINT('Ctrl Pts',(2.26164519245099,7.87911781127896,-25.8668595119862));
#49174=CARTESIAN_POINT('Ctrl Pts',(2.34805359236325,7.88941699556036,-25.863107937955));
#49175=CARTESIAN_POINT('Ctrl Pts',(2.47841969325897,7.90495558322703,-25.8574478623238));
#49176=CARTESIAN_POINT('Ctrl Pts',(2.60878583328091,7.92178731770248,-25.8513174295213));
#49177=CARTESIAN_POINT('Ctrl Pts',(2.7391519851156,7.93991205128417,-25.844716566341));
#49178=CARTESIAN_POINT('Ctrl Pts',(2.77254675013872,7.94455490689162,-25.8430256805416));
#49179=CARTESIAN_POINT('Ctrl Pts',(2.80594152186298,7.94928260741816,-25.8413039117632));
#49180=CARTESIAN_POINT('Ctrl Pts',(2.83933628185507,7.95409517550948,-25.8395512547973));
#49181=CARTESIAN_POINT('Ctrl Pts',(2.87112458796028,7.95867623516301,-25.8378829093401));
#49182=CARTESIAN_POINT('Ctrl Pts',(2.90291288340858,7.96333419376135,-25.8361865759424));
#49183=CARTESIAN_POINT('Ctrl Pts',(2.93470118421066,7.96806902181925,-25.8344622611208));
#49184=CARTESIAN_POINT('Ctrl Pts',(2.98358847562793,7.97535072336469,-25.831810433906));
#49185=CARTESIAN_POINT('Ctrl Pts',(3.03247576357619,7.98281424499757,-25.8290924418474));
#49186=CARTESIAN_POINT('Ctrl Pts',(3.08136305395075,7.99045953986186,-25.8263083278156));
#49187=CARTESIAN_POINT('Ctrl Pts',(3.09765881740894,7.99300797148329,-25.825380289805));
#49188=CARTESIAN_POINT('Ctrl Pts',(3.11203760759698,7.99527206051231,-25.8245558041096));
#49189=CARTESIAN_POINT('Ctrl Pts',(3.13025034515279,7.99816542513299,-25.8235021733253));
#49190=CARTESIAN_POINT('Ctrl Pts',(3.2587731856329,8.01858319255843,-25.816066958229));
#49191=CARTESIAN_POINT('Ctrl Pts',(3.3858763678512,8.04008539286075,-25.8082999187491));
#49192=CARTESIAN_POINT('Ctrl Pts',(3.51154612819138,8.06258692776756,-25.8002309208586));
#49193=CARTESIAN_POINT('Ctrl Pts',(3.71380564174188,8.09880208002115,-25.7872442518004));
#49194=CARTESIAN_POINT('Ctrl Pts',(3.91235133347899,8.13760487958652,-25.7734759965143));
#49195=CARTESIAN_POINT('Ctrl Pts',(4.10714944139394,8.17864887428146,-25.7590478093978));
#49196=CARTESIAN_POINT('Ctrl Pts',(4.29250029058855,8.21770232994627,-25.7453193560622));
#49197=CARTESIAN_POINT('Ctrl Pts',(4.47445852097808,8.25878502137493,-25.7309933926776));
#49198=CARTESIAN_POINT('Ctrl Pts',(4.65301431239839,8.30161272215025,-25.7161706651186));
#49199=CARTESIAN_POINT('Ctrl Pts',(4.83065430932707,8.3442207640047,-25.7014239618215));
#49200=CARTESIAN_POINT('Ctrl Pts',(5.00492682819878,8.38855605849592,-25.6861856286938));
#49201=CARTESIAN_POINT('Ctrl Pts',(5.1758378275253,8.43435590184726,-25.670551811168));
#49202=CARTESIAN_POINT('Ctrl Pts',(5.35320999678042,8.48188717601207,-25.6543269681841));
#49203=CARTESIAN_POINT('Ctrl Pts',(5.52696176321428,8.53099591182413,-25.637676341178));
#49204=CARTESIAN_POINT('Ctrl Pts',(5.69711466993971,8.58141145046569,-25.62070496883));
#49205=CARTESIAN_POINT('Ctrl Pts',(5.87744654478025,8.63484297143877,-25.6027183269734));
#49206=CARTESIAN_POINT('Ctrl Pts',(6.05373611659351,8.68974251290063,-25.5843717510258));
#49207=CARTESIAN_POINT('Ctrl Pts',(6.226022223609,8.74581972929454,-25.5657891374643));
#49208=CARTESIAN_POINT('Ctrl Pts',(6.24124473246824,8.75077448704109,-25.5641472523206));
#49209=CARTESIAN_POINT('Ctrl Pts',(6.2564359933192,8.75573844668456,-25.5625035131198));
#49210=CARTESIAN_POINT('Ctrl Pts',(6.27159604047972,8.76071143370063,-25.5608580130011));
#49211=CARTESIAN_POINT('Origin',(5.999999999061,9.33250979146072,-24.7867247845918));
#49212=CARTESIAN_POINT('Origin',(5.99996968669111,9.33251391750253,-24.7866936478717));
#49213=CARTESIAN_POINT('Ctrl Pts',(6.25392027494701,3.90298732745545,-15.8231684029013));
#49214=CARTESIAN_POINT('Ctrl Pts',(6.30498637037455,3.91655122781545,-15.8051570120035));
#49215=CARTESIAN_POINT('Ctrl Pts',(6.44770248625324,3.96600398299862,-15.7512014975234));
#49216=CARTESIAN_POINT('Ctrl Pts',(6.66633061405961,4.09807443964668,-15.6507405657398));
#49217=CARTESIAN_POINT('Ctrl Pts',(6.88010573794568,4.32343154619026,-15.5214493319802));
#49218=CARTESIAN_POINT('Ctrl Pts',(7.03309503798963,4.607315341482,-15.3885588610201));
#49219=CARTESIAN_POINT('Ctrl Pts',(7.09634443075797,4.87218675594795,-15.2845094186338));
#49220=CARTESIAN_POINT('Ctrl Pts',(7.10389711961593,5.03409215205006,-15.228651260299));
#49221=CARTESIAN_POINT('Ctrl Pts',(7.10327724980352,5.08536189847456,-15.2117263055378));
#49222=CARTESIAN_POINT('Ctrl Pts',(6.05652411355051,3.85906155699697,-15.2125089076995));
#49223=CARTESIAN_POINT('Ctrl Pts',(6.10187709936855,3.87077510290403,-15.1964773801162));
#49224=CARTESIAN_POINT('Ctrl Pts',(6.22889159885922,3.91360449797959,-15.1483525761357));
#49225=CARTESIAN_POINT('Ctrl Pts',(6.42453376431358,4.02884063488479,-15.0583089083087));
#49226=CARTESIAN_POINT('Ctrl Pts',(6.61687258416338,4.22699772610696,-14.9420678245189));
#49227=CARTESIAN_POINT('Ctrl Pts',(6.75502557493823,4.47794845855267,-14.8226484218656));
#49228=CARTESIAN_POINT('Ctrl Pts',(6.8121853548424,4.71267003637461,-14.7296123730615));
#49229=CARTESIAN_POINT('Ctrl Pts',(6.81897933253834,4.85592976215469,-14.6800904100871));
#49230=CARTESIAN_POINT('Ctrl Pts',(6.81842108595897,4.90123798330861,-14.6651416079335));
#49231=CARTESIAN_POINT('Ctrl Pts',(6.04728643245338,3.3642601016969,-14.8018988955162));
#49232=CARTESIAN_POINT('Ctrl Pts',(6.1096864082144,3.38027488763903,-14.780301688516));
#49233=CARTESIAN_POINT('Ctrl Pts',(6.28323634553052,3.43850801268331,-14.7160886442661));
#49234=CARTESIAN_POINT('Ctrl Pts',(6.54570992416607,3.59232396077953,-14.5987447339918));
#49235=CARTESIAN_POINT('Ctrl Pts',(6.79905716620728,3.8511821076201,-14.4503513769499));
#49236=CARTESIAN_POINT('Ctrl Pts',(6.97876410714886,4.17408834693898,-14.2994899754014));
#49237=CARTESIAN_POINT('Ctrl Pts',(7.05291929263889,4.47422356328171,-14.1817471419756));
#49238=CARTESIAN_POINT('Ctrl Pts',(7.06187440122695,4.65851681165845,-14.1181749926599));
#49239=CARTESIAN_POINT('Ctrl Pts',(7.06114148281948,4.71705880021148,-14.098847828217));
#49240=CARTESIAN_POINT('Ctrl Pts',(6.23212119064543,2.7520459899376,-14.8671517492495));
#49241=CARTESIAN_POINT('Ctrl Pts',(6.32282827124314,2.77561132425719,-14.8361981369132));
#49242=CARTESIAN_POINT('Ctrl Pts',(6.5737574938549,2.86088152010372,-14.744831804744));
#49243=CARTESIAN_POINT('Ctrl Pts',(6.94779412332067,3.08265908688098,-14.5808890356009));
#49244=CARTESIAN_POINT('Ctrl Pts',(7.30343635770547,3.44915925509986,-14.3768346722789));
#49245=CARTESIAN_POINT('Ctrl Pts',(7.55305356317214,3.90035404771087,-14.1708337848037));
#49246=CARTESIAN_POINT('Ctrl Pts',(7.65582336285289,4.31732496808673,-14.0093356417527));
#49247=CARTESIAN_POINT('Ctrl Pts',(7.66840148009804,4.57464175472762,-13.920807830227));
#49248=CARTESIAN_POINT('Ctrl Pts',(7.66737543417775,4.65668281802034,-13.8937022602362));
#49249=CARTESIAN_POINT('',(6.99999200753597,4.92968844883675,-14.7967977305573));
#49250=CARTESIAN_POINT('',(7.00000029677448,3.16613090165484,-14.5427412926877));
#49251=CARTESIAN_POINT('Ctrl Pts',(7.,4.92968844926947,-14.7967977304731));
#49252=CARTESIAN_POINT('Ctrl Pts',(7.,4.82769576894919,-14.7564330540733));
#49253=CARTESIAN_POINT('Ctrl Pts',(7.,4.7350293213622,-14.7220626972232));
#49254=CARTESIAN_POINT('Ctrl Pts',(7.,4.65323746896003,-14.6940819631314));
#49255=CARTESIAN_POINT('Ctrl Pts',(7.,4.61234154275894,-14.6800915960855));
#49256=CARTESIAN_POINT('Ctrl Pts',(7.,4.57417008110355,-14.6676560278867));
#49257=CARTESIAN_POINT('Ctrl Pts',(7.,4.53894527480209,-14.6566252007483));
#49258=CARTESIAN_POINT('Ctrl Pts',(7.,4.52133287165136,-14.6511097871791));
#49259=CARTESIAN_POINT('Ctrl Pts',(7.,4.50445726238892,-14.6459439846359));
#49260=CARTESIAN_POINT('Ctrl Pts',(7.,4.4883456810344,-14.6411019035005));
#49261=CARTESIAN_POINT('Ctrl Pts',(7.,4.48028989035715,-14.6386808629328));
#49262=CARTESIAN_POINT('Ctrl Pts',(7.,4.47242510665687,-14.6363407527171));
#49263=CARTESIAN_POINT('Ctrl Pts',(7.,4.46475458846243,-14.6340780114449));
#49264=CARTESIAN_POINT('Ctrl Pts',(7.,4.46091932936521,-14.6329466408089));
#49265=CARTESIAN_POINT('Ctrl Pts',(7.,4.45713263664445,-14.6318346124087));
#49266=CARTESIAN_POINT('Ctrl Pts',(7.,4.45339490911939,-14.6307414807438));
#49267=CARTESIAN_POINT('Ctrl Pts',(7.,4.44965718159433,-14.6296483490789));
#49268=CARTESIAN_POINT('Ctrl Pts',(7.,4.44750552652622,-14.6290200289085));
#49269=CARTESIAN_POINT('Ctrl Pts',(7.,4.44232901759576,-14.6275183273043));
#49270=CARTESIAN_POINT('Ctrl Pts',(7.,4.35950487470844,-14.6034911016374));
#49271=CARTESIAN_POINT('Ctrl Pts',(7.,4.27923941186931,-14.5829868342322));
#49272=CARTESIAN_POINT('Ctrl Pts',(7.,4.20215931213699,-14.5660822358387));
#49273=CARTESIAN_POINT('Ctrl Pts',(7.,4.12507921240467,-14.5491776374452));
#49274=CARTESIAN_POINT('Ctrl Pts',(7.,4.05278013298332,-14.5360945759712));
#49275=CARTESIAN_POINT('Ctrl Pts',(7.,3.98127020879684,-14.5256226924827));
#49276=CARTESIAN_POINT('Ctrl Pts',(7.,3.83825036042388,-14.5046789255058));
#49277=CARTESIAN_POINT('Ctrl Pts',(7.,3.69577797679041,-14.4945086567194));
#49278=CARTESIAN_POINT('Ctrl Pts',(7.,3.55815928031856,-14.4973986345922));
#49279=CARTESIAN_POINT('Ctrl Pts',(7.,3.42054058384671,-14.5002886124651));
#49280=CARTESIAN_POINT('Ctrl Pts',(7.,3.28800110200234,-14.5162068700801));
#49281=CARTESIAN_POINT('Ctrl Pts',(7.,3.16613170174698,-14.5427408959923));
#49282=CARTESIAN_POINT('',(6.24994411785848,2.76546207136057,-14.8593862266086));
#49283=CARTESIAN_POINT('Ctrl Pts',(6.24994455730984,2.7654623494508,-14.8593877207787));
#49284=CARTESIAN_POINT('Ctrl Pts',(6.29979781833251,2.77899594289883,-14.8422062667216));
#49285=CARTESIAN_POINT('Ctrl Pts',(6.34863096323173,2.7944176673382,-14.8247566362977));
#49286=CARTESIAN_POINT('Ctrl Pts',(6.39646857396924,2.81164057419167,-14.8070481760307));
#49287=CARTESIAN_POINT('Ctrl Pts',(6.42911332404107,2.82339361706054,-14.7949637878126));
#49288=CARTESIAN_POINT('Ctrl Pts',(6.46129434933223,2.83598654928082,-14.7827585948818));
#49289=CARTESIAN_POINT('Ctrl Pts',(6.49301580980901,2.84940483943542,-14.7704328360015));
#49290=CARTESIAN_POINT('Ctrl Pts',(6.54021855514441,2.8693717679275,-14.7520916357937));
#49291=CARTESIAN_POINT('Ctrl Pts',(6.58640506262817,2.89116430239203,-14.7334837053198));
#49292=CARTESIAN_POINT('Ctrl Pts',(6.63160836973239,2.91475048338072,-14.7145978869442));
#49293=CARTESIAN_POINT('Ctrl Pts',(6.63723860889029,2.91768822949478,-14.7122455883856));
#49294=CARTESIAN_POINT('Ctrl Pts',(6.64285356156666,2.92065385816639,-14.7098889707024));
#49295=CARTESIAN_POINT('Ctrl Pts',(6.64845326188242,2.92364735500386,-14.7075280059086));
#49296=CARTESIAN_POINT('Ctrl Pts',(6.69418400793763,2.94809417107832,-14.6882468523933));
#49297=CARTESIAN_POINT('Ctrl Pts',(6.73887860241311,2.9743951866194,-14.6686831423798));
#49298=CARTESIAN_POINT('Ctrl Pts',(6.7825302865664,3.00255784800113,-14.648823534793));
#49299=CARTESIAN_POINT('Ctrl Pts',(6.82571493102099,3.03041919040419,-14.6291764098476));
#49300=CARTESIAN_POINT('Ctrl Pts',(6.86787933734953,3.06010299316823,-14.609239479601));
#49301=CARTESIAN_POINT('Ctrl Pts',(6.90897979149492,3.09165114058264,-14.5889981419846));
#49302=CARTESIAN_POINT('Ctrl Pts',(6.91447876829732,3.09587208009287,-14.5862899810089));
#49303=CARTESIAN_POINT('Ctrl Pts',(6.91995863828218,3.10012643844517,-14.5835763710984));
#49304=CARTESIAN_POINT('Ctrl Pts',(6.92541923818674,3.10441435723096,-14.5808572780706));
#49305=CARTESIAN_POINT('Ctrl Pts',(6.95069604285227,3.12426288806353,-14.5682707519501));
#49306=CARTESIAN_POINT('Ctrl Pts',(6.97556046737544,3.14483022611502,-14.5555667144424));
#49307=CARTESIAN_POINT('Ctrl Pts',(7.00000088934497,3.16612989450563,-14.5427407493156));
#49308=CARTESIAN_POINT('',(6.26385789024229,3.90573692077446,-15.8144409741972));
#49309=CARTESIAN_POINT('Origin',(6.52774091094718,2.94125499125657,-15.8038022189583));
#49310=CARTESIAN_POINT('Ctrl Pts',(6.26385527955666,3.90574646326258,-15.8144410794374));
#49311=CARTESIAN_POINT('Ctrl Pts',(6.30677501622484,3.91779325316633,-15.7868226401676));
#49312=CARTESIAN_POINT('Ctrl Pts',(6.34923257297403,3.93289027417838,-15.75778635456));
#49313=CARTESIAN_POINT('Ctrl Pts',(6.3907785074684,3.95108686753143,-15.7274032517978));
#49314=CARTESIAN_POINT('Ctrl Pts',(6.43558717779547,3.97071249787424,-15.6946340662746));
#49315=CARTESIAN_POINT('Ctrl Pts',(6.47933557617439,3.99394464936472,-15.6602976444418));
#49316=CARTESIAN_POINT('Ctrl Pts',(6.52150122927541,4.02069411945903,-15.6245203039367));
#49317=CARTESIAN_POINT('Ctrl Pts',(6.53207018575043,4.02739896011403,-15.6155525985466));
#49318=CARTESIAN_POINT('Ctrl Pts',(6.54253947197269,4.03432477240376,-15.60649446611));
#49319=CARTESIAN_POINT('Ctrl Pts',(6.5529003759936,4.04147015600223,-15.5973481025264));
#49320=CARTESIAN_POINT('Ctrl Pts',(6.57464090466716,4.05646348252013,-15.5781560726277));
#49321=CARTESIAN_POINT('Ctrl Pts',(6.59590457157523,4.07242355443942,-15.5585754483081));
#49322=CARTESIAN_POINT('Ctrl Pts',(6.61660777073193,4.08933791168146,-15.5386277503673));
#49323=CARTESIAN_POINT('Ctrl Pts',(6.63876804721789,4.10744269008932,-15.5172761467683));
#49324=CARTESIAN_POINT('Ctrl Pts',(6.66028617076777,4.12664091652856,-15.4955039354844));
#49325=CARTESIAN_POINT('Ctrl Pts',(6.68107533790851,4.14689256153848,-15.4733417200545));
#49326=CARTESIAN_POINT('Ctrl Pts',(6.70118104281552,4.16647841582952,-15.4519081070337));
#49327=CARTESIAN_POINT('Ctrl Pts',(6.72060496323911,4.18704952161287,-15.4301097156608));
#49328=CARTESIAN_POINT('Ctrl Pts',(6.73926365585971,4.20856966843344,-15.4079765811578));
#49329=CARTESIAN_POINT('Ctrl Pts',(6.74859300217001,4.21932974184372,-15.3969100139063));
#49330=CARTESIAN_POINT('Ctrl Pts',(6.75773099346059,4.23032711811503,-15.3857597628736));
#49331=CARTESIAN_POINT('Ctrl Pts',(6.76666663238851,4.24155727259564,-15.3745298510729));
#49332=CARTESIAN_POINT('Ctrl Pts',(6.77113445185248,4.24717234983594,-15.3689148951726));
#49333=CARTESIAN_POINT('Ctrl Pts',(6.77555167975256,4.25284562488489,-15.3632800242269));
#49334=CARTESIAN_POINT('Ctrl Pts',(6.77991691030056,4.25857654281244,-15.3576257506515));
#49335=CARTESIAN_POINT('Ctrl Pts',(6.7826528047095,4.26216837745751,-15.3540819526112));
#49336=CARTESIAN_POINT('Ctrl Pts',(6.78569591686906,4.26622078384239,-15.3501001756321));
#49337=CARTESIAN_POINT('Ctrl Pts',(6.78842750025002,4.26991217685713,-15.3464895428362));
#49338=CARTESIAN_POINT('Ctrl Pts',(6.79005426899699,4.27211055118867,-15.3443392644922));
#49339=CARTESIAN_POINT('Ctrl Pts',(6.79157148607674,4.27418008599266,-15.3423206972513));
#49340=CARTESIAN_POINT('Ctrl Pts',(6.79285518238893,4.27594167920464,-15.3406052397862));
#49341=CARTESIAN_POINT('Ctrl Pts',(6.79521152840393,4.27917525018686,-15.3374563553317));
#49342=CARTESIAN_POINT('Ctrl Pts',(6.79756024076484,4.28243827572785,-15.3342895371218));
#49343=CARTESIAN_POINT('Ctrl Pts',(6.79990066491025,4.28573099267086,-15.3311048460252));
#49344=CARTESIAN_POINT('Ctrl Pts',(6.81783379914537,4.31096092163608,-15.3067026482244));
#49345=CARTESIAN_POINT('Ctrl Pts',(6.83528346595841,4.33793603225933,-15.2812494305542));
#49346=CARTESIAN_POINT('Ctrl Pts',(6.85196339539571,4.3667222959665,-15.2547860263646));
#49347=CARTESIAN_POINT('Ctrl Pts',(6.86776035936218,4.39398473566812,-15.2297234837451));
#49348=CARTESIAN_POINT('Ctrl Pts',(6.88286710000684,4.42287156068814,-15.2037548229464));
#49349=CARTESIAN_POINT('Ctrl Pts',(6.89700434437673,4.45341835639927,-15.176933537494));
#49350=CARTESIAN_POINT('Ctrl Pts',(6.90834830381464,4.47792961208946,-15.1554116930466));
#49351=CARTESIAN_POINT('Ctrl Pts',(6.91906750511668,4.50350931159876,-15.13334116626));
#49352=CARTESIAN_POINT('Ctrl Pts',(6.92899766648264,4.53016601726516,-15.1107595934415));
#49353=CARTESIAN_POINT('Ctrl Pts',(6.93174472990178,4.53754028423948,-15.1045126644793));
#49354=CARTESIAN_POINT('Ctrl Pts',(6.93443128870946,4.5449969226956,-15.0982266823882));
#49355=CARTESIAN_POINT('Ctrl Pts',(6.93705415527578,4.55253553000811,-15.0919026372694));
#49356=CARTESIAN_POINT('Ctrl Pts',(6.94825805191974,4.58473761693595,-15.0648887019085));
#49357=CARTESIAN_POINT('Ctrl Pts',(6.95830252975268,4.61843781676003,-15.0371784024747));
#49358=CARTESIAN_POINT('Ctrl Pts',(6.96691898512431,4.6535869298058,-15.0088629431602));
#49359=CARTESIAN_POINT('Ctrl Pts',(6.97510443426528,4.68697783880229,-14.9819638597059));
#49360=CARTESIAN_POINT('Ctrl Pts',(6.9820014634844,4.72167619755401,-14.9545186209884));
#49361=CARTESIAN_POINT('Ctrl Pts',(6.98734637694117,4.75761495687658,-14.9266266850321));
#49362=CARTESIAN_POINT('Ctrl Pts',(6.98981427690794,4.77420891366478,-14.9137481775732));
#49363=CARTESIAN_POINT('Ctrl Pts',(6.99195076731028,4.79106696982164,-14.9007747454111));
#49364=CARTESIAN_POINT('Ctrl Pts',(6.99372697726635,4.80818070467899,-14.8877178592447));
#49365=CARTESIAN_POINT('Ctrl Pts',(6.99740919774112,4.84365879930168,-14.8606499254039));
#49366=CARTESIAN_POINT('Ctrl Pts',(6.99954480901166,4.8802379977655,-14.8332216625081));
#49367=CARTESIAN_POINT('Ctrl Pts',(6.99991734819238,4.91777656577306,-14.8055596995045));
#49368=CARTESIAN_POINT('Ctrl Pts',(6.99995664834309,4.92173660932317,-14.8026415653297));
#49369=CARTESIAN_POINT('Ctrl Pts',(6.99997629845513,4.92570729933136,-14.799720853908));
#49370=CARTESIAN_POINT('Ctrl Pts',(6.99997602260847,4.92968844797978,-14.7967977308986));
#49371=CARTESIAN_POINT('Ctrl Pts',(6.99990207659395,4.95612342846035,-14.684705142693));
#49372=CARTESIAN_POINT('Ctrl Pts',(6.99990207659395,4.91843322561129,-15.0109955237193));
#49373=CARTESIAN_POINT('Ctrl Pts',(6.99990207659395,4.8561621330926,-15.8988757775478));
#49374=CARTESIAN_POINT('Ctrl Pts',(6.99990207659395,4.93000355594309,-17.3517252626563));
#49375=CARTESIAN_POINT('Ctrl Pts',(6.99990207659395,5.27370128699297,-19.0057031767965));
#49376=CARTESIAN_POINT('Ctrl Pts',(6.99990207659395,5.86661420603441,-20.5902607600442));
#49377=CARTESIAN_POINT('Ctrl Pts',(6.99990207659395,6.69609459969272,-22.0651325913196));
#49378=CARTESIAN_POINT('Ctrl Pts',(6.99990207659395,7.73957894060174,-23.3944692108351));
#49379=CARTESIAN_POINT('Ctrl Pts',(6.99990207659395,8.69530687990185,-24.2870452318747));
#49380=CARTESIAN_POINT('Ctrl Pts',(6.99990207659395,9.28612124925631,-24.7366401017851));
#49381=CARTESIAN_POINT('Ctrl Pts',(6.99990207659395,9.4330871100264,-24.8428478912403));
#49382=CARTESIAN_POINT('Ctrl Pts',(7.00660364663921,4.48044941032924,-14.629744314853));
#49383=CARTESIAN_POINT('Ctrl Pts',(7.00660364663921,4.44110729653057,-14.970322314067));
#49384=CARTESIAN_POINT('Ctrl Pts',(7.00660364663921,4.37614027536931,-15.8968427125844));
#49385=CARTESIAN_POINT('Ctrl Pts',(7.00660364663921,4.45318215224793,-17.4128418304199));
#49386=CARTESIAN_POINT('Ctrl Pts',(7.00660364663921,4.81191599524873,-19.1393493860805));
#49387=CARTESIAN_POINT('Ctrl Pts',(7.00660364663921,5.4307158401717,-20.792933289964));
#49388=CARTESIAN_POINT('Ctrl Pts',(7.00660364663921,6.29626827380092,-22.332051081099));
#49389=CARTESIAN_POINT('Ctrl Pts',(7.00660364663921,7.38553208571995,-23.7196527338312));
#49390=CARTESIAN_POINT('Ctrl Pts',(7.00660364663921,8.38275194446837,-24.650964724442));
#49391=CARTESIAN_POINT('Ctrl Pts',(7.00660364663921,8.99924836318557,-25.1201131729878));
#49392=CARTESIAN_POINT('Ctrl Pts',(7.00660364663921,9.1526167444896,-25.2309488097062));
#49393=CARTESIAN_POINT('Ctrl Pts',(6.71667356571233,4.1017052012643,-14.5859830529861));
#49394=CARTESIAN_POINT('Ctrl Pts',(6.71667356571233,4.06104779236811,-14.9379372309449));
#49395=CARTESIAN_POINT('Ctrl Pts',(6.71667356571233,3.99393420165435,-15.8952239325906));
#49396=CARTESIAN_POINT('Ctrl Pts',(6.71667356571233,4.07352436451027,-17.4615044548973));
#49397=CARTESIAN_POINT('Ctrl Pts',(6.71667356571233,4.44423035673658,-19.2457620256132));
#49398=CARTESIAN_POINT('Ctrl Pts',(6.71667356571233,5.08364205535591,-20.9543065080017));
#49399=CARTESIAN_POINT('Ctrl Pts',(6.71667356571233,5.97791599936316,-22.5445786282065));
#49400=CARTESIAN_POINT('Ctrl Pts',(6.71667356571233,7.10363063448991,-23.9785724383432));
#49401=CARTESIAN_POINT('Ctrl Pts',(6.71667356571233,8.13388745471671,-24.940727030391));
#49402=CARTESIAN_POINT('Ctrl Pts',(6.71667356571233,8.77083259903691,-25.4254445543805));
#49403=CARTESIAN_POINT('Ctrl Pts',(6.71667356571233,8.92929883618842,-25.5399650052432));
#49404=CARTESIAN_POINT('Ctrl Pts',(6.25321309030958,3.98119853671877,-14.5720593451688));
#49405=CARTESIAN_POINT('Ctrl Pts',(6.25321309030958,3.94012263475573,-14.9276331305612));
#49406=CARTESIAN_POINT('Ctrl Pts',(6.25321309030958,3.87232606083332,-15.8947088784425));
#49407=CARTESIAN_POINT('Ctrl Pts',(6.25321309030958,3.95272702273434,-17.4769876502149));
#49408=CARTESIAN_POINT('Ctrl Pts',(6.25321309030958,4.32724224487352,-19.2796197901663));
#49409=CARTESIAN_POINT('Ctrl Pts',(6.25321309030958,4.97321210511988,-21.0056513148311));
#49410=CARTESIAN_POINT('Ctrl Pts',(6.25321309030958,5.87662449490167,-22.6121994266604));
#49411=CARTESIAN_POINT('Ctrl Pts',(6.25321309030958,7.01393684431548,-24.0609540278942));
#49412=CARTESIAN_POINT('Ctrl Pts',(6.25321309030958,8.05470517584552,-25.0329219423298));
#49413=CARTESIAN_POINT('Ctrl Pts',(6.25321309030958,8.69815657863172,-25.5225931456291));
#49414=CARTESIAN_POINT('Ctrl Pts',(6.25321309030958,8.85824482237706,-25.6382860095647));
#49415=CARTESIAN_POINT('Ctrl Pts',(6.99999999999946,4.92968844925125,-14.7967977306008));
#49416=CARTESIAN_POINT('Ctrl Pts',(6.99999999999946,4.91233123517191,-14.9621835172955));
#49417=CARTESIAN_POINT('Ctrl Pts',(6.99999999997464,4.89876479509306,-15.1274620360007));
#49418=CARTESIAN_POINT('Ctrl Pts',(6.9999999993832,4.88893183450758,-15.2927163168167));
#49419=CARTESIAN_POINT('Ctrl Pts',(6.99999999893632,4.88150212010356,-15.4175812646452));
#49420=CARTESIAN_POINT('Ctrl Pts',(6.99999999820117,4.87620500438501,-15.5424326368658));
#49421=CARTESIAN_POINT('Ctrl Pts',(6.99999999795816,4.87303542048088,-15.6673078032506));
#49422=CARTESIAN_POINT('Ctrl Pts',(6.99999999763562,4.8688284502018,-15.8330538852174));
#49423=CARTESIAN_POINT('Ctrl Pts',(6.99999999919455,4.86836771463358,-15.9988422474281));
#49424=CARTESIAN_POINT('Ctrl Pts',(6.99999999987624,4.87168823513293,-16.1647921805699));
#49425=CARTESIAN_POINT('Ctrl Pts',(6.99999999995189,4.87205668724803,-16.183206343012));
#49426=CARTESIAN_POINT('Ctrl Pts',(6.99999999999964,4.87247174903354,-16.2016224895237));
#49427=CARTESIAN_POINT('Ctrl Pts',(6.99999999999964,4.87293350770597,-16.2200407785058));
#49428=CARTESIAN_POINT('Ctrl Pts',(6.99999999999964,4.87803551097676,-16.4235457178609));
#49429=CARTESIAN_POINT('Ctrl Pts',(6.99999999555513,4.88875796900593,-16.6272930258414));
#49430=CARTESIAN_POINT('Ctrl Pts',(6.99999999493485,4.90514631566278,-16.8307386153249));
#49431=CARTESIAN_POINT('Ctrl Pts',(6.99999999440965,4.91902260107297,-17.0029993762319));
#49432=CARTESIAN_POINT('Ctrl Pts',(6.99999999611632,4.93696006359404,-17.1750435554702));
#49433=CARTESIAN_POINT('Ctrl Pts',(6.99999999794794,4.95895705184918,-17.3465408121815));
#49434=CARTESIAN_POINT('Ctrl Pts',(6.99999999900192,4.97161496384682,-17.4452269213029));
#49435=CARTESIAN_POINT('Ctrl Pts',(6.99999999999964,4.98561660497,-17.5437319472142));
#49436=CARTESIAN_POINT('Ctrl Pts',(6.99999999999964,5.00094770326887,-17.6419939642891));
#49437=CARTESIAN_POINT('Ctrl Pts',(6.99999999999964,5.04134916509787,-17.9009401307474));
#49438=CARTESIAN_POINT('Ctrl Pts',(6.99999999748067,5.09107364972735,-18.1581948885142));
#49439=CARTESIAN_POINT('Ctrl Pts',(6.9999999983993,5.14990920187463,-18.4132918257843));
#49440=CARTESIAN_POINT('Ctrl Pts',(6.99999999910474,5.19509078503942,-18.6091884064351));
#49441=CARTESIAN_POINT('Ctrl Pts',(6.99999999994352,5.24564636503982,-18.803812805501));
#49442=CARTESIAN_POINT('Ctrl Pts',(6.99999999999482,5.30150075775557,-18.9969552607985));
#49443=CARTESIAN_POINT('Ctrl Pts',(6.99999999999814,5.30512332812396,-19.0094819771662));
#49444=CARTESIAN_POINT('Ctrl Pts',(6.99999999999964,5.30876819415222,-19.0220024596165));
#49445=CARTESIAN_POINT('Ctrl Pts',(6.99999999999964,5.3124353329409,-19.0345166513395));
#49446=CARTESIAN_POINT('Ctrl Pts',(6.99999999999964,5.41320704222893,-19.3784023243266));
#49447=CARTESIAN_POINT('Ctrl Pts',(7.0000000000075,5.53077138717327,-19.7175348267532));
#49448=CARTESIAN_POINT('Ctrl Pts',(6.99999999997804,5.66466508951816,-20.0501490251692));
#49449=CARTESIAN_POINT('Ctrl Pts',(6.99999999996837,5.7085987338504,-20.1592874957406));
#49450=CARTESIAN_POINT('Ctrl Pts',(6.99999999999964,5.7542901016912,-20.2677239882539));
#49451=CARTESIAN_POINT('Ctrl Pts',(6.99999999999964,5.80172169984713,-20.3753956739967));
#49452=CARTESIAN_POINT('Ctrl Pts',(6.99999999999964,5.83157383362071,-20.4431612499289));
#49453=CARTESIAN_POINT('Ctrl Pts',(6.99999999997177,5.86211302945351,-20.5106252086442));
#49454=CARTESIAN_POINT('Ctrl Pts',(6.99999999993234,5.89333412587516,-20.577772371119));
#49455=CARTESIAN_POINT('Ctrl Pts',(6.99999999971818,6.06290292235333,-20.9424637123202));
#49456=CARTESIAN_POINT('Ctrl Pts',(6.99999999999964,6.25259012480563,-21.2978070675131));
#49457=CARTESIAN_POINT('Ctrl Pts',(6.99999999999964,6.46101007423756,-21.6416318480036));
#49458=CARTESIAN_POINT('Ctrl Pts',(6.99999999999964,6.5445514342191,-21.7794477808633));
#49459=CARTESIAN_POINT('Ctrl Pts',(6.99999999962317,6.63110403210437,-21.9154125925419));
#49460=CARTESIAN_POINT('Ctrl Pts',(6.99999999912704,6.72060693187971,-22.0494138888238));
#49461=CARTESIAN_POINT('Ctrl Pts',(6.99999999825471,6.87797393131849,-22.2850194610423));
#49462=CARTESIAN_POINT('Ctrl Pts',(6.99999999886799,7.04445985882369,-22.5145575357774));
#49463=CARTESIAN_POINT('Ctrl Pts',(6.99999999981994,7.2197221995766,-22.7374276556396));
#49464=CARTESIAN_POINT('Ctrl Pts',(6.99999999992602,7.23925208826038,-22.7622625894488));
#49465=CARTESIAN_POINT('Ctrl Pts',(6.99999999999964,7.2588909847756,-22.7870146819099));
#49466=CARTESIAN_POINT('Ctrl Pts',(6.99999999999964,7.27863843674251,-22.811683068204));
#49467=CARTESIAN_POINT('Ctrl Pts',(6.99999999999964,7.4168811114768,-22.9843749024913));
#49468=CARTESIAN_POINT('Ctrl Pts',(6.99999999634605,7.56041237864492,-23.1529986871859));
#49469=CARTESIAN_POINT('Ctrl Pts',(6.99999999542156,7.70885456978368,-23.3170717122661));
#49470=CARTESIAN_POINT('Ctrl Pts',(6.99999999531129,7.72655977575305,-23.3366412610634));
#49471=CARTESIAN_POINT('Ctrl Pts',(6.99999999523589,7.74433480164425,-23.3561461126841));
#49472=CARTESIAN_POINT('Ctrl Pts',(6.99999999520038,7.76217897185983,-23.3755854834775));
#49473=CARTESIAN_POINT('Ctrl Pts',(6.99999999489231,7.91695873329861,-23.5442019636824));
#49474=CARTESIAN_POINT('Ctrl Pts',(6.99999999999964,8.07694373314969,-23.7078879606588));
#49475=CARTESIAN_POINT('Ctrl Pts',(6.99999999999964,8.24158930395947,-23.866242493597));
#49476=CARTESIAN_POINT('Ctrl Pts',(6.99999999999964,8.36428137259446,-23.9842465499974));
#49477=CARTESIAN_POINT('Ctrl Pts',(6.99999999741396,8.48959541717548,-24.0992443287782));
#49478=CARTESIAN_POINT('Ctrl Pts',(6.999999997457,8.61757747788213,-24.2113318768014));
#49479=CARTESIAN_POINT('Ctrl Pts',(6.99999999749808,8.73974118137153,-24.3183236685101));
#49480=CARTESIAN_POINT('Ctrl Pts',(6.99999999865099,8.86433631653384,-24.4226638135537));
#49481=CARTESIAN_POINT('Ctrl Pts',(6.9999999992403,8.99143397729645,-24.5244042570306));
#49482=CARTESIAN_POINT('Ctrl Pts',(6.99999999975841,9.10317464243632,-24.6138515746092));
#49483=CARTESIAN_POINT('Ctrl Pts',(6.99999999990827,9.21685018958274,-24.7012891605354));
#49484=CARTESIAN_POINT('Ctrl Pts',(6.99999999989361,9.33251047980344,-24.7867157008307));
#49485=CARTESIAN_POINT('Ctrl Pts',(6.26386081901915,3.90572621523646,-15.8144408559843));
#49486=CARTESIAN_POINT('Ctrl Pts',(6.26460715483143,3.90306655874706,-16.0736393146914));
#49487=CARTESIAN_POINT('Ctrl Pts',(6.26531568073978,3.9088164615582,-16.3306786832361));
#49488=CARTESIAN_POINT('Ctrl Pts',(6.26598637993336,3.92256301947529,-16.5850659454606));
#49489=CARTESIAN_POINT('Ctrl Pts',(6.26666472878982,3.93646636382485,-16.8423546228283));
#49490=CARTESIAN_POINT('Ctrl Pts',(6.26730438316959,3.95854979957321,-17.0969304079669));
#49491=CARTESIAN_POINT('Ctrl Pts',(6.26790532902729,3.98839267344383,-17.3483359936474));
#49492=CARTESIAN_POINT('Ctrl Pts',(6.26800175869402,3.99318135506081,-17.3886773264485));
#49493=CARTESIAN_POINT('Ctrl Pts',(6.26809719168382,3.99816984378879,-17.4289371396668));
#49494=CARTESIAN_POINT('Ctrl Pts',(6.26819162794592,4.00335641748679,-17.469113666875));
#49495=CARTESIAN_POINT('Ctrl Pts',(6.26876871361724,4.03505078253044,-17.7146263296978));
#49496=CARTESIAN_POINT('Ctrl Pts',(6.2693085788154,4.07414047215226,-17.9570248844362));
#49497=CARTESIAN_POINT('Ctrl Pts',(6.26981121343943,4.12010867076005,-18.1959008431826));
#49498=CARTESIAN_POINT('Ctrl Pts',(6.27017912193638,4.15375555867615,-18.3707485172967));
#49499=CARTESIAN_POINT('Ctrl Pts',(6.27052708362784,4.19108813783622,-18.5437099551103));
#49500=CARTESIAN_POINT('Ctrl Pts',(6.27085509534091,4.2319104395092,-18.7146413025029));
#49501=CARTESIAN_POINT('Ctrl Pts',(6.27121137967983,4.27625137669193,-18.900305898243));
#49502=CARTESIAN_POINT('Ctrl Pts',(6.2715441253586,4.32470945321996,-19.0835751290548));
#49503=CARTESIAN_POINT('Ctrl Pts',(6.27185332829706,4.37704091279458,-19.2642823708179));
#49504=CARTESIAN_POINT('Ctrl Pts',(6.27227096980512,4.44772520125795,-19.5083642846041));
#49505=CARTESIAN_POINT('Ctrl Pts',(6.27264565985936,4.52547487734651,-19.7477704244421));
#49506=CARTESIAN_POINT('Ctrl Pts',(6.27297739052688,4.60968091118585,-19.9821806569633));
#49507=CARTESIAN_POINT('Ctrl Pts',(6.27330912119439,4.6938869450252,-20.2165908894845));
#49508=CARTESIAN_POINT('Ctrl Pts',(6.27359789249436,4.78454940161974,-20.4460053998776));
#49509=CARTESIAN_POINT('Ctrl Pts',(6.27384369863648,4.88108706281011,-20.6701555296204));
#49510=CARTESIAN_POINT('Ctrl Pts',(6.27395596464763,4.92517830501504,-20.7725306808193));
#49511=CARTESIAN_POINT('Ctrl Pts',(6.27405926825717,4.9704954823184,-20.8738083811902));
#49512=CARTESIAN_POINT('Ctrl Pts',(6.27415361609019,5.01698510371503,-20.9739664611315));
#49513=CARTESIAN_POINT('Ctrl Pts',(6.27415651999336,5.01841599359143,-20.9770491961231));
#49514=CARTESIAN_POINT('Ctrl Pts',(6.2741594153517,5.01984799417455,-20.9801308705135));
#49515=CARTESIAN_POINT('Ctrl Pts',(6.27416230217101,5.02128110392859,-20.9832114836985));
#49516=CARTESIAN_POINT('Ctrl Pts',(6.27420631174089,5.04312886679225,-21.0301754417279));
#49517=CARTESIAN_POINT('Ctrl Pts',(6.27424833675569,5.06523440558947,-21.0768927576288));
#49518=CARTESIAN_POINT('Ctrl Pts',(6.2742883978265,5.08759148600678,-21.1233617479934));
#49519=CARTESIAN_POINT('Ctrl Pts',(6.27431785040983,5.10402823521087,-21.1575253832326));
#49520=CARTESIAN_POINT('Ctrl Pts',(6.2743467021673,5.12089395791622,-21.1921536959186));
#49521=CARTESIAN_POINT('Ctrl Pts',(6.27437398897063,5.1375813421622,-21.2260056020033));
#49522=CARTESIAN_POINT('Ctrl Pts',(6.27438625195006,5.14508083000008,-21.2412190083843));
#49523=CARTESIAN_POINT('Ctrl Pts',(6.27439819885563,5.15254365473743,-21.2562759175005));
#49524=CARTESIAN_POINT('Ctrl Pts',(6.27440974217502,5.15991163508647,-21.2710652003407));
#49525=CARTESIAN_POINT('Ctrl Pts',(6.27456064646664,5.25623227027768,-21.4644035440535));
#49526=CARTESIAN_POINT('Ctrl Pts',(6.27467736455278,5.35907892797542,-21.6577057407531));
#49527=CARTESIAN_POINT('Ctrl Pts',(6.2747598946937,5.46870212487468,-21.8504730214076));
#49528=CARTESIAN_POINT('Ctrl Pts',(6.27484107136038,5.57652752800879,-22.0400789655467));
#49529=CARTESIAN_POINT('Ctrl Pts',(6.27488917224047,5.69090909310062,-22.2291674455941));
#49530=CARTESIAN_POINT('Ctrl Pts',(6.27490419665066,5.81206997999551,-22.4172156503231));
#49531=CARTESIAN_POINT('Ctrl Pts',(6.27490863038766,5.84782482830833,-22.4727090955091));
#49532=CARTESIAN_POINT('Ctrl Pts',(6.27491018365568,5.88416995006603,-22.528111621419));
#49533=CARTESIAN_POINT('Ctrl Pts',(6.27490885645281,5.92111080747901,-22.5834089610956));
#49534=CARTESIAN_POINT('Ctrl Pts',(6.27490450801904,6.04214345090047,-22.7645845932802));
#49535=CARTESIAN_POINT('Ctrl Pts',(6.27486923844804,6.16957277182416,-22.9446345885511));
#49536=CARTESIAN_POINT('Ctrl Pts',(6.27480304820754,6.30354307114202,-23.1230244188957));
#49537=CARTESIAN_POINT('Ctrl Pts',(6.27475276959969,6.40530792487314,-23.2585306847215));
#49538=CARTESIAN_POINT('Ctrl Pts',(6.2746846496685,6.51084655159941,-23.3930781264593));
#49539=CARTESIAN_POINT('Ctrl Pts',(6.2745986889403,6.62021382699481,-23.5264141272963));
#49540=CARTESIAN_POINT('Ctrl Pts',(6.27448994453198,6.75856863043007,-23.6950905080506));
#49541=CARTESIAN_POINT('Ctrl Pts',(6.27435264758153,6.90305132253116,-23.8618296346804));
#49542=CARTESIAN_POINT('Ctrl Pts',(6.27418680056911,7.05375519708462,-24.0260820616461));
#49543=CARTESIAN_POINT('Ctrl Pts',(6.274013150482,7.21154966418197,-24.1980625383213));
#49544=CARTESIAN_POINT('Ctrl Pts',(6.27380820056856,7.37616533894926,-24.3673161423291));
#49545=CARTESIAN_POINT('Ctrl Pts',(6.27357195460688,7.5476343484384,-24.5332734929099));
#49546=CARTESIAN_POINT('Ctrl Pts',(6.27333930167313,7.71649551254562,-24.6967068240682));
#49547=CARTESIAN_POINT('Ctrl Pts',(6.27307629740119,7.89200319539931,-24.8569434210827));
#49548=CARTESIAN_POINT('Ctrl Pts',(6.27278294639037,8.07415574466986,-25.0134008439504));
#49549=CARTESIAN_POINT('Ctrl Pts',(6.27261681548821,8.17731259849041,-25.1020060024537));
#49550=CARTESIAN_POINT('Ctrl Pts',(6.27244095180671,8.28259999770744,-25.1893983995385));
#49551=CARTESIAN_POINT('Ctrl Pts',(6.27225535633498,8.39001281171083,-25.2754665765872));
#49552=CARTESIAN_POINT('Ctrl Pts',(6.27204648357802,8.51089728364193,-25.3723293785642));
#49553=CARTESIAN_POINT('Ctrl Pts',(6.27182528483322,8.63447390919248,-25.4675151877984));
#49554=CARTESIAN_POINT('Ctrl Pts',(6.27159176169366,8.76072155998436,-25.5608443101141));
#49555=CARTESIAN_POINT('Ctrl Pts',(-6.390310997166,3.94960612761086,-15.460427010644));
#49556=CARTESIAN_POINT('Ctrl Pts',(-4.260207331444,3.32899321753374,-16.2185125151969));
#49557=CARTESIAN_POINT('Ctrl Pts',(0.000153520239401,2.70682972226379,-16.9766167275286));
#49558=CARTESIAN_POINT('Ctrl Pts',(4.260514371923,3.32903805792829,-16.2184578773201));
#49559=CARTESIAN_POINT('Ctrl Pts',(6.390771557884,3.94974031835815,-15.4602630951545));
#49560=CARTESIAN_POINT('Ctrl Pts',(-6.390310997166,3.91824263644539,-16.2404224492195));
#49561=CARTESIAN_POINT('Ctrl Pts',(-4.260207331444,3.34435590545916,-16.9591796463154));
#49562=CARTESIAN_POINT('Ctrl Pts',(0.000153520239401,2.76852197294671,-17.6779444417002));
#49563=CARTESIAN_POINT('Ctrl Pts',(4.260514371923,3.34439740680201,-16.9591278436997));
#49564=CARTESIAN_POINT('Ctrl Pts',(6.390771557884,3.91836672392008,-16.24026703742));
#49565=CARTESIAN_POINT('Ctrl Pts',(-6.390310997166,4.02654093202666,-18.1258725679872));
#49566=CARTESIAN_POINT('Ctrl Pts',(-4.260207331444,3.53815115056139,-18.7395194904352));
#49567=CARTESIAN_POINT('Ctrl Pts',(0.0001535202393995,3.05107476647531,
-19.3531445395367));
#49568=CARTESIAN_POINT('Ctrl Pts',(4.260514371923,3.53818625499516,-18.7394752654212));
#49569=CARTESIAN_POINT('Ctrl Pts',(6.390771557884,4.02664653311775,-18.1257398834285));
#49570=CARTESIAN_POINT('Ctrl Pts',(-6.390310997166,4.89945800148072,-21.0044951210845));
#49571=CARTESIAN_POINT('Ctrl Pts',(-4.260207331444,4.44478850538018,-21.4424839510795));
#49572=CARTESIAN_POINT('Ctrl Pts',(0.0001535202394003,3.98943347064956,
-21.8807678511962));
#49573=CARTESIAN_POINT('Ctrl Pts',(4.260514371923,4.44482132360267,-21.4424523632058));
#49574=CARTESIAN_POINT('Ctrl Pts',(6.390771557884,4.89955631145556,-21.0044004178407));
#49575=CARTESIAN_POINT('Ctrl Pts',(-6.390310997166,6.63374317910258,-23.7052268139868));
#49576=CARTESIAN_POINT('Ctrl Pts',(-4.260207331444,6.09525793886643,-23.998130417564));
#49577=CARTESIAN_POINT('Ctrl Pts',(0.0001535202394,5.55782046091975,-24.2900534534943));
#49578=CARTESIAN_POINT('Ctrl Pts',(4.260514371923,6.09529667291084,-23.9981093781683));
#49579=CARTESIAN_POINT('Ctrl Pts',(6.390771557884,6.63385961198203,-23.7051634814939));
#49580=CARTESIAN_POINT('Ctrl Pts',(-6.390310997166,8.18394426417614,-25.1149800440698));
#49581=CARTESIAN_POINT('Ctrl Pts',(-4.260207331444,7.53598539108648,-25.3660541903064));
#49582=CARTESIAN_POINT('Ctrl Pts',(0.0001535202394001,6.88615442358477,
-25.6190324252077));
#49583=CARTESIAN_POINT('Ctrl Pts',(4.260514371923,7.53603222552418,-25.3660359577308));
#49584=CARTESIAN_POINT('Ctrl Pts',(6.390771557884,8.18408436774532,-25.1149257560885));
#49585=CARTESIAN_POINT('Ctrl Pts',(-6.390310997166,8.98425310970363,-25.6807323427288));
#49586=CARTESIAN_POINT('Ctrl Pts',(-4.260207331444,8.27686639982284,-25.9287942674702));
#49587=CARTESIAN_POINT('Ctrl Pts',(0.0001535202394001,7.5688707583203,-26.1774614807514));
#49588=CARTESIAN_POINT('Ctrl Pts',(4.260514371923,8.27691742628879,-25.9287763455956));
#49589=CARTESIAN_POINT('Ctrl Pts',(6.390771557884,8.98440606294867,-25.6806787060575));
#49590=CARTESIAN_POINT('Ctrl Pts',(-6.26386059950783,3.90573753004527,-15.8144217560873));
#49591=CARTESIAN_POINT('Ctrl Pts',(-5.97372627968023,3.82530519121327,-15.9109296281103));
#49592=CARTESIAN_POINT('Ctrl Pts',(-5.68164548281105,3.74986547664179,-16.0001140046338));
#49593=CARTESIAN_POINT('Ctrl Pts',(-5.38811095600305,3.67970569357336,-16.0820552820059));
#49594=CARTESIAN_POINT('Ctrl Pts',(-5.1129382354064,3.61393469690952,-16.1588707914754));
#49595=CARTESIAN_POINT('Ctrl Pts',(-4.83648797010696,3.55280433012687,-16.229320691623));
#49596=CARTESIAN_POINT('Ctrl Pts',(-4.55916610084168,3.49652988606607,-16.2935087073498));
#49597=CARTESIAN_POINT('Ctrl Pts',(-4.30168885183784,3.44428233312557,-16.3531035519689));
#49598=CARTESIAN_POINT('Ctrl Pts',(-4.04346027638,3.39622087517566,-16.4073005338585));
#49599=CARTESIAN_POINT('Ctrl Pts',(-3.78480525737339,3.35249305011429,-16.4562187999834));
#49600=CARTESIAN_POINT('Ctrl Pts',(-3.57018253931316,3.31620925904162,-16.4968094340984));
#49601=CARTESIAN_POINT('Ctrl Pts',(-3.35526621107239,3.28290892324508,-16.5337661150051));
#49602=CARTESIAN_POINT('Ctrl Pts',(-3.1402418783052,3.25265989964445,-16.5671788848135));
#49603=CARTESIAN_POINT('Ctrl Pts',(-2.90174875105576,3.219109351472,-16.6042384857393));
#49604=CARTESIAN_POINT('Ctrl Pts',(-2.66311062362395,3.18931283044879,-16.6369596995847));
#49605=CARTESIAN_POINT('Ctrl Pts',(-2.42457575010895,3.16332914900677,-16.6653611706952));
#49606=CARTESIAN_POINT('Ctrl Pts',(-2.18945145913184,3.13771698343113,-16.6933565562721));
#49607=CARTESIAN_POINT('Ctrl Pts',(-1.95442749052171,3.11580944452607,-16.7171548319756));
#49608=CARTESIAN_POINT('Ctrl Pts',(-1.71974160126147,3.09763059235909,-16.7368128800229));
#49609=CARTESIAN_POINT('Ctrl Pts',(-1.48657671707649,3.07956955778435,-16.7563435237727));
#49610=CARTESIAN_POINT('Ctrl Pts',(-1.25374554424066,3.0651890947204,-16.7717873914836));
#49611=CARTESIAN_POINT('Ctrl Pts',(-1.02148124690547,3.05447991685876,-16.7832395301357));
#49612=CARTESIAN_POINT('Ctrl Pts',(-0.790833753306384,3.04384528613577,
-16.7946119498608));
#49613=CARTESIAN_POINT('Ctrl Pts',(-0.560745270577479,3.03683103914573,
-16.8020480059554));
#49614=CARTESIAN_POINT('Ctrl Pts',(-0.331444127483368,3.03339486825846,
-16.8056800208761));
#49615=CARTESIAN_POINT('Ctrl Pts',(-0.220772843970497,3.03173641406442,
-16.807432998413));
#49616=CARTESIAN_POINT('Ctrl Pts',(-0.110284969003811,3.0309109629497,-16.8083004233882));
#49617=CARTESIAN_POINT('Ctrl Pts',(-6.17382099488752E-6,3.0309109343344,
-16.8083004870552));
#49618=CARTESIAN_POINT('Ctrl Pts',(-4.11588034283447E-6,3.03091093433386,
-16.8083004870564));
#49619=CARTESIAN_POINT('Ctrl Pts',(-2.05793961891125E-6,3.03091093433362,
-16.8083004870572));
#49620=CARTESIAN_POINT('Ctrl Pts',(1.1750539249883E-12,3.03091093433366,
-16.8083004870578));
#49621=CARTESIAN_POINT('Ctrl Pts',(0.230475565322468,3.03091093890162,-16.8083005524742));
#49622=CARTESIAN_POINT('Ctrl Pts',(0.461841095866946,3.03451839678727,-16.8045094946044));
#49623=CARTESIAN_POINT('Ctrl Pts',(0.693872690690212,3.04179180534984,-16.7967739675693));
#49624=CARTESIAN_POINT('Ctrl Pts',(0.927916161739583,3.04912827945217,-16.7889713681041));
#49625=CARTESIAN_POINT('Ctrl Pts',(1.16263729762952,3.06019453604654,-16.7771555978514));
#49626=CARTESIAN_POINT('Ctrl Pts',(1.39780632263695,3.0750161307351,-16.7612097989639));
#49627=CARTESIAN_POINT('Ctrl Pts',(1.63455675554439,3.08993739410635,-16.7451567716167));
#49628=CARTESIAN_POINT('Ctrl Pts',(1.871761121536,3.10866461740418,-16.7249180178633));
#49629=CARTESIAN_POINT('Ctrl Pts',(2.10918497822673,3.13118963469091,-16.7004149289351));
#49630=CARTESIAN_POINT('Ctrl Pts',(2.34961346391676,3.1539997089264,-16.6756017503109));
#49631=CARTESIAN_POINT('Ctrl Pts',(2.59026703082308,3.18070426197141,-16.6464156411019));
#49632=CARTESIAN_POINT('Ctrl Pts',(2.83090222275172,3.21126053308359,-16.6128161441932));
#49633=CARTESIAN_POINT('Ctrl Pts',(2.93386713401478,3.22433519485014,-16.5984393226237));
#49634=CARTESIAN_POINT('Ctrl Pts',(3.03682868103732,3.23811464118123,-16.5832549690811));
#49635=CARTESIAN_POINT('Ctrl Pts',(3.13976779116438,3.2525936804676,-16.5672621526594));
#49636=CARTESIAN_POINT('Ctrl Pts',(3.40252257005505,3.28955180805919,-16.5264400692207));
#49637=CARTESIAN_POINT('Ctrl Pts',(3.66512621014034,3.33106867965023,-16.4803234953586));
#49638=CARTESIAN_POINT('Ctrl Pts',(3.92723945364459,3.37701812899252,-16.4287510375096));
#49639=CARTESIAN_POINT('Ctrl Pts',(4.19826717559078,3.4245303203394,-16.3754245989859));
#49640=CARTESIAN_POINT('Ctrl Pts',(4.4687705769213,3.47678129432531,-16.3162651879646));
#49641=CARTESIAN_POINT('Ctrl Pts',(4.73837459477634,3.53359543051034,-16.2511431923738));
#49642=CARTESIAN_POINT('Ctrl Pts',(5.03395192678833,3.595882969575,-16.1797474251104));
#49643=CARTESIAN_POINT('Ctrl Pts',(5.32844823704742,3.66365486004385,-16.1011849319197));
#49644=CARTESIAN_POINT('Ctrl Pts',(5.62136928502598,3.73664288696887,-16.0153401939371));
#49645=CARTESIAN_POINT('Ctrl Pts',(5.83644665881003,3.79023436923702,-15.9523086674358));
#49646=CARTESIAN_POINT('Ctrl Pts',(6.05067477162441,3.84663711861222,-15.8853523700907));
#49647=CARTESIAN_POINT('Ctrl Pts',(6.26385797755097,3.90573660178328,-15.8144409707664));
#49648=CARTESIAN_POINT('Ctrl Pts',(-6.38246269292625,3.93894967362139,-15.7729097725756));
#49649=CARTESIAN_POINT('Ctrl Pts',(-5.83395600374064,3.78387662728214,-15.9702601123439));
#49650=CARTESIAN_POINT('Ctrl Pts',(-4.51676965304293,3.45862254641806,-16.3719120782295));
#49651=CARTESIAN_POINT('Ctrl Pts',(-2.37673153344301,3.11825374849332,-16.7692680861992));
#49652=CARTESIAN_POINT('Ctrl Pts',(0.000175407413350786,2.99129135223685,
-16.9125154471428));
#49653=CARTESIAN_POINT('Ctrl Pts',(2.37708240512334,3.11829116289182,-16.7692254872644));
#49654=CARTESIAN_POINT('Ctrl Pts',(4.51699670078421,3.45867323308068,-16.3718511298187));
#49655=CARTESIAN_POINT('Ctrl Pts',(5.83406738808232,3.78390812439344,-15.9702199714471));
#49656=CARTESIAN_POINT('Ctrl Pts',(6.38246334095398,3.93894987729812,-15.7729094699168));
#49657=CARTESIAN_POINT('Ctrl Pts',(-6.17758168919576,3.88967198539074,-15.154162882923));
#49658=CARTESIAN_POINT('Ctrl Pts',(-5.64640092257065,3.74166898124023,-15.3452128053215));
#49659=CARTESIAN_POINT('Ctrl Pts',(-4.370973200626,3.43112903201519,-15.7340791545028));
#49660=CARTESIAN_POINT('Ctrl Pts',(-2.29961550285046,3.10606644179156,-16.118753707528));
#49661=CARTESIAN_POINT('Ctrl Pts',(0.000169703128138686,2.98481674989937,
-16.257404296828));
#49662=CARTESIAN_POINT('Ctrl Pts',(2.29995503766859,3.10610217341112,-16.1187124731847));
#49663=CARTESIAN_POINT('Ctrl Pts',(4.37119302862394,3.43117743709702,-15.7340201451118));
#49664=CARTESIAN_POINT('Ctrl Pts',(5.64650878850444,3.74169904124616,-15.3451739455801));
#49665=CARTESIAN_POINT('Ctrl Pts',(6.1775823172684,3.88967217936339,-15.15416258936));
#49666=CARTESIAN_POINT('Ctrl Pts',(-6.17627524027959,3.38234690796609,-14.7450182290604));
#49667=CARTESIAN_POINT('Ctrl Pts',(-5.64643658833439,3.23615773351961,-14.9338120192099));
#49668=CARTESIAN_POINT('Ctrl Pts',(-4.37356735177373,2.92910800412423,-15.3184353559978));
#49669=CARTESIAN_POINT('Ctrl Pts',(-2.30271816604516,2.60683192149392,-15.6997831889741));
#49670=CARTESIAN_POINT('Ctrl Pts',(0.000169988787698856,2.48637475214055,
-15.8374778743519));
#49671=CARTESIAN_POINT('Ctrl Pts',(2.30305795089379,2.60686739928376,-15.6997422594087));
#49672=CARTESIAN_POINT('Ctrl Pts',(4.37378683344432,2.92915591510232,-15.3183769362156));
#49673=CARTESIAN_POINT('Ctrl Pts',(5.64654418199573,3.23618742585186,-14.9337736202781));
#49674=CARTESIAN_POINT('Ctrl Pts',(6.17627586451967,3.38234709913452,-14.7450179412791));
#49675=CARTESIAN_POINT('Ctrl Pts',(-6.37670151809056,2.76894332529829,-14.8215582716457));
#49676=CARTESIAN_POINT('Ctrl Pts',(-5.83152084753289,2.61814590976835,-15.0136238374691));
#49677=CARTESIAN_POINT('Ctrl Pts',(-4.52079209118095,2.30113400780086,-15.4053243805069));
#49678=CARTESIAN_POINT('Ctrl Pts',(-2.3828478805525,1.96739333350805,-15.794842346463));
#49679=CARTESIAN_POINT('Ctrl Pts',(0.000175989273597215,1.84233431609406,
-15.9358247251825));
#49680=CARTESIAN_POINT('Ctrl Pts',(2.38319917637242,1.96743014026188,-15.7948004683328));
#49681=CARTESIAN_POINT('Ctrl Pts',(4.52101824376224,2.30118352497297,-15.4052648171334));
#49682=CARTESIAN_POINT('Ctrl Pts',(5.83163155708262,2.61817654012613,-15.0135847758853));
#49683=CARTESIAN_POINT('Ctrl Pts',(6.37670215701753,2.7689435223799,-14.8215579824318));
#49684=CARTESIAN_POINT('Ctrl Pts',(-6.24994460521886,2.76546685544382,-14.8593819056678));
#49685=CARTESIAN_POINT('Ctrl Pts',(-5.99094249999219,2.69516002979088,-14.9486425804541));
#49686=CARTESIAN_POINT('Ctrl Pts',(-5.72720728127898,2.62787545102769,-15.0328670687827));
#49687=CARTESIAN_POINT('Ctrl Pts',(-5.45886142643465,2.56415819329477,-15.1117505190932));
#49688=CARTESIAN_POINT('Ctrl Pts',(-5.22285449580001,2.50811963650497,-15.181127558647));
#49689=CARTESIAN_POINT('Ctrl Pts',(-4.98328152550268,2.45484087388617,-15.2463730336044));
#49690=CARTESIAN_POINT('Ctrl Pts',(-4.74024475778304,2.40471692783325,-15.3072665448488));
#49691=CARTESIAN_POINT('Ctrl Pts',(-4.72533948106778,2.40164286092153,-15.3110011017382));
#49692=CARTESIAN_POINT('Ctrl Pts',(-4.71042120035891,2.39858060782454,-15.3147192911877));
#49693=CARTESIAN_POINT('Ctrl Pts',(-4.69548992988297,2.39553024632854,-15.3184210658687));
#49694=CARTESIAN_POINT('Ctrl Pts',(-4.45028046023139,2.34543554568759,-15.3792136292185));
#49695=CARTESIAN_POINT('Ctrl Pts',(-4.20156648623987,2.29854558829399,-15.4355808996657));
#49696=CARTESIAN_POINT('Ctrl Pts',(-3.94948718691868,2.25519371924219,-15.4873109946335));
#49697=CARTESIAN_POINT('Ctrl Pts',(-3.8157727435299,2.23219789588131,-15.5147510139992));
#49698=CARTESIAN_POINT('Ctrl Pts',(-3.6811117686411,2.21019665045448,-15.5408860893749));
#49699=CARTESIAN_POINT('Ctrl Pts',(-3.545527931086,2.18923389337213,-15.5656831929245));
#49700=CARTESIAN_POINT('Ctrl Pts',(-3.47773601230845,2.17875251483096,-15.5780817446993));
#49701=CARTESIAN_POINT('Ctrl Pts',(-3.4097133744286,2.16853075563841,-15.5901457844336));
#49702=CARTESIAN_POINT('Ctrl Pts',(-3.34146322033014,2.15857364302317,-15.601871087987));
#49703=CARTESIAN_POINT('Ctrl Pts',(-3.30733814328091,2.15359508671555,-15.6077337397637));
#49704=CARTESIAN_POINT('Ctrl Pts',(-3.27315618700011,2.14868269188944,-15.6135117062827));
#49705=CARTESIAN_POINT('Ctrl Pts',(-3.23891775843242,2.14383707189763,-15.6192044529497));
#49706=CARTESIAN_POINT('Ctrl Pts',(-3.22179854414857,2.14141426190172,-15.6220508262832));
#49707=CARTESIAN_POINT('Ctrl Pts',(-3.2046652117838,2.1390081456044,-15.6248758945757));
#49708=CARTESIAN_POINT('Ctrl Pts',(-3.187517813095,2.13661879796061,-15.6276795906241));
#49709=CARTESIAN_POINT('Ctrl Pts',(-3.17037041440618,2.13422945031681,-15.6304832866724));
#49710=CARTESIAN_POINT('Ctrl Pts',(-3.15207046448132,2.13170072040929,-15.6334486169825));
#49711=CARTESIAN_POINT('Ctrl Pts',(-3.13603347006549,2.12950113539336,-15.6360264945505));
#49712=CARTESIAN_POINT('Ctrl Pts',(-2.87501520781348,2.0937006703159,-15.6779840525346));
#49713=CARTESIAN_POINT('Ctrl Pts',(-2.61248816369087,2.06209953498922,-15.7147041617999));
#49714=CARTESIAN_POINT('Ctrl Pts',(-2.34863686523688,2.03493974475676,-15.7461369357379));
#49715=CARTESIAN_POINT('Ctrl Pts',(-2.04845599284398,2.00404033446862,-15.7818976750548));
#49716=CARTESIAN_POINT('Ctrl Pts',(-1.74656066392248,1.97888880541283,-15.8108155701126));
#49717=CARTESIAN_POINT('Ctrl Pts',(-1.44332961648421,1.95966138466728,-15.8328336538368));
#49718=CARTESIAN_POINT('Ctrl Pts',(-1.14508568668948,1.94075018948653,-15.8544896150977));
#49719=CARTESIAN_POINT('Ctrl Pts',(-0.845549100638975,1.9275697949549,-15.869470795419));
#49720=CARTESIAN_POINT('Ctrl Pts',(-0.545085108667407,1.92032135217525,
-15.8776861228819));
#49721=CARTESIAN_POINT('Ctrl Pts',(-0.363702352701681,1.91594564472622,
-15.8826455149428));
#49722=CARTESIAN_POINT('Ctrl Pts',(-0.181981756268516,1.91373233336849,
-15.885138558788));
#49723=CARTESIAN_POINT('Ctrl Pts',(-5.73471096132168E-6,1.91373185585388,
-15.8851386642953));
#49724=CARTESIAN_POINT('Ctrl Pts',(5.39138121133536E-5,1.91373185569736,
-15.8851386643299));
#49725=CARTESIAN_POINT('Ctrl Pts',(0.00011356230696275,1.91373185577524,
-15.885138664097));
#49726=CARTESIAN_POINT('Ctrl Pts',(0.000173210773584176,1.91373185608752,
-15.8851386635966));
#49727=CARTESIAN_POINT('Ctrl Pts',(0.297559266330309,1.91373341299712,-15.8851361688966));
#49728=CARTESIAN_POINT('Ctrl Pts',(0.594244088085259,1.91955829910996,-15.8784882520397));
#49729=CARTESIAN_POINT('Ctrl Pts',(0.889890545446005,1.93109463048215,-15.8652927006163));
#49730=CARTESIAN_POINT('Ctrl Pts',(1.12073841233604,1.94010247557111,-15.8549892965919));
#49731=CARTESIAN_POINT('Ctrl Pts',(1.35095322925663,1.95259331338095,-15.8406930825171));
#49732=CARTESIAN_POINT('Ctrl Pts',(1.58037070720459,1.9685285947701,-15.8224346483479));
#49733=CARTESIAN_POINT('Ctrl Pts',(1.83765030286678,1.98639917197822,-15.8019587778847));
#49734=CARTESIAN_POINT('Ctrl Pts',(2.09393063440068,2.00857720947524,-15.7765029281989));
#49735=CARTESIAN_POINT('Ctrl Pts',(2.34899413482236,2.03488903452172,-15.7461056736265));
#49736=CARTESIAN_POINT('Ctrl Pts',(2.35332241868072,2.03533553136445,-15.7455898493471));
#49737=CARTESIAN_POINT('Ctrl Pts',(2.35765035237713,2.03578321905682,-15.7450726015952));
#49738=CARTESIAN_POINT('Ctrl Pts',(2.36197793520127,2.03623209616452,-15.7445539306617));
#49739=CARTESIAN_POINT('Ctrl Pts',(2.49165282103475,2.04968258112567,-15.7290120919899));
#49740=CARTESIAN_POINT('Ctrl Pts',(2.62101226358897,2.06419998622132,-15.7121926420529));
#49741=CARTESIAN_POINT('Ctrl Pts',(2.75002880797683,2.07975509189862,-15.6941026937445));
#49742=CARTESIAN_POINT('Ctrl Pts',(2.81453708017076,2.08753264473727,-15.6850577195903));
#49743=CARTESIAN_POINT('Ctrl Pts',(2.87895962758892,2.09556962127403,-15.6756951086055));
#49744=CARTESIAN_POINT('Ctrl Pts',(2.94329309702094,2.10386188537721,-15.6660157300993));
#49745=CARTESIAN_POINT('Ctrl Pts',(2.97545983173696,2.10800801742881,-15.6611760408462));
#49746=CARTESIAN_POINT('Ctrl Pts',(3.0076042969285,2.1122179712847,-15.6562571589625));
#49747=CARTESIAN_POINT('Ctrl Pts',(3.0397260755728,2.11649121694422,-15.6512591900128));
#49748=CARTESIAN_POINT('Ctrl Pts',(3.05578696489494,2.11862783977398,-15.648760205538));
#49749=CARTESIAN_POINT('Ctrl Pts',(3.07184218257719,2.12078028554911,-15.6462414492505));
#49750=CARTESIAN_POINT('Ctrl Pts',(3.08789167676611,2.12294848633111,-15.6437029342547));
#49751=CARTESIAN_POINT('Ctrl Pts',(3.10394117095503,2.1251166871131,-15.6411644192589));
#49752=CARTESIAN_POINT('Ctrl Pts',(3.11884751751632,2.12714464314771,-15.6387889801949));
#49753=CARTESIAN_POINT('Ctrl Pts',(3.13602293707478,2.1295002852458,-15.6360281261192));
#49754=CARTESIAN_POINT('Ctrl Pts',(3.41741466579409,2.16809370649934,-15.5907959558965));
#49755=CARTESIAN_POINT('Ctrl Pts',(3.69506739828332,2.21131136347053,-15.5397930462567));
#49756=CARTESIAN_POINT('Ctrl Pts',(3.96874459550752,2.25866743763374,-15.4833263036421));
#49757=CARTESIAN_POINT('Ctrl Pts',(4.21434190285783,2.30116467313283,-15.4326531745628));
#49758=CARTESIAN_POINT('Ctrl Pts',(4.45673811956246,2.34699530799611,-15.3775795312776));
#49759=CARTESIAN_POINT('Ctrl Pts',(4.69578022911293,2.39583435949049,-15.318310772496));
#49760=CARTESIAN_POINT('Ctrl Pts',(4.97402015772782,2.45268197611741,-15.2493231985346));
#49761=CARTESIAN_POINT('Ctrl Pts',(5.24771606928571,2.51360455783964,-15.1746524946147));
#49762=CARTESIAN_POINT('Ctrl Pts',(5.5167488360978,2.57809132060363,-15.0946099661954));
#49763=CARTESIAN_POINT('Ctrl Pts',(5.76514914613282,2.63763251349824,-15.0207059986194));
#49764=CARTESIAN_POINT('Ctrl Pts',(6.00957444404958,2.70021279219826,-14.9422222022724));
#49765=CARTESIAN_POINT('Ctrl Pts',(6.24994323895025,2.76546151517861,-14.8593832382704));
#49766=CARTESIAN_POINT('Ctrl Pts',(7.10527469285759,-5.08837285721628,-15.2149674210636));
#49767=CARTESIAN_POINT('Ctrl Pts',(7.10577175309562,-5.05127732240867,-15.2272006288549));
#49768=CARTESIAN_POINT('Ctrl Pts',(7.10233361655264,-4.93362690673713,-15.2672676676193));
#49769=CARTESIAN_POINT('Ctrl Pts',(7.06814935170305,-4.72835757096628,-15.3442190548759));
#49770=CARTESIAN_POINT('Ctrl Pts',(6.97357315551598,-4.48015474944715,-15.4505389279076));
#49771=CARTESIAN_POINT('Ctrl Pts',(6.81834137563527,-4.24729988507321,-15.5671389409917));
#49772=CARTESIAN_POINT('Ctrl Pts',(6.60934038952052,-4.05649431802118,-15.6839486604479));
#49773=CARTESIAN_POINT('Ctrl Pts',(6.40994316745287,-3.9505452960972,-15.77095398068));
#49774=CARTESIAN_POINT('Ctrl Pts',(6.28626990966703,-3.91128985961304,-15.8165793739769));
#49775=CARTESIAN_POINT('Ctrl Pts',(6.24914971117037,-3.90167129702033,-15.829595813689));
#49776=CARTESIAN_POINT('Ctrl Pts',(6.81642516792956,-4.90351678924822,-14.6670079284464));
#49777=CARTESIAN_POINT('Ctrl Pts',(6.81687157292555,-4.87082825456401,-14.6777811179155));
#49778=CARTESIAN_POINT('Ctrl Pts',(6.81378644819866,-4.76705724898886,-14.7131664511101));
#49779=CARTESIAN_POINT('Ctrl Pts',(6.78300083518967,-4.58570531998746,-14.7816063849249));
#49780=CARTESIAN_POINT('Ctrl Pts',(6.69776708002038,-4.36656036449269,-14.8767160883548));
#49781=CARTESIAN_POINT('Ctrl Pts',(6.55813791989439,-4.16163596433278,-14.9812858449522));
#49782=CARTESIAN_POINT('Ctrl Pts',(6.3708916441972,-3.99466535000316,-15.0859722384302));
#49783=CARTESIAN_POINT('Ctrl Pts',(6.19324335984852,-3.90268987971195,-15.1636514989911));
#49784=CARTESIAN_POINT('Ctrl Pts',(6.08361516941286,-3.8688401576237,-15.2041933227212));
#49785=CARTESIAN_POINT('Ctrl Pts',(6.05076212875822,-3.86056538918408,-15.215740706429));
#49786=CARTESIAN_POINT('Ctrl Pts',(7.05949177097581,-4.7187225394648,-14.0973262672783));
#49787=CARTESIAN_POINT('Ctrl Pts',(7.06007854662092,-4.67643436909571,-14.1112731878018));
#49788=CARTESIAN_POINT('Ctrl Pts',(7.05601182042207,-4.54261602000926,-14.1568412078288));
#49789=CARTESIAN_POINT('Ctrl Pts',(7.01591712851095,-4.31014738785563,-14.2439120150253));
#49790=CARTESIAN_POINT('Ctrl Pts',(6.90517332848893,-4.02902460202869,-14.3641431158811));
#49791=CARTESIAN_POINT('Ctrl Pts',(6.72258565932859,-3.76383137770917,-14.4967470520898));
#49792=CARTESIAN_POINT('Ctrl Pts',(6.47447165821453,-3.54432976015602,-14.6311667794549));
#49793=CARTESIAN_POINT('Ctrl Pts',(6.23472572267083,-3.42079528084269,-14.733085402626));
#49794=CARTESIAN_POINT('Ctrl Pts',(6.08433124395451,-3.3746170314338,-14.7874360195946));
#49795=CARTESIAN_POINT('Ctrl Pts',(6.03903337281355,-3.36327931177702,-14.8030279496368));
#49796=CARTESIAN_POINT('Ctrl Pts',(7.66941902033053,-4.65925181838288,-13.8920899655214));
#49797=CARTESIAN_POINT('Ctrl Pts',(7.6702419374224,-4.59987218133953,-13.9116905082337));
#49798=CARTESIAN_POINT('Ctrl Pts',(7.66452510755031,-4.41247144972349,-13.975395110386));
#49799=CARTESIAN_POINT('Ctrl Pts',(7.60873074023539,-4.08854266857875,-14.0955952751784));
#49800=CARTESIAN_POINT('Ctrl Pts',(7.45493552358401,-3.69646802310441,-14.2602308509189));
#49801=CARTESIAN_POINT('Ctrl Pts',(7.1999797850509,-3.32370834451298,-14.4419084359676));
#49802=CARTESIAN_POINT('Ctrl Pts',(6.84968015880541,-3.01095984373919,-14.6277404369394));
#49803=CARTESIAN_POINT('Ctrl Pts',(6.50612889451362,-2.83175107132688,-14.7710147674676));
#49804=CARTESIAN_POINT('Ctrl Pts',(6.28782028218345,-2.76387668293926,-14.8486958800387));
#49805=CARTESIAN_POINT('Ctrl Pts',(6.22181049242793,-2.74714790790825,-14.8711013367127));
#49806=CARTESIAN_POINT('',(6.26385989016308,-3.90573722907187,-15.8144313885695));
#49807=CARTESIAN_POINT('',(6.24996242253145,-2.76547028474026,-14.8593821272229));
#49808=CARTESIAN_POINT('Origin',(6.527838794926,-2.94126717711685,-15.8037762219005));
#49809=CARTESIAN_POINT('',(6.99999979527712,-3.16612999317638,-14.5427403187255));
#49810=CARTESIAN_POINT('Ctrl Pts',(6.99999979527712,-3.16612999317638,-14.5427403187255));
#49811=CARTESIAN_POINT('Ctrl Pts',(6.96025925123918,-3.13150165427226,-14.5635935033793));
#49812=CARTESIAN_POINT('Ctrl Pts',(6.91940655197007,-3.09881147495865,-14.5841219942725));
#49813=CARTESIAN_POINT('Ctrl Pts',(6.87749829651554,-3.06800285157106,-14.6043423325847));
#49814=CARTESIAN_POINT('Ctrl Pts',(6.86185360058381,-3.05650173944537,-14.6118907509357));
#49815=CARTESIAN_POINT('Ctrl Pts',(6.84606134376919,-3.04526309517268,-14.6193962484639));
#49816=CARTESIAN_POINT('Ctrl Pts',(6.83012290677287,-3.03428495759989,-14.6268597356979));
#49817=CARTESIAN_POINT('Ctrl Pts',(6.78727089454268,-3.0047691847771,-14.6469260349407));
#49818=CARTESIAN_POINT('Ctrl Pts',(6.74336503020372,-2.9771339417348,-14.6666887601211));
#49819=CARTESIAN_POINT('Ctrl Pts',(6.69843860682942,-2.95134978681162,-14.6861604765471));
#49820=CARTESIAN_POINT('Ctrl Pts',(6.68185279676599,-2.94183086533775,-14.6933489898093));
#49821=CARTESIAN_POINT('Ctrl Pts',(6.66512751469401,-2.93256458045001,-14.7004978259819));
#49822=CARTESIAN_POINT('Ctrl Pts',(6.64826319259013,-2.92355073295329,-14.7076075327013));
#49823=CARTESIAN_POINT('Ctrl Pts',(6.60317001610057,-2.89944878485744,-14.7266180365279));
#49824=CARTESIAN_POINT('Ctrl Pts',(6.55709254862238,-2.8771564114029,-14.7453451674277));
#49825=CARTESIAN_POINT('Ctrl Pts',(6.51001371638684,-2.85669396795406,-14.7637988395615));
#49826=CARTESIAN_POINT('Ctrl Pts',(6.47779611569965,-2.84269084169084,-14.7764272972311));
#49827=CARTESIAN_POINT('Ctrl Pts',(6.44510892339048,-2.82954552561692,-14.788927602381));
#49828=CARTESIAN_POINT('Ctrl Pts',(6.41194011923371,-2.81727689091429,-14.801301031713));
#49829=CARTESIAN_POINT('Ctrl Pts',(6.36428119018118,-2.79964858004421,-14.8190799177978));
#49830=CARTESIAN_POINT('Ctrl Pts',(6.31562823555339,-2.78382801429811,-14.8365973961792));
#49831=CARTESIAN_POINT('Ctrl Pts',(6.26596696981809,-2.76988784963211,-14.8538446148066));
#49832=CARTESIAN_POINT('Ctrl Pts',(6.26065696768343,-2.76839730558258,-14.8556887636895));
#49833=CARTESIAN_POINT('Ctrl Pts',(6.25533542719756,-2.76692830682691,-14.8575298123915));
#49834=CARTESIAN_POINT('Ctrl Pts',(6.25000232416703,-2.76548097644809,-14.8593677423417));
#49835=CARTESIAN_POINT('',(6.99999610169145,-4.92964753519558,-14.7967972847303));
#49836=CARTESIAN_POINT('Ctrl Pts',(6.99999610169145,-4.92964753519558,-14.7967972847303));
#49837=CARTESIAN_POINT('Ctrl Pts',(6.99999610613836,-4.91661229043681,-14.791628391893));
#49838=CARTESIAN_POINT('Ctrl Pts',(7.00000000000004,-4.90361602938088,-14.7863598515099));
#49839=CARTESIAN_POINT('Ctrl Pts',(7.00000000000004,-4.68651912055677,-14.7023782689544));
#49840=CARTESIAN_POINT('Ctrl Pts',(7.,-4.37639477651136,-14.5833717164819));
#49841=CARTESIAN_POINT('Ctrl Pts',(7.,-3.62764529519874,-14.4736742989645));
#49842=CARTESIAN_POINT('Ctrl Pts',(7.,-3.36166428568053,-14.5001704079875));
#49843=CARTESIAN_POINT('Ctrl Pts',(7.,-3.16613006334553,-14.5427402348609));
#49844=CARTESIAN_POINT('Ctrl Pts',(6.9999961018476,-4.92964640469684,-14.7967897782623));
#49845=CARTESIAN_POINT('Ctrl Pts',(6.99999545357539,-4.90144163830488,-14.8174799284486));
#49846=CARTESIAN_POINT('Ctrl Pts',(6.99899242211926,-4.87385494684075,-14.8379871689643));
#49847=CARTESIAN_POINT('Ctrl Pts',(6.99710015379376,-4.84694425873787,-14.8582529829778));
#49848=CARTESIAN_POINT('Ctrl Pts',(6.99462095173791,-4.81168655645035,-14.8848047394535));
#49849=CARTESIAN_POINT('Ctrl Pts',(6.99061682905021,-4.77758978796254,-14.9109414498812));
#49850=CARTESIAN_POINT('Ctrl Pts',(6.98535378928391,-4.74472637574954,-14.9365584985346));
#49851=CARTESIAN_POINT('Ctrl Pts',(6.97984402030381,-4.71032233982514,-14.9633764642539));
#49852=CARTESIAN_POINT('Ctrl Pts',(6.9729541530082,-4.6772700776306,-14.9896249687013));
#49853=CARTESIAN_POINT('Ctrl Pts',(6.9649510374448,-4.64562082080034,-15.0152097168229));
#49854=CARTESIAN_POINT('Ctrl Pts',(6.96448148193806,-4.64376390861269,-15.0167108146483));
#49855=CARTESIAN_POINT('Ctrl Pts',(6.96400808470404,-4.64191181719858,-15.0182096344437));
#49856=CARTESIAN_POINT('Ctrl Pts',(6.96353089618533,-4.64006455362156,-15.0197061596802));
#49857=CARTESIAN_POINT('Ctrl Pts',(6.95827901842607,-4.61973379939072,-15.0361767311584));
#49858=CARTESIAN_POINT('Ctrl Pts',(6.9525684519033,-4.59998814679231,-15.0523690733808));
#49859=CARTESIAN_POINT('Ctrl Pts',(6.94647157041035,-4.58082833485301,-15.0682640391052));
#49860=CARTESIAN_POINT('Ctrl Pts',(6.93624916912817,-4.54870383212791,-15.0949145026561));
#49861=CARTESIAN_POINT('Ctrl Pts',(6.92494289805191,-4.51822761460672,-15.1207277618141));
#49862=CARTESIAN_POINT('Ctrl Pts',(6.91285653739889,-4.48938067867097,-15.1456340112259));
#49863=CARTESIAN_POINT('Ctrl Pts',(6.90347902408293,-4.46699904257488,-15.1649581644772));
#49864=CARTESIAN_POINT('Ctrl Pts',(6.89363089342732,-4.44559760714516,-15.1837368697021));
#49865=CARTESIAN_POINT('Ctrl Pts',(6.88343785827852,-4.42515687040387,-15.2019466950999));
#49866=CARTESIAN_POINT('Ctrl Pts',(6.87592821023104,-4.41009729918515,-15.2153626578379));
#49867=CARTESIAN_POINT('Ctrl Pts',(6.86823115088852,-4.39555891832723,-15.2284700122123));
#49868=CARTESIAN_POINT('Ctrl Pts',(6.86039673372419,-4.38152778746263,-15.2412620985545));
#49869=CARTESIAN_POINT('Ctrl Pts',(6.85503441981097,-4.37192409561483,-15.2500177189322));
#49870=CARTESIAN_POINT('Ctrl Pts',(6.84960766117097,-4.36255800803777,-15.2586256824296));
#49871=CARTESIAN_POINT('Ctrl Pts',(6.84413136976615,-4.35342466366611,-15.2670843255968));
#49872=CARTESIAN_POINT('Ctrl Pts',(6.84139322406374,-4.34885799148029,-15.2713136471804));
#49873=CARTESIAN_POINT('Ctrl Pts',(6.83864268736027,-4.34434951010423,-15.2755056389739));
#49874=CARTESIAN_POINT('Ctrl Pts',(6.83588153604075,-4.33989857293696,-15.2796601323838));
#49875=CARTESIAN_POINT('Ctrl Pts',(6.83450096038099,-4.33767310435332,-15.2817373790888));
#49876=CARTESIAN_POINT('Ctrl Pts',(6.83311773059012,-4.33546202211664,-15.2838052512154));
#49877=CARTESIAN_POINT('Ctrl Pts',(6.83173206482601,-4.33326524533274,-15.2858637287704));
#49878=CARTESIAN_POINT('Ctrl Pts',(6.83065726241951,-4.33156129836729,-15.2874604028653));
#49879=CARTESIAN_POINT('Ctrl Pts',(6.83004028587927,-4.33058748223666,-15.2883741809166));
#49880=CARTESIAN_POINT('Ctrl Pts',(6.82881311612304,-4.32866432005909,-15.2901810082252));
#49881=CARTESIAN_POINT('Ctrl Pts',(6.82845818380387,-4.32810808698022,-15.2907035939586));
#49882=CARTESIAN_POINT('Ctrl Pts',(6.82805199550011,-4.32747259371732,-15.2913008776399));
#49883=CARTESIAN_POINT('Ctrl Pts',(6.82756797534166,-4.32671775049805,-15.2920109583931));
#49884=CARTESIAN_POINT('Ctrl Pts',(6.80355964120888,-4.28927606979582,-15.3272323343803));
#49885=CARTESIAN_POINT('Ctrl Pts',(6.77748021137456,-4.25387016495786,-15.3617950155865));
#49886=CARTESIAN_POINT('Ctrl Pts',(6.74960463512441,-4.22067176874938,-15.395577183151));
#49887=CARTESIAN_POINT('Ctrl Pts',(6.71795255192088,-4.18297574447406,-15.4339360665316));
#49888=CARTESIAN_POINT('Ctrl Pts',(6.6839859149371,-4.14812527207758,-15.4712883958782));
#49889=CARTESIAN_POINT('Ctrl Pts',(6.64816824301974,-4.11626345192712,-15.5074860027474));
#49890=CARTESIAN_POINT('Ctrl Pts',(6.62199446893495,-4.092980417662,-15.5339374144078));
#49891=CARTESIAN_POINT('Ctrl Pts',(6.59483098593749,-4.07129351351006,-15.5597726972291));
#49892=CARTESIAN_POINT('Ctrl Pts',(6.56684287796802,-4.05125841777049,-15.5849411778566));
#49893=CARTESIAN_POINT('Ctrl Pts',(6.5270962587532,-4.02280607214707,-15.6206835730485));
#49894=CARTESIAN_POINT('Ctrl Pts',(6.48568899948451,-3.99768436133919,-15.6550804830691));
#49895=CARTESIAN_POINT('Ctrl Pts',(6.4431438002412,-3.97592981096522,-15.688016124873));
#49896=CARTESIAN_POINT('Ctrl Pts',(6.41212103682534,-3.96006700431551,-15.7120318691121));
#49897=CARTESIAN_POINT('Ctrl Pts',(6.38049206287102,-3.94599472702329,-15.7352710976102));
#49898=CARTESIAN_POINT('Ctrl Pts',(6.34844350829305,-3.93372675932074,-15.7576954210374));
#49899=CARTESIAN_POINT('Ctrl Pts',(6.32053397916,-3.92304318227627,-15.7772236748456));
#49900=CARTESIAN_POINT('Ctrl Pts',(6.29230613452632,-3.91372773195061,-15.79613405827));
#49901=CARTESIAN_POINT('Ctrl Pts',(6.26389264427641,-3.90575590947883,-15.8144088685689));
#49902=CARTESIAN_POINT('Ctrl Pts',(6.9993386693906,-9.44604681400665,-24.824660272019));
#49903=CARTESIAN_POINT('Ctrl Pts',(6.9993386693906,-9.4152902963795,-24.8024268448143));
#49904=CARTESIAN_POINT('Ctrl Pts',(6.9993386693906,-8.9165030314828,-24.437914914655));
#49905=CARTESIAN_POINT('Ctrl Pts',(6.9993386693906,-8.00787683705666,-23.6489663151524));
#49906=CARTESIAN_POINT('Ctrl Pts',(6.9993386693906,-6.88744313917509,-22.3090627902165));
#49907=CARTESIAN_POINT('Ctrl Pts',(6.9993386693906,-5.99155649181728,-20.8064994919115));
#49908=CARTESIAN_POINT('Ctrl Pts',(6.9993386693906,-5.34582279737036,-19.1801225035148));
#49909=CARTESIAN_POINT('Ctrl Pts',(6.9993386693906,-4.96572780212844,-17.4735522140584));
#49910=CARTESIAN_POINT('Ctrl Pts',(6.9993386693906,-4.8759191278038,-15.9617953190228));
#49911=CARTESIAN_POINT('Ctrl Pts',(6.9993386693906,-4.9383180577078,-15.0338172904337));
#49912=CARTESIAN_POINT('Ctrl Pts',(6.9993386693906,-4.9783443035646,-14.6872933671644));
#49913=CARTESIAN_POINT('Ctrl Pts',(7.01706646970942,-9.16066152666895,-25.2195383971088));
#49914=CARTESIAN_POINT('Ctrl Pts',(7.01706646970942,-9.12853933592334,-25.196317292769));
#49915=CARTESIAN_POINT('Ctrl Pts',(7.01706646970942,-8.60761353833628,-24.815622075188));
#49916=CARTESIAN_POINT('Ctrl Pts',(7.01706646970942,-7.65890581809753,-23.9919035502457));
#49917=CARTESIAN_POINT('Ctrl Pts',(7.01706646970942,-6.48824535535127,-22.5919646079468));
#49918=CARTESIAN_POINT('Ctrl Pts',(7.01706646970942,-5.552742828921,-21.0228679220168));
#49919=CARTESIAN_POINT('Ctrl Pts',(7.01706646970942,-4.87818323848258,-19.3240593792248));
#49920=CARTESIAN_POINT('Ctrl Pts',(7.01706646970942,-4.48117975208743,-17.5413569127717));
#49921=CARTESIAN_POINT('Ctrl Pts',(7.01706646970942,-4.38738464109396,-15.9624909042645));
#49922=CARTESIAN_POINT('Ctrl Pts',(7.01706646970942,-4.4525357174292,-14.9933640194634));
#49923=CARTESIAN_POINT('Ctrl Pts',(7.01706646970942,-4.49435138601102,-14.631371943798));
#49924=CARTESIAN_POINT('Ctrl Pts',(6.72658891709759,-8.93068742279116,-25.5377459115975));
#49925=CARTESIAN_POINT('Ctrl Pts',(6.72658891709759,-8.89746472174831,-25.5137289002038));
#49926=CARTESIAN_POINT('Ctrl Pts',(6.72658891709759,-8.35869886917577,-25.1199925862902));
#49927=CARTESIAN_POINT('Ctrl Pts',(6.72658891709759,-7.37769196117677,-24.2682551591898));
#49928=CARTESIAN_POINT('Ctrl Pts',(6.72658891709759,-6.16655689881398,-22.8199374394217));
#49929=CARTESIAN_POINT('Ctrl Pts',(6.72658891709759,-5.19913042013451,-21.197225669337));
#49930=CARTESIAN_POINT('Ctrl Pts',(6.72658891709759,-4.50134184805847,-19.4400490797251));
#49931=CARTESIAN_POINT('Ctrl Pts',(6.72658891709759,-4.09071286913051,-17.5959964667979));
#49932=CARTESIAN_POINT('Ctrl Pts',(6.72658891709759,-3.9937053388489,-15.963051432781));
#49933=CARTESIAN_POINT('Ctrl Pts',(6.72658891709759,-4.06107419738145,-14.960765265593));
#49934=CARTESIAN_POINT('Ctrl Pts',(6.72658891709759,-4.10433184950327,-14.5863083760655));
#49935=CARTESIAN_POINT('Ctrl Pts',(6.25330944738942,-8.85809586787838,-25.6381884304439));
#49936=CARTESIAN_POINT('Ctrl Pts',(6.25330944738942,-8.82452578966113,-25.6139201901951));
#49937=CARTESIAN_POINT('Ctrl Pts',(6.25330944738942,-8.28012870596488,-25.2160674412389));
#49938=CARTESIAN_POINT('Ctrl Pts',(6.25330944738942,-7.28892652718185,-24.355485819768));
#49939=CARTESIAN_POINT('Ctrl Pts',(6.25330944738942,-6.06501561714329,-22.8918972907141));
#49940=CARTESIAN_POINT('Ctrl Pts',(6.25330944738942,-5.08751231113854,-21.252261865925));
#49941=CARTESIAN_POINT('Ctrl Pts',(6.25330944738942,-4.38239148787448,-19.4766613441969));
#49942=CARTESIAN_POINT('Ctrl Pts',(6.25330944738942,-3.96746160866336,-17.6132434964464));
#49943=CARTESIAN_POINT('Ctrl Pts',(6.25330944738942,-3.86944007503447,-15.9632283641636));
#49944=CARTESIAN_POINT('Ctrl Pts',(6.25330944738942,-3.93750897872531,-14.950475436469));
#49945=CARTESIAN_POINT('Ctrl Pts',(6.25330944738942,-3.98122179438819,-14.5720840160315));
#49946=CARTESIAN_POINT('',(7.,-9.3325097692458,-24.7867247203242));
#49947=CARTESIAN_POINT('Ctrl Pts',(7.00000000000003,-9.3325097625576,-24.7867247293774));
#49948=CARTESIAN_POINT('Ctrl Pts',(7.00000000000003,-9.20047564887516,-24.6891826178643));
#49949=CARTESIAN_POINT('Ctrl Pts',(7.00000000006074,-9.07101759620012,-24.5890285581922));
#49950=CARTESIAN_POINT('Ctrl Pts',(6.99999999867344,-8.94403312611638,-24.4862283763798));
#49951=CARTESIAN_POINT('Ctrl Pts',(6.9999999972833,-8.816787959178,-24.3832171476257));
#49952=CARTESIAN_POINT('Ctrl Pts',(6.99999999422993,-8.69202620501044,-24.2775486102555));
#49953=CARTESIAN_POINT('Ctrl Pts',(6.99999999314803,-8.56967699865244,-24.1691471512216));
#49954=CARTESIAN_POINT('Ctrl Pts',(6.99999999206995,-8.44775837368218,-24.0611271875162));
#49955=CARTESIAN_POINT('Ctrl Pts',(6.99999999472217,-8.32823502604961,-23.9503931844797));
#49956=CARTESIAN_POINT('Ctrl Pts',(6.99999999803541,-8.21107368231993,-23.8368341942939));
#49957=CARTESIAN_POINT('Ctrl Pts',(6.99999999907234,-8.17440657537131,-23.8012944889135));
#49958=CARTESIAN_POINT('Ctrl Pts',(7.00000000000003,-8.13797110754852,-23.7654778407869));
#49959=CARTESIAN_POINT('Ctrl Pts',(7.00000000000003,-8.10176708255221,-23.7293801929953));
#49960=CARTESIAN_POINT('Ctrl Pts',(7.00000000000003,-8.07278510317455,-23.7004833705015));
#49961=CARTESIAN_POINT('Ctrl Pts',(6.99999999938399,-8.0439475664873,-23.671409737078));
#49962=CARTESIAN_POINT('Ctrl Pts',(6.99999999847202,-8.01525905976914,-23.6421620929155));
#49963=CARTESIAN_POINT('Ctrl Pts',(6.9999999941611,-7.87964747362771,-23.5039074442948));
#49964=CARTESIAN_POINT('Ctrl Pts',(6.99999998574664,-7.7473685255244,-23.3617612765062));
#49965=CARTESIAN_POINT('Ctrl Pts',(6.9999999850052,-7.61879186130439,-23.216052524166));
#49966=CARTESIAN_POINT('Ctrl Pts',(6.99999998426218,-7.48994339745887,-23.0700357564906));
#49967=CARTESIAN_POINT('Ctrl Pts',(6.99999998984224,-7.36481318793464,-22.9204416165475));
#49968=CARTESIAN_POINT('Ctrl Pts',(6.99999999473002,-7.24373815942285,-22.767639947986));
#49969=CARTESIAN_POINT('Ctrl Pts',(6.99999999759811,-7.17269293526201,-22.6779779513833));
#49970=CARTESIAN_POINT('Ctrl Pts',(7.00000000000003,-7.10304330304755,-22.5872122518149));
#49971=CARTESIAN_POINT('Ctrl Pts',(7.00000000000003,-7.03485110636723,-22.4954231417833));
#49972=CARTESIAN_POINT('Ctrl Pts',(7.00000000000003,-6.98781951651517,-22.4321169574095));
#49973=CARTESIAN_POINT('Ctrl Pts',(6.99999999890221,-6.9414866272677,-22.3683207500365));
#49974=CARTESIAN_POINT('Ctrl Pts',(6.99999999758213,-6.89585802963811,-22.3040438365628));
#49975=CARTESIAN_POINT('Ctrl Pts',(6.99999999346277,-6.75347250731112,-22.1034656383719));
#49976=CARTESIAN_POINT('Ctrl Pts',(6.99999998925871,-6.61794209682095,-21.898208866214));
#49977=CARTESIAN_POINT('Ctrl Pts',(6.99999999152161,-6.48945127241347,-21.6886107784926));
#49978=CARTESIAN_POINT('Ctrl Pts',(6.99999999354316,-6.37466462383332,-21.5013673535297));
#49979=CARTESIAN_POINT('Ctrl Pts',(7.00000000000003,-6.26549638305752,-21.3106585483591));
#49980=CARTESIAN_POINT('Ctrl Pts',(7.00000000000003,-6.16210765966451,-21.11670577957));
#49981=CARTESIAN_POINT('Ctrl Pts',(7.00000000000003,-6.10679638864214,-21.0129442298772));
#49982=CARTESIAN_POINT('Ctrl Pts',(6.9999999980303,-6.05312424078025,-20.9082598246668));
#49983=CARTESIAN_POINT('Ctrl Pts',(6.99999999636314,-6.00113654312204,-20.8027188607212));
#49984=CARTESIAN_POINT('Ctrl Pts',(6.99999999271528,-5.8873843169222,-20.5717888494901));
#49985=CARTESIAN_POINT('Ctrl Pts',(6.99999999204984,-5.78169965820049,-20.3367563671334));
#49986=CARTESIAN_POINT('Ctrl Pts',(6.99999999506637,-5.6843830048425,-20.0983727638304));
#49987=CARTESIAN_POINT('Ctrl Pts',(6.99999999705719,-5.62015694177595,-19.9410467583477));
#49988=CARTESIAN_POINT('Ctrl Pts',(7.00000000000003,-5.55957473197771,-19.782261714332));
#49989=CARTESIAN_POINT('Ctrl Pts',(7.00000000000003,-5.5027113982491,-19.6222387061761));
#49990=CARTESIAN_POINT('Ctrl Pts',(7.00000000000003,-5.45028577156463,-19.4747041538307));
#49991=CARTESIAN_POINT('Ctrl Pts',(6.99999999722477,-5.40103410796304,-19.3261153637749));
#49992=CARTESIAN_POINT('Ctrl Pts',(6.99999999446467,-5.3549894682949,-19.176560385357));
#49993=CARTESIAN_POINT('Ctrl Pts',(6.99999999008271,-5.28188871907092,-18.939125994485));
#49994=CARTESIAN_POINT('Ctrl Pts',(6.99999998784245,-5.21686862674689,-18.6992564658101));
#49995=CARTESIAN_POINT('Ctrl Pts',(6.99999999262694,-5.160067507945,-18.4573202583932));
#49996=CARTESIAN_POINT('Ctrl Pts',(6.99999999531402,-5.12816673181356,-18.3214434842435));
#49997=CARTESIAN_POINT('Ctrl Pts',(7.00000000000003,-5.09885930665234,-18.1849147103942));
#49998=CARTESIAN_POINT('Ctrl Pts',(7.00000000000003,-5.07217694828604,-18.0477988967269));
#49999=CARTESIAN_POINT('Ctrl Pts',(7.00000000000003,-5.03493020649233,-17.8563946273819));
#50000=CARTESIAN_POINT('Ctrl Pts',(6.99999999014834,-5.00273496135442,-17.6638469339319));
#50001=CARTESIAN_POINT('Ctrl Pts',(6.99999998525275,-4.97570204626941,-17.4706101632764));
#50002=CARTESIAN_POINT('Ctrl Pts',(6.99999998003397,-4.94688448272432,-17.2646163627521));
#50003=CARTESIAN_POINT('Ctrl Pts',(6.99999998145001,-4.92393390756773,-17.0578398871184));
#50004=CARTESIAN_POINT('Ctrl Pts',(6.99999998835933,-4.90684079792026,-16.8508352932017));
#50005=CARTESIAN_POINT('Ctrl Pts',(6.99999999308633,-4.89514657809842,-16.7092134774339));
#50006=CARTESIAN_POINT('Ctrl Pts',(7.00000000000003,-4.88619290480723,-16.5674849963347));
#50007=CARTESIAN_POINT('Ctrl Pts',(7.00000000000003,-4.87996268171837,-16.4258270845899));
#50008=CARTESIAN_POINT('Ctrl Pts',(7.00000000000003,-4.87263517759921,-16.2592200599269));
#50009=CARTESIAN_POINT('Ctrl Pts',(6.99999999283354,-4.86914729178053,-16.0927259175112));
#50010=CARTESIAN_POINT('Ctrl Pts',(6.9999999915726,-4.8694498897709,-15.9262297382788));
#50011=CARTESIAN_POINT('Ctrl Pts',(6.99999999107899,-4.86956834344757,-15.8610538772038));
#50012=CARTESIAN_POINT('Ctrl Pts',(6.99999999110873,-4.87026820069051,-15.7958776284049));
#50013=CARTESIAN_POINT('Ctrl Pts',(6.99999999149977,-4.87154867710779,-15.730693883814));
#50014=CARTESIAN_POINT('Ctrl Pts',(6.99999999249444,-4.87480578700939,-15.5648879251355));
#50015=CARTESIAN_POINT('Ctrl Pts',(6.99999999551013,-4.88181602636915,-15.3990333262998));
#50016=CARTESIAN_POINT('Ctrl Pts',(6.99999999717036,-4.89260120199109,-15.2330487286309));
#50017=CARTESIAN_POINT('Ctrl Pts',(6.9999999986237,-4.9020424443407,-15.0877473568381));
#50018=CARTESIAN_POINT('Ctrl Pts',(6.99999999923216,-4.91437718871111,-14.9423461487223));
#50019=CARTESIAN_POINT('Ctrl Pts',(6.99999999922774,-4.92965270723262,-14.7967937941787));
#50020=CARTESIAN_POINT('',(6.27159471697144,-8.76071062883554,-25.5608579993264));
#50021=CARTESIAN_POINT('Origin',(5.999999877385,-9.33250977407517,-24.7867246592848));
#50022=CARTESIAN_POINT('Ctrl Pts',(6.27159470456775,-8.76071047658199,-25.5608577604381));
#50023=CARTESIAN_POINT('Ctrl Pts',(6.27193966902754,-8.57412214084626,-25.4228903789273));
#50024=CARTESIAN_POINT('Ctrl Pts',(6.2722578257168,-8.39339828136479,-25.280910205322));
#50025=CARTESIAN_POINT('Ctrl Pts',(6.27254917034707,-8.218616766293,-25.1354917691069));
#50026=CARTESIAN_POINT('Ctrl Pts',(6.27284515826574,-8.04104968080664,-24.9877557348695));
#50027=CARTESIAN_POINT('Ctrl Pts',(6.27311347268825,-7.8696158047382,-24.8364709589357));
#50028=CARTESIAN_POINT('Ctrl Pts',(6.27335411005216,-7.70435942652848,-24.6822005640585));
#50029=CARTESIAN_POINT('Ctrl Pts',(6.27354178927092,-7.57547176147274,-24.5618811476563));
#50030=CARTESIAN_POINT('Ctrl Pts',(6.2737126330027,-7.45034099758903,-24.4397448236428));
#50031=CARTESIAN_POINT('Ctrl Pts',(6.27386663991676,-7.32897316278584,-24.3160426977429));
#50032=CARTESIAN_POINT('Ctrl Pts',(6.27406868997597,-7.16974408948665,-24.1537511408067));
#50033=CARTESIAN_POINT('Ctrl Pts',(6.27424176006529,-7.01699206497253,-23.9887664745278));
#50034=CARTESIAN_POINT('Ctrl Pts',(6.27438584793179,-6.87061872077468,-23.8216766723927));
#50035=CARTESIAN_POINT('Ctrl Pts',(6.27447252014277,-6.7825717416733,-23.721168260856));
#50036=CARTESIAN_POINT('Ctrl Pts',(6.27454870572353,-6.69683228994838,-23.6198972266081));
#50037=CARTESIAN_POINT('Ctrl Pts',(6.2746144043227,-6.61337488394086,-23.517983465972));
#50038=CARTESIAN_POINT('Ctrl Pts',(6.27472591337913,-6.47172412252793,-23.3450070641982));
#50039=CARTESIAN_POINT('Ctrl Pts',(6.27480721185364,-6.33664862454043,-23.1701816545098));
#50040=CARTESIAN_POINT('Ctrl Pts',(6.27485829868477,-6.208004962577,-22.9940551660041));
#50041=CARTESIAN_POINT('Ctrl Pts',(6.27487121294748,-6.17548507417922,-22.9495320728125));
#50042=CARTESIAN_POINT('Ctrl Pts',(6.27488219659928,-6.14337608568578,-22.9049256021009));
#50043=CARTESIAN_POINT('Ctrl Pts',(6.27489124963109,-6.11167545340995,-22.8602441341454));
#50044=CARTESIAN_POINT('Ctrl Pts',(6.27492812701298,-5.98254342920341,-22.6782348810993));
#50045=CARTESIAN_POINT('Ctrl Pts',(6.27493296902064,-5.86018864921786,-22.494985184616));
#50046=CARTESIAN_POINT('Ctrl Pts',(6.27490577558772,-5.74438505523325,-22.3110381127273));
#50047=CARTESIAN_POINT('Ctrl Pts',(6.27488257621681,-5.64559022719756,-22.1541084466469));
#50048=CARTESIAN_POINT('Ctrl Pts',(6.27483606080642,-5.55156315842536,-21.9966702876301));
#50049=CARTESIAN_POINT('Ctrl Pts',(6.27476622982249,-5.46215438129282,-21.8390323218734));
#50050=CARTESIAN_POINT('Ctrl Pts',(6.27472435185156,-5.40853551529692,-21.7444960891583));
#50051=CARTESIAN_POINT('Ctrl Pts',(6.27467408861181,-5.35657744174566,-21.6498875004173));
#50052=CARTESIAN_POINT('Ctrl Pts',(6.27461544161658,-5.30624659063555,-21.555268783472));
#50053=CARTESIAN_POINT('Ctrl Pts',(6.27458611811897,-5.28108116508049,-21.5079594249993));
#50054=CARTESIAN_POINT('Ctrl Pts',(6.27455469605052,-5.25632255329401,-21.4606475301866));
#50055=CARTESIAN_POINT('Ctrl Pts',(6.27452117885621,-5.23196644431683,-21.4133405291976));
#50056=CARTESIAN_POINT('Ctrl Pts',(6.27450442025905,-5.21978838982823,-21.3896870287031));
#50057=CARTESIAN_POINT('Ctrl Pts',(6.27448713770267,-5.20771096158906,-21.3660347513678));
#50058=CARTESIAN_POINT('Ctrl Pts',(6.27446933118762,-5.19573361922136,-21.3423846150635));
#50059=CARTESIAN_POINT('Ctrl Pts',(6.27445391935991,-5.18536703504556,-21.321915038321));
#50060=CARTESIAN_POINT('Ctrl Pts',(6.27443872970706,-5.17546074577125,-21.3022173602556));
#50061=CARTESIAN_POINT('Ctrl Pts',(6.27442216598168,-5.16501365823709,-21.2812921859785));
#50062=CARTESIAN_POINT('Ctrl Pts',(6.27441959231268,-5.16339039144624,-21.2780408357447));
#50063=CARTESIAN_POINT('Ctrl Pts',(6.27441698546962,-5.16175415908346,-21.274759804579));
#50064=CARTESIAN_POINT('Ctrl Pts',(6.2744143394645,-5.16010130860683,-21.2714415407458));
#50065=CARTESIAN_POINT('Ctrl Pts',(6.27440279605979,-5.15289061886207,-21.2569653547084));
#50066=CARTESIAN_POINT('Ctrl Pts',(6.27439106278321,-5.14570487770957,-21.2424654747839));
#50067=CARTESIAN_POINT('Ctrl Pts',(6.27437913963575,-5.13854426363549,-21.2279419562949));
#50068=CARTESIAN_POINT('Ctrl Pts',(6.274200106179,-5.03102320057894,-21.0098623152047));
#50069=CARTESIAN_POINT('Ctrl Pts',(6.27397826260158,-4.92916542322791,-20.7864491802973));
#50070=CARTESIAN_POINT('Ctrl Pts',(6.27371361318119,-4.83351359924625,-20.5579654055483));
#50071=CARTESIAN_POINT('Ctrl Pts',(6.27345238572287,-4.73909856963335,-20.3324359649062));
#50072=CARTESIAN_POINT('Ctrl Pts',(6.27314945222804,-4.65073004052687,-20.1019661153687));
#50073=CARTESIAN_POINT('Ctrl Pts',(6.27280481864902,-4.56895448022259,-19.8668529213087));
#50074=CARTESIAN_POINT('Ctrl Pts',(6.2726079764887,-4.52224725570509,-19.7325648198132));
#50075=CARTESIAN_POINT('Ctrl Pts',(6.27239753063306,-4.47769129316522,-19.5967627473317));
#50076=CARTESIAN_POINT('Ctrl Pts',(6.27217348248945,-4.4353920966628,-19.4595087727019));
#50077=CARTESIAN_POINT('Ctrl Pts',(6.27177013518626,-4.35924209353329,-19.2124144668563));
#50078=CARTESIAN_POINT('Ctrl Pts',(6.27132270305512,-4.29040493734449,-18.9606111698754));
#50079=CARTESIAN_POINT('Ctrl Pts',(6.27083119629828,-4.22947047044943,-18.7045320527505));
#50080=CARTESIAN_POINT('Ctrl Pts',(6.27036732545112,-4.17196216077399,-18.4628514749192));
#50081=CARTESIAN_POINT('Ctrl Pts',(6.26986419816364,-4.12149300234368,-18.217362749668));
#50082=CARTESIAN_POINT('Ctrl Pts',(6.26932182446785,-4.07857886873002,-17.9684779797761));
#50083=CARTESIAN_POINT('Ctrl Pts',(6.26905885247513,-4.05777178438981,-17.8478052325467));
#50084=CARTESIAN_POINT('Ctrl Pts',(6.26878665434446,-4.03874105556843,-17.7263348437419));
#50085=CARTESIAN_POINT('Ctrl Pts',(6.26850523144062,-4.02154717103653,-17.6041178806059));
#50086=CARTESIAN_POINT('Ctrl Pts',(6.26791730876932,-3.98562729960334,-17.3487935183506));
#50087=CARTESIAN_POINT('Ctrl Pts',(6.26728912556651,-3.95772395811605,-17.0902075422599));
#50088=CARTESIAN_POINT('Ctrl Pts',(6.26662069656093,-3.93824735949043,-16.8288449332124));
#50089=CARTESIAN_POINT('Ctrl Pts',(6.26595957943061,-3.91898381334836,-16.5703413425198));
#50090=CARTESIAN_POINT('Ctrl Pts',(6.2652590921452,-3.90796367252156,-16.3091214850602));
#50091=CARTESIAN_POINT('Ctrl Pts',(6.26451925231485,-3.90559010632334,-16.0457052708358));
#50092=CARTESIAN_POINT('Ctrl Pts',(6.26430324302721,-3.9048971018072,-15.9687962610009));
#50093=CARTESIAN_POINT('Ctrl Pts',(6.26408387915132,-3.9049412158933,-15.8917003575276));
#50094=CARTESIAN_POINT('Ctrl Pts',(6.26386116118544,-3.90573258304734,-15.8144313372742));
#50095=CARTESIAN_POINT('Ctrl Pts',(6.99999999998951,-10.9278021978185,-24.1259274559598));
#50096=CARTESIAN_POINT('Ctrl Pts',(6.99999999998951,-10.9277942568591,-24.1259309536957));
#50097=CARTESIAN_POINT('Ctrl Pts',(6.99999999998951,-10.6628645501556,-24.2426238189737));
#50098=CARTESIAN_POINT('Ctrl Pts',(6.99999999998951,-10.1334756387631,-24.4687760835904));
#50099=CARTESIAN_POINT('Ctrl Pts',(6.99999999998951,-9.59921869200086,-24.6831198888034));
#50100=CARTESIAN_POINT('Ctrl Pts',(6.99999999998951,-9.33250574064608,-24.7867214499183));
#50101=CARTESIAN_POINT('Ctrl Pts',(7.00000270572097,-11.1660644378211,-24.6668575634647));
#50102=CARTESIAN_POINT('Ctrl Pts',(7.00000270572097,-11.1660563761032,-24.6668611143908));
#50103=CARTESIAN_POINT('Ctrl Pts',(7.00000270572097,-10.8970978743297,-24.7853285323181));
#50104=CARTESIAN_POINT('Ctrl Pts',(7.00000270572097,-10.3596666804285,-25.0149163654536));
#50105=CARTESIAN_POINT('Ctrl Pts',(7.00000270572097,-9.81729343793422,-25.2325164806277));
#50106=CARTESIAN_POINT('Ctrl Pts',(7.00000270572097,-9.5465245747403,-25.3376935135454));
#50107=CARTESIAN_POINT('Ctrl Pts',(6.5796719778295,-11.3336093881581,-25.0472372157099));
#50108=CARTESIAN_POINT('Ctrl Pts',(6.5796719778295,-11.3336012415234,-25.0472408040392));
#50109=CARTESIAN_POINT('Ctrl Pts',(6.5796719778295,-11.0618097089271,-25.1669560795245));
#50110=CARTESIAN_POINT('Ctrl Pts',(6.5796719778295,-10.5187232176262,-25.3989597892034));
#50111=CARTESIAN_POINT('Ctrl Pts',(6.5796719778295,-9.97064263198303,-25.6188497270959));
#50112=CARTESIAN_POINT('Ctrl Pts',(6.5796719778295,-9.69702166956951,-25.7251346247928));
#50113=CARTESIAN_POINT('Ctrl Pts',(5.98852435812706,-11.3308746781034,-25.0410285650881));
#50114=CARTESIAN_POINT('Ctrl Pts',(5.98852435812706,-11.3308665328548,-25.0410321528068));
#50115=CARTESIAN_POINT('Ctrl Pts',(5.98852435812706,-11.0591212416852,-25.1607270604577));
#50116=CARTESIAN_POINT('Ctrl Pts',(5.98852435812706,-10.5161270575496,-25.3926913375982));
#50117=CARTESIAN_POINT('Ctrl Pts',(5.98852435812706,-9.96813962856907,-25.612543900438));
#50118=CARTESIAN_POINT('Ctrl Pts',(5.98852435812706,-9.69456521882714,-25.7188107152953));
#50119=CARTESIAN_POINT('',(6.99999999994032,-10.9277762174568,-24.1259366382796));
#50120=CARTESIAN_POINT('',(5.98852583803798,-11.3308502321837,-25.0410393004596));
#50121=CARTESIAN_POINT('Origin',(5.999999999061,-10.9277802195584,-24.1259421376201));
#50122=CARTESIAN_POINT('',(5.98852581355327,-9.69456736137568,-25.7188095579027));
#50123=CARTESIAN_POINT('Origin',(5.98846856056595,4.75314848987823,11.4751154608873));
#50124=CARTESIAN_POINT('Origin',(6.,-9.33250981979305,-24.7867247762541));
#50125=CARTESIAN_POINT('Origin',(6.99999997874466,4.74964867791879,11.46639970089));
#50126=CARTESIAN_POINT('Origin',(5.999999877385,-9.33250977407517,-24.7867246592848));
#50127=CARTESIAN_POINT('Origin',(5.99999764420532,-9.33250908124357,-24.7867226423044));
#50128=CARTESIAN_POINT('Ctrl Pts',(-6.09443191456128,-9.75587847514191,
-25.6959433244507));
#50129=CARTESIAN_POINT('Ctrl Pts',(-6.05633875294463,-9.74303070101173,
-25.700443119661));
#50130=CARTESIAN_POINT('Ctrl Pts',(-5.71232895595596,-9.62809884345565,
-25.7408006177088));
#50131=CARTESIAN_POINT('Ctrl Pts',(-5.02622191953824,-9.4183974530615,-25.8161825058434));
#50132=CARTESIAN_POINT('Ctrl Pts',(-3.98582966128773,-9.15597820979409,
-25.9131480292542));
#50133=CARTESIAN_POINT('Ctrl Pts',(-2.81226414604675,-8.93052993886067,
-25.9984040994506));
#50134=CARTESIAN_POINT('Ctrl Pts',(-1.52049089180403,-8.77111616050463,
-26.0601535869399));
#50135=CARTESIAN_POINT('Ctrl Pts',(-0.189402768854967,-8.70741653122222,
-26.0857988309911));
#50136=CARTESIAN_POINT('Ctrl Pts',(1.08608586087063,-8.74249055315278,-26.0715618637506));
#50137=CARTESIAN_POINT('Ctrl Pts',(2.24125031195963,-8.85308572724539,-26.0282772201452));
#50138=CARTESIAN_POINT('Ctrl Pts',(3.27297079110899,-9.01439205730505,-25.9665661311678));
#50139=CARTESIAN_POINT('Ctrl Pts',(4.19996253766372,-9.20867731868125,-25.8936091309432));
#50140=CARTESIAN_POINT('Ctrl Pts',(5.05700893778035,-9.42941774767843,-25.812292285677));
#50141=CARTESIAN_POINT('Ctrl Pts',(5.68046392620768,-9.6183284355846,-25.7443188151842));
#50142=CARTESIAN_POINT('Ctrl Pts',(6.02236021791466,-9.73156265908241,-25.7044579013743));
#50143=CARTESIAN_POINT('Ctrl Pts',(6.09429718633961,-9.75582422974853,-25.6959615814221));
#50144=CARTESIAN_POINT('Ctrl Pts',(-6.21850070569984,-9.42753381746598,
-25.836104681144));
#50145=CARTESIAN_POINT('Ctrl Pts',(-6.17967838293833,-9.41439786728843,
-25.8405746553953));
#50146=CARTESIAN_POINT('Ctrl Pts',(-5.82907993570433,-9.29687497796809,
-25.8806344898236));
#50147=CARTESIAN_POINT('Ctrl Pts',(-5.12974930543611,-9.08221820664856,
-25.9549339225927));
#50148=CARTESIAN_POINT('Ctrl Pts',(-4.06875950537382,-8.8130870839257,-26.0494404552579));
#50149=CARTESIAN_POINT('Ctrl Pts',(-2.87124953326329,-8.58145036507263,
-26.1316253526395));
#50150=CARTESIAN_POINT('Ctrl Pts',(-1.55244036708564,-8.41736480859588,
-26.1904032766854));
#50151=CARTESIAN_POINT('Ctrl Pts',(-0.193343137336627,-8.35164772530744,
-26.2143313324476));
#50152=CARTESIAN_POINT('Ctrl Pts',(1.10885789494489,-8.38784887380784,-26.2011016135553));
#50153=CARTESIAN_POINT('Ctrl Pts',(2.28833274099946,-8.5017594106142,-26.1601252018067));
#50154=CARTESIAN_POINT('Ctrl Pts',(3.34139710108736,-8.66764143052762,-26.1009947690095));
#50155=CARTESIAN_POINT('Ctrl Pts',(4.28714687780912,-8.86714807435702,-26.030425005036));
#50156=CARTESIAN_POINT('Ctrl Pts',(5.16111273668051,-9.09348349929248,-25.9510676829607));
#50157=CARTESIAN_POINT('Ctrl Pts',(5.79660262437972,-9.28687614882921,-25.8841068018567));
#50158=CARTESIAN_POINT('Ctrl Pts',(6.14504916278866,-9.40267148435833,-25.8445606466716));
#50159=CARTESIAN_POINT('Ctrl Pts',(6.21836333046621,-9.42747718413902,-25.8361202061885));
#50160=CARTESIAN_POINT('Ctrl Pts',(-6.32914064070096,-9.0707560819202,-25.7774948834612));
#50161=CARTESIAN_POINT('Ctrl Pts',(-6.28961409118642,-9.0574087794442,-25.7819223687199));
#50162=CARTESIAN_POINT('Ctrl Pts',(-5.93266456189295,-8.93800532070565,
-25.8215673303875));
#50163=CARTESIAN_POINT('Ctrl Pts',(-5.22080192937556,-8.72008792140814,
-25.8945057370815));
#50164=CARTESIAN_POINT('Ctrl Pts',(-4.14080030333458,-8.44715465611549,
-25.9860986694478));
#50165=CARTESIAN_POINT('Ctrl Pts',(-2.92180186623126,-8.21250760778291,
-26.0647484312864));
#50166=CARTESIAN_POINT('Ctrl Pts',(-1.57941028084733,-8.04654008989577,
-26.1201796098463));
#50167=CARTESIAN_POINT('Ctrl Pts',(-0.19661544115636,-7.98024992882376,
-26.1422128861359));
#50168=CARTESIAN_POINT('Ctrl Pts',(1.12798876719248,-8.01674575599185,-26.1300915415413));
#50169=CARTESIAN_POINT('Ctrl Pts',(2.32845989603055,-8.13187910606727,-26.0916963854716));
#50170=CARTESIAN_POINT('Ctrl Pts',(3.40038128787747,-8.29980004443677,-26.0355022183721));
#50171=CARTESIAN_POINT('Ctrl Pts',(4.36310376860213,-8.50197197562449,-25.9677006730754));
#50172=CARTESIAN_POINT('Ctrl Pts',(5.25272562824825,-8.73153230032595,-25.8906750740432));
#50173=CARTESIAN_POINT('Ctrl Pts',(5.89960821227025,-8.92785481431609,-25.8249809893108));
#50174=CARTESIAN_POINT('Ctrl Pts',(6.25435575265139,-9.04549377336416,-25.7858681030111));
#50175=CARTESIAN_POINT('Ctrl Pts',(6.32900000292914,-9.0706987506402,-25.777507429552));
#50176=CARTESIAN_POINT('Ctrl Pts',(-6.3948835674422,-8.78685861212201,-25.5363210765471));
#50177=CARTESIAN_POINT('Ctrl Pts',(-6.35487788533204,-8.77343700879775,
-25.5407054494319));
#50178=CARTESIAN_POINT('Ctrl Pts',(-5.99362001528234,-8.65339939708486,
-25.5799359505694));
#50179=CARTESIAN_POINT('Ctrl Pts',(-5.27347945378245,-8.43484642766188,
-25.6516208656583));
#50180=CARTESIAN_POINT('Ctrl Pts',(-4.18145742918569,-8.16210766130676,
-25.7406724567017));
#50181=CARTESIAN_POINT('Ctrl Pts',(-2.94953791498026,-7.92849091848468,
-25.8163265750121));
#50182=CARTESIAN_POINT('Ctrl Pts',(-1.59372603078983,-7.7639722778274,-25.8689859498486));
#50183=CARTESIAN_POINT('Ctrl Pts',(-0.198288364692249,-7.69871949889113,
-25.889484851852));
#50184=CARTESIAN_POINT('Ctrl Pts',(1.13803432083435,-7.73459195431683,-25.8782582937982));
#50185=CARTESIAN_POINT('Ctrl Pts',(2.35021414803826,-7.84850340786168,-25.841984575314));
#50186=CARTESIAN_POINT('Ctrl Pts',(3.43314197030597,-8.01534144112571,-25.7882487521332));
#50187=CARTESIAN_POINT('Ctrl Pts',(4.40622507863034,-8.21685948830795,-25.7228106836747));
#50188=CARTESIAN_POINT('Ctrl Pts',(5.30578804040778,-8.44635294622799,-25.6478272923519));
#50189=CARTESIAN_POINT('Ctrl Pts',(5.9601824771856,-8.64321722847831,-25.5832948261093));
#50190=CARTESIAN_POINT('Ctrl Pts',(6.31919080554775,-8.76145685074049,-25.5446108733089));
#50191=CARTESIAN_POINT('Ctrl Pts',(6.39473997725938,-8.78680247499924,-25.5363312425679));
#50192=CARTESIAN_POINT('',(-5.98852245733357,-9.69456809190394,-25.718809606518));
#50193=CARTESIAN_POINT('Ctrl Pts',(-5.98852261948844,-9.6945676514372,-25.7188097472701));
#50194=CARTESIAN_POINT('Ctrl Pts',(-5.87206434363686,-9.65602090275627,
-25.732349267617));
#50195=CARTESIAN_POINT('Ctrl Pts',(-5.74891036679771,-9.61638755853972,
-25.7463704895299));
#50196=CARTESIAN_POINT('Ctrl Pts',(-5.61905842363419,-9.57605268651985,
-25.7607445054415));
#50197=CARTESIAN_POINT('Ctrl Pts',(-5.51153067647356,-9.5426522012083,-25.7726473350102));
#50198=CARTESIAN_POINT('Ctrl Pts',(-5.39940999121403,-9.50877138149677,
-25.7847917051554));
#50199=CARTESIAN_POINT('Ctrl Pts',(-5.28269811078158,-9.47465117482898,
-25.7970892678802));
#50200=CARTESIAN_POINT('Ctrl Pts',(-5.21045748173724,-9.45353194357617,
-25.8047010351112));
#50201=CARTESIAN_POINT('Ctrl Pts',(-5.13645747597292,-9.43232409335956,
-25.8123701755227));
#50202=CARTESIAN_POINT('Ctrl Pts',(-5.06069821747161,-9.41109583723057,
-25.8200701491049));
#50203=CARTESIAN_POINT('Ctrl Pts',(-5.00135512738415,-9.39446750241339,
-25.8261016261151));
#50204=CARTESIAN_POINT('Ctrl Pts',(-4.940932629606,-9.3778267010815,-25.8321519616997));
#50205=CARTESIAN_POINT('Ctrl Pts',(-4.87943059212148,-9.36120808501283,
-25.8382085024417));
#50206=CARTESIAN_POINT('Ctrl Pts',(-4.80942185399454,-9.34229085254428,
-25.8451027581786));
#50207=CARTESIAN_POINT('Ctrl Pts',(-4.73801437156246,-9.32340262460789,
-25.8520049648563));
#50208=CARTESIAN_POINT('Ctrl Pts',(-4.66520814401506,-9.30459812859164,
-25.8588947595222));
#50209=CARTESIAN_POINT('Ctrl Pts',(-4.62880503024137,-9.29519588058352,
-25.8623396568552));
#50210=CARTESIAN_POINT('Ctrl Pts',(-4.59205223023201,-9.28581456359189,
-25.8657814461128));
#50211=CARTESIAN_POINT('Ctrl Pts',(-4.55494974405073,-9.27646135470819,
-25.8692174200576));
#50212=CARTESIAN_POINT('Ctrl Pts',(-4.53639850096009,-9.27178475026633,
-25.87093540703));
#50213=CARTESIAN_POINT('Ctrl Pts',(-4.51775983632789,-9.26711517272567,
-25.8726519398435));
#50214=CARTESIAN_POINT('Ctrl Pts',(-4.49903375016761,-9.2624535265998,-25.8743666750007));
#50215=CARTESIAN_POINT('Ctrl Pts',(-4.48967070708747,-9.26012270353686,
-25.8752240425794));
#50216=CARTESIAN_POINT('Ctrl Pts',(-4.48028580862534,-9.25779386331942,
-25.8760809607221));
#50217=CARTESIAN_POINT('Ctrl Pts',(-4.47087905478302,-9.25546712013321,
-25.8769373859222));
#50218=CARTESIAN_POINT('Ctrl Pts',(-4.4614723009407,-9.253140376947,-25.8777938111223));
#50219=CARTESIAN_POINT('Ctrl Pts',(-4.45080026163539,-9.25051015999041,
-25.8787622907533));
#50220=CARTESIAN_POINT('Ctrl Pts',(-4.4425932271173,-9.24849329615969,-25.8795051389721));
#50221=CARTESIAN_POINT('Ctrl Pts',(-4.30856578830439,-9.21555629643465,
-25.8916364446181));
#50222=CARTESIAN_POINT('Ctrl Pts',(-4.17021571232035,-9.18297044935259,
-25.9036951620593));
#50223=CARTESIAN_POINT('Ctrl Pts',(-4.02753511601077,-9.15105931833411,
-25.9155534623622));
#50224=CARTESIAN_POINT('Ctrl Pts',(-3.89063485291537,-9.12044098378059,
-25.9269313544744));
#50225=CARTESIAN_POINT('Ctrl Pts',(-3.74974763042379,-9.09044397683782,
-25.9381245168833));
#50226=CARTESIAN_POINT('Ctrl Pts',(-3.60488117560292,-9.06137189871749,
-25.9490157809797));
#50227=CARTESIAN_POINT('Ctrl Pts',(-3.4569563761102,-9.03168606612013,-25.9601369757358));
#50228=CARTESIAN_POINT('Ctrl Pts',(-3.30487851538804,-9.00296562174038,
-25.9709430808878));
#50229=CARTESIAN_POINT('Ctrl Pts',(-3.14864759357098,-8.97555104598866,
-25.9812999739124));
#50230=CARTESIAN_POINT('Ctrl Pts',(-3.07053213266245,-8.9618437581128,-25.9864784204247));
#50231=CARTESIAN_POINT('Ctrl Pts',(-2.99137840636983,-8.94846315819212,
-25.9915444311804));
#50232=CARTESIAN_POINT('Ctrl Pts',(-2.91118641383546,-8.93545291839981,
-25.9964804840002));
#50233=CARTESIAN_POINT('Ctrl Pts',(-2.89492183649935,-8.93281417549574,
-25.9974816165358));
#50234=CARTESIAN_POINT('Ctrl Pts',(-2.8786145518893,-8.93019066405754,-25.9984774035267));
#50235=CARTESIAN_POINT('Ctrl Pts',(-2.86226455462771,-8.92758275918284,
-25.9994676936367));
#50236=CARTESIAN_POINT('Ctrl Pts',(-2.83830797547962,-8.92376156713358,
-26.0009187008157));
#50237=CARTESIAN_POINT('Ctrl Pts',(-2.81425969566226,-8.91997388051614,
-26.0023579069037));
#50238=CARTESIAN_POINT('Ctrl Pts',(-2.79011972518663,-8.91622085219789,
-26.0037848560267));
#50239=CARTESIAN_POINT('Ctrl Pts',(-2.76981216043608,-8.91306364595109,
-26.0049852660165));
#50240=CARTESIAN_POINT('Ctrl Pts',(-2.74943970403522,-8.90993097041398,
-26.0061770006707));
#50241=CARTESIAN_POINT('Ctrl Pts',(-2.72900235599295,-8.90682351895854,
-26.007359785224));
#50242=CARTESIAN_POINT('Ctrl Pts',(-2.71878368197181,-8.90526979323082,
-26.0079511775006));
#50243=CARTESIAN_POINT('Ctrl Pts',(-2.70854878504028,-8.90372237351926,
-26.0085403322403));
#50244=CARTESIAN_POINT('Ctrl Pts',(-2.69829766519956,-8.90218134668462,
-26.0091272149495));
#50245=CARTESIAN_POINT('Ctrl Pts',(-2.68804654535884,-8.90064031984998,
-26.0097140976586));
#50246=CARTESIAN_POINT('Ctrl Pts',(-2.67637482465604,-8.8988969930817,-26.0103782308601));
#50247=CARTESIAN_POINT('Ctrl Pts',(-2.66749563695095,-8.89757753171104,
-26.0108810124235));
#50248=CARTESIAN_POINT('Ctrl Pts',(-2.4817721187646,-8.86997872244956,-26.021397555594));
#50249=CARTESIAN_POINT('Ctrl Pts',(-2.29115211002206,-8.84449825424844,
-26.031158807538));
#50250=CARTESIAN_POINT('Ctrl Pts',(-2.09562977114086,-8.82160895207015,
-26.0399712214066));
#50251=CARTESIAN_POINT('Ctrl Pts',(-1.9920271200296,-8.80948045360125,-26.044640710554));
#50252=CARTESIAN_POINT('Ctrl Pts',(-1.88704839731678,-8.79808016320673,
-26.0490434488219));
#50253=CARTESIAN_POINT('Ctrl Pts',(-1.78069528279165,-8.78748324876857,
-26.0531481972549));
#50254=CARTESIAN_POINT('Ctrl Pts',(-1.69992409241387,-8.77943529081903,
-26.0562655993038));
#50255=CARTESIAN_POINT('Ctrl Pts',(-1.61836026565276,-8.7718494917914,-26.059211532594));
#50256=CARTESIAN_POINT('Ctrl Pts',(-1.53600234381161,-8.76475689540864,
-26.0619727221466));
#50257=CARTESIAN_POINT('Ctrl Pts',(-1.4618110337009,-8.75836760090048,-26.0644601121366));
#50258=CARTESIAN_POINT('Ctrl Pts',(-1.38697529445642,-8.75237857171189,
-26.0667975749014));
#50259=CARTESIAN_POINT('Ctrl Pts',(-1.31149638803829,-8.74681213319418,
-26.0689746055433));
#50260=CARTESIAN_POINT('Ctrl Pts',(-1.23186330964479,-8.74093933169387,
-26.0712714545571));
#50261=CARTESIAN_POINT('Ctrl Pts',(-1.15151359812717,-8.73553695291215,
-26.0733897207682));
#50262=CARTESIAN_POINT('Ctrl Pts',(-1.07044725193411,-8.730630679564,-26.075316971428));
#50263=CARTESIAN_POINT('Ctrl Pts',(-1.02991407883757,-8.72817754288992,
-26.076280596758));
#50264=CARTESIAN_POINT('Ctrl Pts',(-0.98920174707087,-8.72584843119376,
-26.0771964639889));
#50265=CARTESIAN_POINT('Ctrl Pts',(-0.948310256537152,-8.72364651475522,
-26.0780630037134));
#50266=CARTESIAN_POINT('Ctrl Pts',(-0.927864511270293,-8.72254555653596,
-26.0784962735757));
#50267=CARTESIAN_POINT('Ctrl Pts',(-0.907373976312124,-8.72147639704049,
-26.0789172112858));
#50268=CARTESIAN_POINT('Ctrl Pts',(-0.88683865166021,-8.72043942951786,
-26.0793256198315));
#50269=CARTESIAN_POINT('Ctrl Pts',(-0.876570989334252,-8.71992094575655,
-26.0795298241043));
#50270=CARTESIAN_POINT('Ctrl Pts',(-0.866292129584895,-8.71941050998264,
-26.0797308960684));
#50271=CARTESIAN_POINT('Ctrl Pts',(-0.856002072412508,-8.71890817113153,
-26.0799288110538));
#50272=CARTESIAN_POINT('Ctrl Pts',(-0.845712015240121,-8.71840583228042,
-26.0801267260392));
#50273=CARTESIAN_POINT('Ctrl Pts',(-0.833723425538011,-8.71783205476417,
-26.0803528299732));
#50274=CARTESIAN_POINT('Ctrl Pts',(-0.825098308626926,-8.717425494198,-26.080513060353));
#50275=CARTESIAN_POINT('Ctrl Pts',(-0.603312001943076,-8.70697119342208,
-26.0846332252766));
#50276=CARTESIAN_POINT('Ctrl Pts',(-0.379421475271433,-8.70066427031859,
-26.0871466546555));
#50277=CARTESIAN_POINT('Ctrl Pts',(-0.1534220406775,-8.69871630031096,-26.0879154399325));
#50278=CARTESIAN_POINT('Ctrl Pts',(-0.0981746734312987,-8.69824010348069,
-26.0881033756351));
#50279=CARTESIAN_POINT('Ctrl Pts',(-0.0428013132975154,-8.69802458934256,
-26.088186939491));
#50280=CARTESIAN_POINT('Ctrl Pts',(0.0126974846559747,-8.69807140240537,
-26.0881659825254));
#50281=CARTESIAN_POINT('Ctrl Pts',(0.153960862518239,-8.69819055762358,
-26.088112639897));
#50282=CARTESIAN_POINT('Ctrl Pts',(0.29603961296522,-8.7000139697725,-26.0873805428933));
#50283=CARTESIAN_POINT('Ctrl Pts',(0.438933750157111,-8.70358140100969,
-26.0859632058811));
#50284=CARTESIAN_POINT('Ctrl Pts',(0.510380818753056,-8.70536511662828,
-26.085254537375));
#50285=CARTESIAN_POINT('Ctrl Pts',(0.582031733559519,-8.70758483852733,
-26.0843745626165));
#50286=CARTESIAN_POINT('Ctrl Pts',(0.653886494540562,-8.71024420963292,
-26.0833229538545));
#50287=CARTESIAN_POINT('Ctrl Pts',(0.689813875031083,-8.71157389518571,
-26.0827971494734));
#50288=CARTESIAN_POINT('Ctrl Pts',(0.725792217051223,-8.71301349319521,
-26.0822284370765));
#50289=CARTESIAN_POINT('Ctrl Pts',(0.761821520526584,-8.71456341919052,
-26.0816167928097));
#50290=CARTESIAN_POINT('Ctrl Pts',(0.779836172264264,-8.71533838218817,
-26.0813109706763));
#50291=CARTESIAN_POINT('Ctrl Pts',(0.797863564365103,-8.71614092719457,
-26.080994415615));
#50292=CARTESIAN_POINT('Ctrl Pts',(0.81590369681761,-8.71697110131534,-26.0806671265482));
#50293=CARTESIAN_POINT('Ctrl Pts',(0.833943829270117,-8.7178012754361,-26.0803398374813));
#50294=CARTESIAN_POINT('Ctrl Pts',(0.853616708032527,-8.71873848300525,
-26.0799705399663));
#50295=CARTESIAN_POINT('Ctrl Pts',(0.870062315217264,-8.71954455667472,
-26.0796530569462));
#50296=CARTESIAN_POINT('Ctrl Pts',(0.954906881865696,-8.72370317303982,
-26.0780151296288));
#50297=CARTESIAN_POINT('Ctrl Pts',(1.03913119420662,-8.72843365652,-26.0761559642982));
#50298=CARTESIAN_POINT('Ctrl Pts',(1.12272942609343,-8.7337099482048,-26.0740877362734));
#50299=CARTESIAN_POINT('Ctrl Pts',(1.34022986286555,-8.74743746037918,-26.0687067552576));
#50300=CARTESIAN_POINT('Ctrl Pts',(1.55349103100834,-8.76485636048876,-26.0619123572394));
#50301=CARTESIAN_POINT('Ctrl Pts',(1.76251272652862,-8.78549453835477,-26.0539173562375));
#50302=CARTESIAN_POINT('Ctrl Pts',(1.93917900970795,-8.80293803945215,-26.0471599375518));
#50303=CARTESIAN_POINT('Ctrl Pts',(2.11281718314964,-8.82268213996404,-26.0395443778246));
#50304=CARTESIAN_POINT('Ctrl Pts',(2.28343846123769,-8.84446515591452,-26.0311863868139));
#50305=CARTESIAN_POINT('Ctrl Pts',(2.3146215842016,-8.84844626819149,-26.0296588618514));
#50306=CARTESIAN_POINT('Ctrl Pts',(2.34570396261418,-8.85249553939135,-26.0281065081374));
#50307=CARTESIAN_POINT('Ctrl Pts',(2.37668569270351,-8.85661137768177,-26.0265300027406));
#50308=CARTESIAN_POINT('Ctrl Pts',(2.47745093085241,-8.86999776457236,-26.0214025633981));
#50309=CARTESIAN_POINT('Ctrl Pts',(2.57802291569005,-8.8842004818162,-26.015976492447));
#50310=CARTESIAN_POINT('Ctrl Pts',(2.67763152738052,-8.89908328647086,-26.0103066010436));
#50311=CARTESIAN_POINT('Ctrl Pts',(2.77938427561843,-8.9142864526369,-26.0045146617453));
#50312=CARTESIAN_POINT('Ctrl Pts',(2.88013158172736,-8.9301992170122,-25.9984683577212));
#50313=CARTESIAN_POINT('Ctrl Pts',(2.97906278137935,-8.94662576433618,-25.9922440351348));
#50314=CARTESIAN_POINT('Ctrl Pts',(3.01306549452358,-8.95227157858459,-25.990104731698));
#50315=CARTESIAN_POINT('Ctrl Pts',(3.04685376840857,-8.95797766172956,-25.9879445467223));
#50316=CARTESIAN_POINT('Ctrl Pts',(3.08039500479343,-8.96373477115169,-25.9857670260623));
#50317=CARTESIAN_POINT('Ctrl Pts',(3.15894907803007,-8.97721800683175,-25.9806672403705));
#50318=CARTESIAN_POINT('Ctrl Pts',(3.23636199036927,-8.99101552360982,-25.9754593206734));
#50319=CARTESIAN_POINT('Ctrl Pts',(3.31263226361224,-9.00508247212714,-25.9701607458246));
#50320=CARTESIAN_POINT('Ctrl Pts',(3.45643416232766,-9.03160465200025,-25.9601706790353));
#50321=CARTESIAN_POINT('Ctrl Pts',(3.59617380830651,-9.05908323278079,-25.9498590854424));
#50322=CARTESIAN_POINT('Ctrl Pts',(3.73185545191301,-9.0872291360773,-25.9393395658838));
#50323=CARTESIAN_POINT('Ctrl Pts',(3.83567798231805,-9.10876616071162,-25.9312901119548));
#50324=CARTESIAN_POINT('Ctrl Pts',(3.93712340771991,-9.13069417429627,-25.9231187412403));
#50325=CARTESIAN_POINT('Ctrl Pts',(4.03619172746806,-9.15289058487712,-25.9148725074305));
#50326=CARTESIAN_POINT('Ctrl Pts',(4.0609588074051,-9.15843968752233,-25.9128109489781));
#50327=CARTESIAN_POINT('Ctrl Pts',(4.08659006974544,-9.16422980812985,-25.910661321275));
#50328=CARTESIAN_POINT('Ctrl Pts',(4.11454679751779,-9.17061410451057,-25.9082932570447));
#50329=CARTESIAN_POINT('Ctrl Pts',(4.14250352529014,-9.17699840089129,-25.9059251928145));
#50330=CARTESIAN_POINT('Ctrl Pts',(4.17028169065756,-9.18340722888102,-25.90355006307));
#50331=CARTESIAN_POINT('Ctrl Pts',(4.19788129363969,-9.18983788987918,-25.9011688869911));
#50332=CARTESIAN_POINT('Ctrl Pts',(4.20564501959985,-9.19164682494845,-25.9004990658147));
#50333=CARTESIAN_POINT('Ctrl Pts',(4.21339461673097,-9.19345748825839,-25.8998287659398));
#50334=CARTESIAN_POINT('Ctrl Pts',(4.22113008445721,-9.19526982128289,-25.8991580094122));
#50335=CARTESIAN_POINT('Ctrl Pts',(4.26839290987553,-9.2063429693288,-25.8950597635421));
#50336=CARTESIAN_POINT('Ctrl Pts',(4.31512826475942,-9.21747842096176,-25.8909444866922));
#50337=CARTESIAN_POINT('Ctrl Pts',(4.36133616318358,-9.22866296308564,-25.8868173528634));
#50338=CARTESIAN_POINT('Ctrl Pts',(4.51929288752084,-9.26689611580086,-25.8727091903471));
#50339=CARTESIAN_POINT('Ctrl Pts',(4.67108689359218,-9.30569782268728,-25.8584650443958));
#50340=CARTESIAN_POINT('Ctrl Pts',(4.81671592687905,-9.34457708467627,-25.8442720103327));
#50341=CARTESIAN_POINT('Ctrl Pts',(4.86938363922463,-9.35863802939607,-25.8391390047879));
#50342=CARTESIAN_POINT('Ctrl Pts',(4.92124512535988,-9.37270953859383,-25.8340124451188));
#50343=CARTESIAN_POINT('Ctrl Pts',(4.97230066796867,-9.38676979635092,-25.8289003898528));
#50344=CARTESIAN_POINT('Ctrl Pts',(5.00457274340919,-9.39565724864042,-25.8256690730404));
#50345=CARTESIAN_POINT('Ctrl Pts',(5.03652276008337,-9.40453935274694,-25.8224438719359));
#50346=CARTESIAN_POINT('Ctrl Pts',(5.06815068241344,-9.41341134502733,-25.8192265142138));
#50347=CARTESIAN_POINT('Ctrl Pts',(5.21038996184149,-9.45331108222424,-25.8047571905804));
#50348=CARTESIAN_POINT('Ctrl Pts',(5.34611446592922,-9.49300293214208,-25.7904489428062));
#50349=CARTESIAN_POINT('Ctrl Pts',(5.47532374055758,-9.53208408751539,-25.7764525725624));
#50350=CARTESIAN_POINT('Ctrl Pts',(5.60704945441462,-9.57192637518952,-25.7621836134101));
#50351=CARTESIAN_POINT('Ctrl Pts',(5.73200388397534,-9.6111339299822,-25.7482386066609));
#50352=CARTESIAN_POINT('Ctrl Pts',(5.85018857600751,-9.64932450496305,-25.7347472541537));
#50353=CARTESIAN_POINT('Ctrl Pts',(5.86232648746063,-9.65324678803957,-25.7333616530298));
#50354=CARTESIAN_POINT('Ctrl Pts',(5.87439299269056,-9.65715838230777,-25.7319808128288));
#50355=CARTESIAN_POINT('Ctrl Pts',(5.88638809326722,-9.66105889975959,-25.7306048578009));
#50356=CARTESIAN_POINT('Ctrl Pts',(5.92102969266071,-9.67232351251794,-25.726631128481));
#50357=CARTESIAN_POINT('Ctrl Pts',(5.95507574029098,-9.68349572625319,-25.7226981598991));
#50358=CARTESIAN_POINT('Ctrl Pts',(5.98852582161058,-9.69456702968901,-25.7188089328263));
#50359=CARTESIAN_POINT('',(-6.27159361730922,-8.76070973783752,-25.5608563036425));
#50360=CARTESIAN_POINT('Origin',(-5.9999949808,-9.33250914740362,-24.7867195890602));
#50361=CARTESIAN_POINT('Ctrl Pts',(-6.27159386307039,-8.76070927462836,
-25.56085716797));
#50362=CARTESIAN_POINT('Ctrl Pts',(-6.19708064101881,-8.73626652885538,
-25.5689447883498));
#50363=CARTESIAN_POINT('Ctrl Pts',(-6.11543892747885,-8.70997409384621,
-25.5777035213267));
#50364=CARTESIAN_POINT('Ctrl Pts',(-6.02658468999164,-8.68208172222085,
-25.5870520415819));
#50365=CARTESIAN_POINT('Ctrl Pts',(-5.93855992585843,-8.6544497318637,-25.5963132913965));
#50366=CARTESIAN_POINT('Ctrl Pts',(-5.8434565165779,-8.62524745650439,-25.6061534758547));
#50367=CARTESIAN_POINT('Ctrl Pts',(-5.74118378182371,-8.59476439466987,
-25.6164754166227));
#50368=CARTESIAN_POINT('Ctrl Pts',(-5.6404952869802,-8.56475352596948,-25.6266374669707));
#50369=CARTESIAN_POINT('Ctrl Pts',(-5.53285768868566,-8.5335011967807,-25.6372665625407));
#50370=CARTESIAN_POINT('Ctrl Pts',(-5.41817810268241,-8.50132997649802,
-25.6482508431793));
#50371=CARTESIAN_POINT('Ctrl Pts',(-5.37925207454577,-8.49041000486612,
-25.6519792697642));
#50372=CARTESIAN_POINT('Ctrl Pts',(-5.33951466255555,-8.4793845652548,-25.6557484475657));
#50373=CARTESIAN_POINT('Ctrl Pts',(-5.29896211848324,-8.46826753089785,
-25.6595534564569));
#50374=CARTESIAN_POINT('Ctrl Pts',(-5.21821342920711,-8.44613116501754,
-25.6671300336527));
#50375=CARTESIAN_POINT('Ctrl Pts',(-5.13423280764027,-8.42363090369957,
-25.6748488992373));
#50376=CARTESIAN_POINT('Ctrl Pts',(-5.04699090796374,-8.40088618384965,
-25.6826701541321));
#50377=CARTESIAN_POINT('Ctrl Pts',(-4.92201132303848,-8.36830292217578,
-25.6938746005504));
#50378=CARTESIAN_POINT('Ctrl Pts',(-4.79033868981777,-8.33521570366159,
-25.7052899395705));
#50379=CARTESIAN_POINT('Ctrl Pts',(-4.6518870917885,-8.30201778587879,-25.7167847294538));
#50380=CARTESIAN_POINT('Ctrl Pts',(-4.51343549375923,-8.268819868096,-25.728279519337));
#50381=CARTESIAN_POINT('Ctrl Pts',(-4.36820473336794,-8.23551097951922,
-25.7398538586143));
#50382=CARTESIAN_POINT('Ctrl Pts',(-4.21611190204717,-8.20253752415175,
-25.7513583798219));
#50383=CARTESIAN_POINT('Ctrl Pts',(-4.07082877172975,-8.17104039985229,
-25.7623478054201));
#50384=CARTESIAN_POINT('Ctrl Pts',(-3.91928373419016,-8.13984958966014,
-25.7732733247265));
#50385=CARTESIAN_POINT('Ctrl Pts',(-3.76142160008198,-8.10939970549724,
-25.7839928332117));
#50386=CARTESIAN_POINT('Ctrl Pts',(-3.73054732381349,-8.10344439429294,
-25.786089327525));
#50387=CARTESIAN_POINT('Ctrl Pts',(-3.69943145109153,-8.09751757244847,
-25.7881778959314));
#50388=CARTESIAN_POINT('Ctrl Pts',(-3.66807362440159,-8.09162271074323,
-25.7902574076099));
#50389=CARTESIAN_POINT('Ctrl Pts',(-3.58017497740066,-8.07509891356584,
-25.7960864551638));
#50390=CARTESIAN_POINT('Ctrl Pts',(-3.49037513070284,-8.05882589735015,
-25.8018444457918));
#50391=CARTESIAN_POINT('Ctrl Pts',(-3.39866711056178,-8.04288325223482,
-25.8075055234358));
#50392=CARTESIAN_POINT('Ctrl Pts',(-3.35281310049126,-8.03491192967715,
-25.8103360622577));
#50393=CARTESIAN_POINT('Ctrl Pts',(-3.30648203810739,-8.02702323593776,
-25.8131423273727));
#50394=CARTESIAN_POINT('Ctrl Pts',(-3.25967322192836,-8.01922760746874,
-25.8159209778804));
#50395=CARTESIAN_POINT('Ctrl Pts',(-3.23626881383885,-8.01532979323423,
-25.8173103031342));
#50396=CARTESIAN_POINT('Ctrl Pts',(-3.2127449667047,-8.01145524761749,-25.8186927218278));
#50397=CARTESIAN_POINT('Ctrl Pts',(-3.18910159680807,-8.00760529720807,
-25.8200678036269));
#50398=CARTESIAN_POINT('Ctrl Pts',(-3.17727991185975,-8.00568032200336,
-25.8207553445264));
#50399=CARTESIAN_POINT('Ctrl Pts',(-3.16542834618611,-8.00376149574843,
-25.8214410510163));
#50400=CARTESIAN_POINT('Ctrl Pts',(-3.153546889955,-8.00184898612967,-25.822124868798));
#50401=CARTESIAN_POINT('Ctrl Pts',(-3.1416654337239,-7.99993647651091,-25.8228086865797));
#50402=CARTESIAN_POINT('Ctrl Pts',(-3.12814004446228,-7.99777350884686,
-25.8235825260523));
#50403=CARTESIAN_POINT('Ctrl Pts',(-3.11781283988124,-7.99613057576302,
-25.8241706011561));
#50404=CARTESIAN_POINT('Ctrl Pts',(-3.07662101472709,-7.98957745562305,
-25.8265162394809));
#50405=CARTESIAN_POINT('Ctrl Pts',(-3.03568844271409,-7.98319675839628,
-25.8288016648055));
#50406=CARTESIAN_POINT('Ctrl Pts',(-2.99501685898111,-7.97698388940999,
-25.8310284388352));
#50407=CARTESIAN_POINT('Ctrl Pts',(-2.79740091933288,-7.94679667194882,
-25.8418479349523));
#50408=CARTESIAN_POINT('Ctrl Pts',(-2.60595036248865,-7.92057001971489,
-25.8512835464356));
#50409=CARTESIAN_POINT('Ctrl Pts',(-2.42085823916677,-7.89776613030724,
-25.8595190543067));
#50410=CARTESIAN_POINT('Ctrl Pts',(-2.23093018845681,-7.87436644054158,
-25.8679697324258));
#50411=CARTESIAN_POINT('Ctrl Pts',(-2.04769685011509,-7.85457034414563,
-25.8751568615175));
#50412=CARTESIAN_POINT('Ctrl Pts',(-1.87131799226574,-7.83781990485744,
-25.8812683924748));
#50413=CARTESIAN_POINT('Ctrl Pts',(-1.78117118814471,-7.82925879618565,
-25.8843919810433));
#50414=CARTESIAN_POINT('Ctrl Pts',(-1.69281417152675,-7.82149367808869,
-25.8872344244849));
#50415=CARTESIAN_POINT('Ctrl Pts',(-1.60626396048369,-7.81445276530423,
-25.8898196774583));
#50416=CARTESIAN_POINT('Ctrl Pts',(-1.43907018611961,-7.80085144915243,
-25.8948137519626));
#50417=CARTESIAN_POINT('Ctrl Pts',(-1.27862092923838,-7.78995013294518,
-25.8988490903609));
#50418=CARTESIAN_POINT('Ctrl Pts',(-1.12501574825844,-7.78123955773252,
-25.9020960152113));
#50419=CARTESIAN_POINT('Ctrl Pts',(-0.969938844053647,-7.7724455246849,
-25.9053740495248));
#50420=CARTESIAN_POINT('Ctrl Pts',(-0.821837400097612,-7.76588424261616,
-25.9078485020547));
#50421=CARTESIAN_POINT('Ctrl Pts',(-0.680781487683452,-7.76107119712844,
-25.9096791178162));
#50422=CARTESIAN_POINT('Ctrl Pts',(-0.538387209027835,-7.75621248451844,
-25.9115271028202));
#50423=CARTESIAN_POINT('Ctrl Pts',(-0.403172411170193,-7.75313516554023,
-25.9127189940968));
#50424=CARTESIAN_POINT('Ctrl Pts',(-0.275182242969547,-7.75138351950705,
-25.9134031520801));
#50425=CARTESIAN_POINT('Ctrl Pts',(-0.236222356389467,-7.75085032284248,
-25.9136114080564));
#50426=CARTESIAN_POINT('Ctrl Pts',(-0.197931723059676,-7.75044026708882,
-25.9137725064282));
#50427=CARTESIAN_POINT('Ctrl Pts',(-0.160311209414855,-7.75014131167927,
-25.9138903374117));
#50428=CARTESIAN_POINT('Ctrl Pts',(-0.153998804667823,-7.75009114948414,
-25.9139101084564));
#50429=CARTESIAN_POINT('Ctrl Pts',(-0.147705266086702,-7.75004411608126,
-25.9139286610374));
#50430=CARTESIAN_POINT('Ctrl Pts',(-0.141430596982659,-7.75000015410289,
-25.9139460130055));
#50431=CARTESIAN_POINT('Ctrl Pts',(-0.103047862356985,-7.74973123459157,
-25.9140521566089));
#50432=CARTESIAN_POINT('Ctrl Pts',(-0.0662557655660949,-7.7495797024787,
-25.9141126178867));
#50433=CARTESIAN_POINT('Ctrl Pts',(-0.0289811603192746,-7.74952611417544,
-25.9141334371331));
#50434=CARTESIAN_POINT('Ctrl Pts',(-0.0185590840463095,-7.7495111307469,
-25.9141392582484));
#50435=CARTESIAN_POINT('Ctrl Pts',(-0.00809928513411629,-7.74950410145234,
-25.9141418862787));
#50436=CARTESIAN_POINT('Ctrl Pts',(0.00244355322760035,-7.74950529241563,
-25.9141412344764));
#50437=CARTESIAN_POINT('Ctrl Pts',(0.127127957617791,-7.74951937728952,
-25.9141335259665));
#50438=CARTESIAN_POINT('Ctrl Pts',(0.258986367500759,-7.75068425897285,
-25.9136690002192));
#50439=CARTESIAN_POINT('Ctrl Pts',(0.397985564384329,-7.75344426614272,
-25.9126040413307));
#50440=CARTESIAN_POINT('Ctrl Pts',(0.535666614760285,-7.7561780998246,-25.9115491815786));
#50441=CARTESIAN_POINT('Ctrl Pts',(0.680353984971248,-7.76047708718023,
-25.9099052014884));
#50442=CARTESIAN_POINT('Ctrl Pts',(0.831993438911318,-7.76681627477429,
-25.907517222457));
#50443=CARTESIAN_POINT('Ctrl Pts',(0.942266724269816,-7.7714261769095,-25.9057806671851));
#50444=CARTESIAN_POINT('Ctrl Pts',(1.05621605154075,-7.77711589621786,-25.9036503474668));
#50445=CARTESIAN_POINT('Ctrl Pts',(1.17381162281563,-7.78408209266922,-25.9010616180959));
#50446=CARTESIAN_POINT('Ctrl Pts',(1.33437225434298,-7.79359347893528,-25.8975270630261));
#50447=CARTESIAN_POINT('Ctrl Pts',(1.50173206401884,-7.80548373360795,-25.8931383077185));
#50448=CARTESIAN_POINT('Ctrl Pts',(1.67578004007753,-7.82026797246305,-25.8877236195892));
#50449=CARTESIAN_POINT('Ctrl Pts',(1.84378667050358,-7.83453903846281,-25.8824968796522));
#50450=CARTESIAN_POINT('Ctrl Pts',(2.01802545152726,-7.85150699806721,-25.8763141118331));
#50451=CARTESIAN_POINT('Ctrl Pts',(2.1983598498116,-7.87166084096275,-25.8690099460407));
#50452=CARTESIAN_POINT('Ctrl Pts',(2.26108424604589,-7.87867080489336,-25.8664693914173));
#50453=CARTESIAN_POINT('Ctrl Pts',(2.32454574387929,-7.88606641066583,-25.8637930754091));
#50454=CARTESIAN_POINT('Ctrl Pts',(2.38873742215535,-7.8938688900564,-25.860973738592));
#50455=CARTESIAN_POINT('Ctrl Pts',(2.47500004738477,-7.90435408648068,-25.8571850326134));
#50456=CARTESIAN_POINT('Ctrl Pts',(2.56258134375727,-7.91557403890685,-25.8531380530837));
#50457=CARTESIAN_POINT('Ctrl Pts',(2.65146464458645,-7.92757931330867,-25.8488156636023));
#50458=CARTESIAN_POINT('Ctrl Pts',(2.72897721207415,-7.93804876745358,-25.8450462321875));
#50459=CARTESIAN_POINT('Ctrl Pts',(2.80747997437277,-7.94911552377676,-25.8410673744993));
#50460=CARTESIAN_POINT('Ctrl Pts',(2.88696064306362,-7.96081345283505,-25.8368674928884));
#50461=CARTESIAN_POINT('Ctrl Pts',(2.92670097740905,-7.9666624173642,-25.8347675520829));
#50462=CARTESIAN_POINT('Ctrl Pts',(2.96668578716397,-7.97266917986723,-25.8326123492592));
#50463=CARTESIAN_POINT('Ctrl Pts',(3.00691341526369,-7.97883801602081,-25.8304004296764));
#50464=CARTESIAN_POINT('Ctrl Pts',(3.02702722931355,-7.9819224340976,-25.829294469885));
#50465=CARTESIAN_POINT('Ctrl Pts',(3.04720174789494,-7.98504737087738,-25.8281743305421));
#50466=CARTESIAN_POINT('Ctrl Pts',(3.06743675928565,-7.98821336188863,-25.8270398278529));
#50467=CARTESIAN_POINT('Ctrl Pts',(3.07755426498101,-7.98979635739425,-25.8264725765082));
#50468=CARTESIAN_POINT('Ctrl Pts',(3.08768689387456,-7.99138961647581,-25.8259017343043));
#50469=CARTESIAN_POINT('Ctrl Pts',(3.09783461902328,-7.99299320618079,-25.8253272782121));
#50470=CARTESIAN_POINT('Ctrl Pts',(3.10798234417199,-7.99459679588577,-25.82475282212));
#50471=CARTESIAN_POINT('Ctrl Pts',(3.1164924327771,-7.99594695194843,-25.8242692123921));
#50472=CARTESIAN_POINT('Ctrl Pts',(3.12832305613581,-7.99783503428302,-25.8235930451759));
#50473=CARTESIAN_POINT('Ctrl Pts',(3.24396819272957,-8.01629116570257,-25.8169834652994));
#50474=CARTESIAN_POINT('Ctrl Pts',(3.35682173877642,-8.03535443277902,-25.8101924262962));
#50475=CARTESIAN_POINT('Ctrl Pts',(3.46689179392627,-8.05487866527595,-25.803267018375));
#50476=CARTESIAN_POINT('Ctrl Pts',(3.63912997498682,-8.08543028340038,-25.7924301049036));
#50477=CARTESIAN_POINT('Ctrl Pts',(3.80455199674186,-8.11710766108124,-25.7812651359542));
#50478=CARTESIAN_POINT('Ctrl Pts',(3.96321409892716,-8.14939039424876,-25.7699423194765));
#50479=CARTESIAN_POINT('Ctrl Pts',(4.12187620111246,-8.18167312741628,-25.7586195029989));
#50480=CARTESIAN_POINT('Ctrl Pts',(4.27377865492778,-8.21456150445218,-25.7471387505097));
#50481=CARTESIAN_POINT('Ctrl Pts',(4.41898996524078,-8.24759193080513,-25.7356524370349));
#50482=CARTESIAN_POINT('Ctrl Pts',(4.56351962868667,-8.28046730665551,-25.7242200422913));
#50483=CARTESIAN_POINT('Ctrl Pts',(4.70142133262044,-8.31348366819116,-25.7127822039499));
#50484=CARTESIAN_POINT('Ctrl Pts',(4.83277589947591,-8.34623514225956,-25.7014757980672));
#50485=CARTESIAN_POINT('Ctrl Pts',(4.90532428829938,-8.36432409593767,-25.6952311615098));
#50486=CARTESIAN_POINT('Ctrl Pts',(4.97587556693888,-8.38233314402035,-25.6890263039231));
#50487=CARTESIAN_POINT('Ctrl Pts',(5.04444365587221,-8.40020029078686,-25.6828820636048));
#50488=CARTESIAN_POINT('Ctrl Pts',(5.1353885124747,-8.42389826933422,-25.6747326888246));
#50489=CARTESIAN_POINT('Ctrl Pts',(5.22284458645003,-8.44734616967657,-25.6666901042532));
#50490=CARTESIAN_POINT('Ctrl Pts',(5.30684444827134,-8.47041101632681,-25.6587988967422));
#50491=CARTESIAN_POINT('Ctrl Pts',(5.42689921939801,-8.50337589062097,-25.6475205792412));
#50492=CARTESIAN_POINT('Ctrl Pts',(5.53989448481551,-8.53555643652212,-25.6365523846394));
#50493=CARTESIAN_POINT('Ctrl Pts',(5.6459272916651,-8.56661204936056,-25.626011907698));
#50494=CARTESIAN_POINT('Ctrl Pts',(5.75378657216675,-8.59820261227985,-25.6152898652205));
#50495=CARTESIAN_POINT('Ctrl Pts',(5.85444161366389,-8.62862920659797,-25.6050103186927));
#50496=CARTESIAN_POINT('Ctrl Pts',(5.94798721656892,-8.65758340246176,-25.5952771356166));
#50497=CARTESIAN_POINT('Ctrl Pts',(6.02496432786757,-8.6814093257372,-25.5872678621321));
#50498=CARTESIAN_POINT('Ctrl Pts',(6.09712726844943,-8.70423919491187,-25.5796281564338));
#50499=CARTESIAN_POINT('Ctrl Pts',(6.16452420707897,-8.72592546147543,-25.5724066590223));
#50500=CARTESIAN_POINT('Ctrl Pts',(6.20165893268432,-8.73787427657916,-25.5684277197665));
#50501=CARTESIAN_POINT('Ctrl Pts',(6.23734668826649,-8.74947631976018,-25.5645756231204));
#50502=CARTESIAN_POINT('Ctrl Pts',(6.27159479316261,-8.76071029005264,-25.5608580129605));
#50503=CARTESIAN_POINT('Ctrl Pts',(-6.390311350308,-8.98426072265847,-25.6807376024135));
#50504=CARTESIAN_POINT('Ctrl Pts',(-4.260207566872,-8.27687337786428,-25.9287995262545));
#50505=CARTESIAN_POINT('Ctrl Pts',(0.0001663377215664,-7.56887498315389,
-26.1774674747135));
#50506=CARTESIAN_POINT('Ctrl Pts',(4.260540242315,-8.27692866476545,-25.9287801080206));
#50507=CARTESIAN_POINT('Ctrl Pts',(6.390810363473,-8.9844264466778,-25.6806794874087));
#50508=CARTESIAN_POINT('Ctrl Pts',(-6.390311350308,-8.18394893381911,-25.1149841535959));
#50509=CARTESIAN_POINT('Ctrl Pts',(-4.260207566872,-7.53598966689574,-25.3660582042809));
#50510=CARTESIAN_POINT('Ctrl Pts',(0.0001663377215664,-6.8861563415995,
-25.6190371135297));
#50511=CARTESIAN_POINT('Ctrl Pts',(4.260540242315,-7.53604041174194,-25.3660384494022));
#50512=CARTESIAN_POINT('Ctrl Pts',(6.390810363473,-8.18410073524863,-25.1149253329315));
#50513=CARTESIAN_POINT('Ctrl Pts',(-6.390311350308,-6.63374493681489,-23.7052293667987));
#50514=CARTESIAN_POINT('Ctrl Pts',(-4.260207566872,-6.09525955626641,-23.9981328630517));
#50515=CARTESIAN_POINT('Ctrl Pts',(0.0001663377215663,-5.5578203229384,
-24.2900566685128));
#50516=CARTESIAN_POINT('Ctrl Pts',(4.260540242315,-6.09530152436809,-23.998110067003));
#50517=CARTESIAN_POINT('Ctrl Pts',(6.390810363473,-6.63387109113548,-23.7051607464652));
#50518=CARTESIAN_POINT('Ctrl Pts',(-6.390311350308,-4.89945807532427,-21.0044950488243));
#50519=CARTESIAN_POINT('Ctrl Pts',(-4.260207566872,-4.44478852897079,-21.4424839271908));
#50520=CARTESIAN_POINT('Ctrl Pts',(0.0001663377215666,-3.98943207393405,
-21.8807691943046));
#50521=CARTESIAN_POINT('Ctrl Pts',(4.260540242315,-4.44482408731423,-21.4424497019158));
#50522=CARTESIAN_POINT('Ctrl Pts',(6.390810363473,-4.89956459357196,-21.0043924384536));
#50523=CARTESIAN_POINT('Ctrl Pts',(-6.390311350308,-4.02649527288926,-18.1257216335683));
#50524=CARTESIAN_POINT('Ctrl Pts',(-4.260207566872,-3.53810367046438,-18.7393778278849));
#50525=CARTESIAN_POINT('Ctrl Pts',(0.0001663377215658,-3.05102410498822,
-19.3530139783685));
#50526=CARTESIAN_POINT('Ctrl Pts',(4.260540242315,-3.5381417060386,-18.7393299096397));
#50527=CARTESIAN_POINT('Ctrl Pts',(6.390810363473,-4.02660969144102,-18.1255778685305));
#50528=CARTESIAN_POINT('Ctrl Pts',(-6.390311350308,-3.91822475000029,-16.2401092417364));
#50529=CARTESIAN_POINT('Ctrl Pts',(-4.260207566872,-3.34432375800902,-16.9588839722607));
#50530=CARTESIAN_POINT('Ctrl Pts',(0.0001663377215673,-2.76847329023801,
-17.67766846846));
#50531=CARTESIAN_POINT('Ctrl Pts',(4.260540242315,-3.34436872560761,-16.9588278430867));
#50532=CARTESIAN_POINT('Ctrl Pts',(6.390810363473,-3.91835920133192,-16.2399408499196));
#50533=CARTESIAN_POINT('Ctrl Pts',(-6.390311350308,-3.94962504311709,-15.4599592241865));
#50534=CARTESIAN_POINT('Ctrl Pts',(-4.260207566872,-3.32898404753985,-16.2180683920147));
#50535=CARTESIAN_POINT('Ctrl Pts',(0.0001663377215673,-2.70679083262895,
-16.9761985551425));
#50536=CARTESIAN_POINT('Ctrl Pts',(4.260540242315,-3.32903263399909,-16.2180091903709));
#50537=CARTESIAN_POINT('Ctrl Pts',(6.390810363473,-3.94977044452508,-15.4597816172428));
#50538=CARTESIAN_POINT('',(-6.26386060052019,-3.90573752923273,-15.8144217504595));
#50539=CARTESIAN_POINT('Ctrl Pts',(-6.2715955238423,-8.76070944182667,-25.5608567088109));
#50540=CARTESIAN_POINT('Ctrl Pts',(-6.27195777356125,-8.56459408488497,
-25.4158727806631));
#50541=CARTESIAN_POINT('Ctrl Pts',(-6.27229031321318,-8.37478238328197,
-25.2662940479724));
#50542=CARTESIAN_POINT('Ctrl Pts',(-6.27259314304416,-8.1913537279175,-25.112746927186));
#50543=CARTESIAN_POINT('Ctrl Pts',(-6.2728986357117,-8.00631215176943,-24.957849639263));
#50544=CARTESIAN_POINT('Ctrl Pts',(-6.27317389377364,-7.82776629043592,
-24.7989138205072));
#50545=CARTESIAN_POINT('Ctrl Pts',(-6.27341891748261,-7.65576238405222,
-24.6365421341386));
#50546=CARTESIAN_POINT('Ctrl Pts',(-6.27366754263728,-7.48123030302019,
-24.4717838509204));
#50547=CARTESIAN_POINT('Ctrl Pts',(-6.27388503811653,-7.31343384998446,
-24.3034879431072));
#50548=CARTESIAN_POINT('Ctrl Pts',(-6.27407140418428,-7.15238613772221,
-24.1322429852995));
#50549=CARTESIAN_POINT('Ctrl Pts',(-6.27421804474197,-7.02566711303238,
-23.9975003445527));
#50550=CARTESIAN_POINT('Ctrl Pts',(-6.27434541247218,-6.90312564630339,
-23.8609310582105));
#50551=CARTESIAN_POINT('Ctrl Pts',(-6.27445350750348,-6.78475354197435,
-23.7228045339384));
#50552=CARTESIAN_POINT('Ctrl Pts',(-6.27450262984591,-6.730960921048,-23.6600347808604));
#50553=CARTESIAN_POINT('Ctrl Pts',(-6.27454777213208,-6.67802913997596,
-23.5969432473287));
#50554=CARTESIAN_POINT('Ctrl Pts',(-6.27458893437407,-6.6259526392861,-23.5335576726619));
#50555=CARTESIAN_POINT('Ctrl Pts',(-6.27470712617076,-6.47642202861682,
-23.3515545894672));
#50556=CARTESIAN_POINT('Ctrl Pts',(-6.27479250318269,-6.33394454999158,
-23.1671310164002));
#50557=CARTESIAN_POINT('Ctrl Pts',(-6.27484506540985,-6.19837392969763,
-22.9809083500403));
#50558=CARTESIAN_POINT('Ctrl Pts',(-6.27489762763701,-6.06280330940369,
-22.7946856836805));
#50559=CARTESIAN_POINT('Ctrl Pts',(-6.27491737507941,-5.93413944051589,
-22.6066637620607));
#50560=CARTESIAN_POINT('Ctrl Pts',(-6.27490430773705,-5.81221558908333,
-22.4174135733054));
#50561=CARTESIAN_POINT('Ctrl Pts',(-6.2748947676246,-5.72320229014943,-22.2792471405111));
#50562=CARTESIAN_POINT('Ctrl Pts',(-6.27486753869774,-5.63762494416323,
-22.1401745615071));
#50563=CARTESIAN_POINT('Ctrl Pts',(-6.27482283814201,-5.55559566787712,
-22.000668726424));
#50564=CARTESIAN_POINT('Ctrl Pts',(-6.2747779206947,-5.47316837729791,-21.8604859950076));
#50565=CARTESIAN_POINT('Ctrl Pts',(-6.274715361659,-5.39432374986302,-21.7198661346417));
#50566=CARTESIAN_POINT('Ctrl Pts',(-6.27463538139726,-5.31912446741838,
-21.5793022040088));
#50567=CARTESIAN_POINT('Ctrl Pts',(-6.2745769115678,-5.2641497883714,-21.4765424871483));
#50568=CARTESIAN_POINT('Ctrl Pts',(-6.27450913115853,-5.21112225376327,
-21.3738129550114));
#50569=CARTESIAN_POINT('Ctrl Pts',(-6.27443212626573,-5.16004897315625,
-21.2713091205343));
#50570=CARTESIAN_POINT('Ctrl Pts',(-6.27435635457874,-5.10979361287016,
-21.1704468483025));
#50571=CARTESIAN_POINT('Ctrl Pts',(-6.27427024744633,-5.06062330858267,
-21.0681861027421));
#50572=CARTESIAN_POINT('Ctrl Pts',(-6.27417380486852,-5.01262251506725,
-20.9645377933814));
#50573=CARTESIAN_POINT('Ctrl Pts',(-6.27399075524317,-4.92151620632652,
-20.7678115690527));
#50574=CARTESIAN_POINT('Ctrl Pts',(-6.27377047251187,-4.83462177577421,
-20.5660838688701));
#50575=CARTESIAN_POINT('Ctrl Pts',(-6.27351295667464,-4.75246065776447,
-20.3594970111178));
#50576=CARTESIAN_POINT('Ctrl Pts',(-6.27325823298668,-4.67119038245961,
-20.1551500984832));
#50577=CARTESIAN_POINT('Ctrl Pts',(-6.27296707922523,-4.59455132156058,
-19.9460487147278));
#50578=CARTESIAN_POINT('Ctrl Pts',(-6.2726394953903,-4.52307273725537,-19.7323747704891));
#50579=CARTESIAN_POINT('Ctrl Pts',(-6.27231699872677,-4.45270417051253,
-19.5220190485268));
#50580=CARTESIAN_POINT('Ctrl Pts',(-6.2719591946766,-4.38733705627334,-19.3072316127526));
#50581=CARTESIAN_POINT('Ctrl Pts',(-6.27156608323978,-4.32750034373043,
-19.0882303678766));
#50582=CARTESIAN_POINT('Ctrl Pts',(-6.27136275171617,-4.29655062110826,
-18.974954963952));
#50583=CARTESIAN_POINT('Ctrl Pts',(-6.27114997428599,-4.2670808590318,-18.8605529604809));
#50584=CARTESIAN_POINT('Ctrl Pts',(-6.27092775094925,-4.23916681989789,
-18.7450593753188));
#50585=CARTESIAN_POINT('Ctrl Pts',(-6.27050608281783,-4.18620001229596,
-18.5259106353175));
#50586=CARTESIAN_POINT('Ctrl Pts',(-6.27005040532724,-4.13883315746638,
-18.3028288891132));
#50587=CARTESIAN_POINT('Ctrl Pts',(-6.2695607180599,-4.09760163845932,-18.0760877681166));
#50588=CARTESIAN_POINT('Ctrl Pts',(-6.26938505158857,-4.08281057498897,
-17.9947484822313));
#50589=CARTESIAN_POINT('Ctrl Pts',(-6.26920500844612,-4.06880927968371,
-17.9129387064842));
#50590=CARTESIAN_POINT('Ctrl Pts',(-6.26902058861328,-4.05562321450361,
-17.8306725395332));
#50591=CARTESIAN_POINT('Ctrl Pts',(-6.26850854126086,-4.01901169794123,
-17.602257990332));
#50592=CARTESIAN_POINT('Ctrl Pts',(-6.26796275346181,-3.98868443460602,
-17.3703213570019));
#50593=CARTESIAN_POINT('Ctrl Pts',(-6.26738322480352,-3.96507786318383,
-17.1352142780564));
#50594=CARTESIAN_POINT('Ctrl Pts',(-6.2668123124285,-3.94182226820349,-16.9036027107862));
#50595=CARTESIAN_POINT('Ctrl Pts',(-6.26620865503669,-3.9250890327587,-16.6689142257609));
#50596=CARTESIAN_POINT('Ctrl Pts',(-6.26557225223362,-3.91530349225849,
-16.4315345452492));
#50597=CARTESIAN_POINT('Ctrl Pts',(-6.26502584108532,-3.90690169327874,
-16.2277219548773));
#50598=CARTESIAN_POINT('Ctrl Pts',(-6.2644552905974,-3.903621743592,-16.0219261954994));
#50599=CARTESIAN_POINT('Ctrl Pts',(-6.26386060052019,-3.90573752923273,
-15.8144217504595));
#50600=CARTESIAN_POINT('Ctrl Pts',(6.26385989016308,-3.90573722907187,-15.8144313885695));
#50601=CARTESIAN_POINT('Ctrl Pts',(5.97553399679439,-3.82580629714082,-15.9103385752986));
#50602=CARTESIAN_POINT('Ctrl Pts',(5.68536880827791,-3.75082902346428,-15.998984836958));
#50603=CARTESIAN_POINT('Ctrl Pts',(5.39385181719438,-3.68107864601722,-16.0804594738038));
#50604=CARTESIAN_POINT('Ctrl Pts',(5.12003902107913,-3.61556429706663,-16.1569860530755));
#50605=CARTESIAN_POINT('Ctrl Pts',(4.84503362991563,-3.55466183515149,-16.2271853098323));
#50606=CARTESIAN_POINT('Ctrl Pts',(4.56923960300567,-3.49857607970672,-16.2911687766404));
#50607=CARTESIAN_POINT('Ctrl Pts',(4.31279432864831,-3.44642510637448,-16.3506633852936));
#50608=CARTESIAN_POINT('Ctrl Pts',(4.05566719282585,-3.39843896167755,-16.4047836798324));
#50609=CARTESIAN_POINT('Ctrl Pts',(3.79818295898821,-3.35475746998996,-16.4536554844221));
#50610=CARTESIAN_POINT('Ctrl Pts',(3.57800514413088,-3.3174049096171,-16.4954463427683));
#50611=CARTESIAN_POINT('Ctrl Pts',(3.35756621340383,-3.28319976136122,-16.5333998249633));
#50612=CARTESIAN_POINT('Ctrl Pts',(3.13706923218936,-3.25221122731596,-16.5676189494495));
#50613=CARTESIAN_POINT('Ctrl Pts',(2.89173684623179,-3.21773233806868,-16.6056923026961));
#50614=CARTESIAN_POINT('Ctrl Pts',(2.64636709253532,-3.18724212042279,-16.639157630225));
#50615=CARTESIAN_POINT('Ctrl Pts',(2.4011994254868,-3.16079038021371,-16.6680517792548));
#50616=CARTESIAN_POINT('Ctrl Pts',(2.15979139190104,-3.13474427606927,-16.6965028380074));
#50617=CARTESIAN_POINT('Ctrl Pts',(1.91857929450951,-3.11261378305586,-16.7205218280064));
#50618=CARTESIAN_POINT('Ctrl Pts',(1.67779173970442,-3.09441416005317,-16.7401828536933));
#50619=CARTESIAN_POINT('Ctrl Pts',(1.43871515257066,-3.07634385837945,-16.7597041737406));
#50620=CARTESIAN_POINT('Ctrl Pts',(1.20005709610199,-3.06214882614483,-16.7749291990503));
#50621=CARTESIAN_POINT('Ctrl Pts',(0.962041338001033,-3.05181105112491,
-16.7859696350219));
#50622=CARTESIAN_POINT('Ctrl Pts',(0.725844259084509,-3.04155226707765,
-16.7969257109862));
#50623=CARTESIAN_POINT('Ctrl Pts',(0.490279700428395,-3.03509205442575,
-16.8037608856791));
#50624=CARTESIAN_POINT('Ctrl Pts',(0.255566339400218,-3.03237950988673,
-16.806623472729));
#50625=CARTESIAN_POINT('Ctrl Pts',(0.170630036434285,-3.03139791470287,
-16.8076593641664));
#50626=CARTESIAN_POINT('Ctrl Pts',(0.0858051992296905,-3.03090676284046,
-16.8081754131188));
#50627=CARTESIAN_POINT('Ctrl Pts',(0.00110219042761073,-3.03090254471751,
-16.8081799291764));
#50628=CARTESIAN_POINT('Ctrl Pts',(0.000734796036953708,-3.03090252642165,
-16.8081799487646));
#50629=CARTESIAN_POINT('Ctrl Pts',(0.000367399226901863,-3.0309025172856,
-16.8081799587317));
#50630=CARTESIAN_POINT('Ctrl Pts',(-1.6247122406382E-12,-3.03090251730972,
-16.808179959077));
#50631=CARTESIAN_POINT('Ctrl Pts',(-0.229875830423132,-3.03090253239659,
-16.8081801751603));
#50632=CARTESIAN_POINT('Ctrl Pts',(-0.46069844667378,-3.03449140238313,
-16.8044103498536));
#50633=CARTESIAN_POINT('Ctrl Pts',(-0.692242623528576,-3.04173275150852,
-16.7967117441749));
#50634=CARTESIAN_POINT('Ctrl Pts',(-0.925635275154074,-3.04903191012559,
-16.7889516786116));
#50635=CARTESIAN_POINT('Ctrl Pts',(-1.15976105416605,-3.06004208265118,
-16.7771998500654));
#50636=CARTESIAN_POINT('Ctrl Pts',(-1.39438929807558,-3.07479400283838,
-16.7613341401061));
#50637=CARTESIAN_POINT('Ctrl Pts',(-1.63050140140359,-3.08963921859541,
-16.7453680906362));
#50638=CARTESIAN_POINT('Ctrl Pts',(-1.86712234520368,-3.10827360850861,
-16.7252359917334));
#50639=CARTESIAN_POINT('Ctrl Pts',(-2.10401706291493,-3.13069428508702,
-16.7008539691834));
#50640=CARTESIAN_POINT('Ctrl Pts',(-2.34376869870852,-3.15338535197618,
-16.6761779027569));
#50641=CARTESIAN_POINT('Ctrl Pts',(-2.58380075158332,-3.17995453594481,
-16.6471488047795));
#50642=CARTESIAN_POINT('Ctrl Pts',(-2.82386954738932,-3.21036459359605,
-16.6137208487122));
#50643=CARTESIAN_POINT('Ctrl Pts',(-2.927994146548,-3.22355429221014,-16.5992222025449));
#50644=CARTESIAN_POINT('Ctrl Pts',(-3.03212565779147,-3.23746610815007,
-16.5838965601351));
#50645=CARTESIAN_POINT('Ctrl Pts',(-3.13624419901553,-3.25209507527437,
-16.5677425234917));
#50646=CARTESIAN_POINT('Ctrl Pts',(-3.3990646725385,-3.28902213957589,-16.5269658135031));
#50647=CARTESIAN_POINT('Ctrl Pts',(-3.66179671230626,-3.33051927196033,
-16.4808834330153));
#50648=CARTESIAN_POINT('Ctrl Pts',(-3.92409681112318,-3.37646580551342,
-16.4293256145461));
#50649=CARTESIAN_POINT('Ctrl Pts',(-4.19384845018918,-3.423717609044,-16.376303118171));
#50650=CARTESIAN_POINT('Ctrl Pts',(-4.46314325816149,-3.47567475800782,
-16.3174900314543));
#50651=CARTESIAN_POINT('Ctrl Pts',(-4.7316076127716,-3.53216981419204,-16.2527504905616));
#50652=CARTESIAN_POINT('Ctrl Pts',(-5.02537496897885,-3.59398957912181,
-16.1819091909868));
#50653=CARTESIAN_POINT('Ctrl Pts',(-5.31814795279717,-3.66124259971326,
-16.103971693354));
#50654=CARTESIAN_POINT('Ctrl Pts',(-5.60943702954381,-3.73367270940399,
-16.0188149762675));
#50655=CARTESIAN_POINT('Ctrl Pts',(-5.82848677133169,-3.78814024043064,
-15.9547770209221));
#50656=CARTESIAN_POINT('Ctrl Pts',(-6.04669735500675,-3.84553455164856,
-15.8866578189599));
#50657=CARTESIAN_POINT('Ctrl Pts',(-6.26386060052019,-3.90573752923273,
-15.8144217504595));
#50658=CARTESIAN_POINT('Ctrl Pts',(6.38277618953878,-3.93902298367305,-15.7736509876441));
#50659=CARTESIAN_POINT('Ctrl Pts',(6.32406965201728,-3.92242603988433,-15.7947737499583));
#50660=CARTESIAN_POINT('Ctrl Pts',(5.68189763608108,-3.74339185396048,-16.0219765267289));
#50661=CARTESIAN_POINT('Ctrl Pts',(4.3416298703543,-3.42592551432459,-16.4111224147635));
#50662=CARTESIAN_POINT('Ctrl Pts',(2.26093495053969,-3.1113690382538,-16.7778275679097));
#50663=CARTESIAN_POINT('Ctrl Pts',(0.00239109326725635,-2.99312376423343,
-16.9112693274866));
#50664=CARTESIAN_POINT('Ctrl Pts',(-2.25660966670575,-3.11089910253385,
-16.7783633179704));
#50665=CARTESIAN_POINT('Ctrl Pts',(-4.33836522858824,-3.42525974347605,
-16.4119189559543));
#50666=CARTESIAN_POINT('Ctrl Pts',(-5.68016038563479,-3.74293403065789,
-16.0225505707191));
#50667=CARTESIAN_POINT('Ctrl Pts',(-6.32338632353712,-3.92223285081666,
-15.7950196002647));
#50668=CARTESIAN_POINT('Ctrl Pts',(-6.38277186385808,-3.93902174367425,
-15.7736525473708));
#50669=CARTESIAN_POINT('Ctrl Pts',(6.17957679916044,-3.89068228939978,-15.1604192383161));
#50670=CARTESIAN_POINT('Ctrl Pts',(6.12270909368446,-3.87483541835791,-15.1808735763493));
#50671=CARTESIAN_POINT('Ctrl Pts',(5.500659799661,-3.70388659307422,-15.400888496091));
#50672=CARTESIAN_POINT('Ctrl Pts',(4.2025877538095,-3.40064492207699,-15.7777527540127));
#50673=CARTESIAN_POINT('Ctrl Pts',(2.18817889704034,-3.10011512502998,-16.1328510982524));
#50674=CARTESIAN_POINT('Ctrl Pts',(0.00231396716250085,-2.98714523578678,
-16.2620475592341));
#50675=CARTESIAN_POINT('Ctrl Pts',(-2.18399216732578,-3.09966614175185,
-16.1333698383091));
#50676=CARTESIAN_POINT('Ctrl Pts',(-4.19942635557926,-3.40000887948827,
-15.7785241473102));
#50677=CARTESIAN_POINT('Ctrl Pts',(-5.49897707124986,-3.7034493797774,-15.4014444027214));
#50678=CARTESIAN_POINT('Ctrl Pts',(-6.12204716868564,-3.87465096080647,
-15.1811116463534));
#50679=CARTESIAN_POINT('Ctrl Pts',(-6.17957260911428,-3.89068110637816,
-15.1604207480391));
#50680=CARTESIAN_POINT('Ctrl Pts',(6.17623614235066,-3.3901470900782,-14.7509334303916));
#50681=CARTESIAN_POINT('Ctrl Pts',(6.1195290660352,-3.37449952843537,-14.7711429291056));
#50682=CARTESIAN_POINT('Ctrl Pts',(5.49920093562508,-3.2056835753871,-14.9885423978857));
#50683=CARTESIAN_POINT('Ctrl Pts',(4.20386779883051,-2.90584507060185,-15.3613285942364));
#50684=CARTESIAN_POINT('Ctrl Pts',(2.19034988765805,-2.60796875639558,-15.7133110788741));
#50685=CARTESIAN_POINT('Ctrl Pts',(0.00231704624412195,-2.49578212587921,
-15.841584047978));
#50686=CARTESIAN_POINT('Ctrl Pts',(-2.18616172967826,-2.60752317468483,
-15.7138258279247));
#50687=CARTESIAN_POINT('Ctrl Pts',(-4.20071107704675,-2.90521550125399,
-15.3620923337382));
#50688=CARTESIAN_POINT('Ctrl Pts',(-5.49752249868785,-3.20525164179727,
-14.9890918874241));
#50689=CARTESIAN_POINT('Ctrl Pts',(-6.118869010867,-3.37431738868919,-14.7713781487167));
#50690=CARTESIAN_POINT('Ctrl Pts',(-6.17623196352304,-3.39014591921539,
-14.7509349215014));
#50691=CARTESIAN_POINT('Ctrl Pts',(6.37340174051362,-2.779344847644,-14.8203009020849));
#50692=CARTESIAN_POINT('Ctrl Pts',(6.31508205120875,-2.76321556726599,-14.8408512070517));
#50693=CARTESIAN_POINT('Ctrl Pts',(5.67705854619564,-2.58918646586821,-15.0619384307092));
#50694=CARTESIAN_POINT('Ctrl Pts',(4.34347432998779,-2.27971680019969,-15.4415401757572));
#50695=CARTESIAN_POINT('Ctrl Pts',(2.26537698871116,-1.97141906261117,-15.8009351771397));
#50696=CARTESIAN_POINT('Ctrl Pts',(0.00239760332421311,-1.85503039601574,
-15.9322038348625));
#50697=CARTESIAN_POINT('Ctrl Pts',(-2.26104951319322,-1.97095717406781,
-15.8014615465953));
#50698=CARTESIAN_POINT('Ctrl Pts',(-4.34022135115418,-2.27906626152107,
-15.4423187874132));
#50699=CARTESIAN_POINT('Ctrl Pts',(-5.67533167450272,-2.58874103693919,
-15.0624974659534));
#50700=CARTESIAN_POINT('Ctrl Pts',(-6.31440322588509,-2.76302781680913,
-14.8410903928893));
#50701=CARTESIAN_POINT('Ctrl Pts',(-6.37339744190952,-2.77934363626544,
-14.8203024183022));
#50702=CARTESIAN_POINT('',(-6.249946133935,-2.76546782187014,-14.8593871026385));
#50703=CARTESIAN_POINT('Ctrl Pts',(-6.26386069626091,-3.90573717912781,
-15.8144217465729));
#50704=CARTESIAN_POINT('Ctrl Pts',(-6.25435278828631,-3.90345940501981,
-15.7850161412327));
#50705=CARTESIAN_POINT('Ctrl Pts',(-6.24502133065853,-3.89974161222485,
-15.7549842405191));
#50706=CARTESIAN_POINT('Ctrl Pts',(-6.23596915592907,-3.89443417155273,
-15.7244986756939));
#50707=CARTESIAN_POINT('Ctrl Pts',(-6.2271444796111,-3.88926011698486,-15.6947792712421));
#50708=CARTESIAN_POINT('Ctrl Pts',(-6.21858551912677,-3.88257463437956,
-15.6646290267509));
#50709=CARTESIAN_POINT('Ctrl Pts',(-6.21039361594383,-3.87426710369931,
-15.6342479860573));
#50710=CARTESIAN_POINT('Ctrl Pts',(-6.20232798335637,-3.86608762590524,
-15.6043352409495));
#50711=CARTESIAN_POINT('Ctrl Pts',(-6.19461850613904,-3.85633510187562,
-15.5741992093649));
#50712=CARTESIAN_POINT('Ctrl Pts',(-6.18736330797966,-3.84494106661073,
-15.5440647189826));
#50713=CARTESIAN_POINT('Ctrl Pts',(-6.18023558928131,-3.83374723338617,
-15.5144597149779));
#50714=CARTESIAN_POINT('Ctrl Pts',(-6.17354666467265,-3.82096863573755,
-15.4848568331048));
#50715=CARTESIAN_POINT('Ctrl Pts',(-6.1673860145996,-3.80658418723543,-15.4554941847338));
#50716=CARTESIAN_POINT('Ctrl Pts',(-6.16658691141318,-3.80471836812597,
-15.4516855305177));
#50717=CARTESIAN_POINT('Ctrl Pts',(-6.16579668723456,-3.8028255969964,-15.4478809449517));
#50718=CARTESIAN_POINT('Ctrl Pts',(-6.16501552817343,-3.80090588826776,
-15.4440809697158));
#50719=CARTESIAN_POINT('Ctrl Pts',(-6.15908467647008,-3.78633074173258,
-15.4152301367392));
#50720=CARTESIAN_POINT('Ctrl Pts',(-6.15367730115858,-3.7701987020078,-15.3866443546201));
#50721=CARTESIAN_POINT('Ctrl Pts',(-6.14886799870019,-3.75254373120564,
-15.3585666204129));
#50722=CARTESIAN_POINT('Ctrl Pts',(-6.14412030816652,-3.73511493805424,
-15.3308485897722));
#50723=CARTESIAN_POINT('Ctrl Pts',(-6.13995573756892,-3.71620200565619,
-15.303626479117));
#50724=CARTESIAN_POINT('Ctrl Pts',(-6.13643278986983,-3.69588658064368,
-15.2771349926435));
#50725=CARTESIAN_POINT('Ctrl Pts',(-6.13293052880874,-3.67569044716736,
-15.2507990633447));
#50726=CARTESIAN_POINT('Ctrl Pts',(-6.13006259738892,-3.65410845511605,
-15.2251860084886));
#50727=CARTESIAN_POINT('Ctrl Pts',(-6.12786957795671,-3.63126787890627,
-15.2005153049664));
#50728=CARTESIAN_POINT('Ctrl Pts',(-6.12568399895156,-3.60850479569017,
-15.1759283036527));
#50729=CARTESIAN_POINT('Ctrl Pts',(-6.12416889885337,-3.58449208282344,
-15.1522780155925));
#50730=CARTESIAN_POINT('Ctrl Pts',(-6.12334491227003,-3.55939782163374,
-15.1297589600051));
#50731=CARTESIAN_POINT('Ctrl Pts',(-6.12252166712978,-3.53432614086812,
-15.1072601676095));
#50732=CARTESIAN_POINT('Ctrl Pts',(-6.12238833698384,-3.50817547284213,
-15.0858911958049));
#50733=CARTESIAN_POINT('Ctrl Pts',(-6.12294457092848,-3.4811476984129,-15.0658129831534));
#50734=CARTESIAN_POINT('Ctrl Pts',(-6.1235035154685,-3.453988214365,-15.0456369269396));
#50735=CARTESIAN_POINT('Ctrl Pts',(-6.12475871787342,-3.42594380389806,
-15.0267647165739));
#50736=CARTESIAN_POINT('Ctrl Pts',(-6.12668863274399,-3.39724362941968,
-15.0093178766538));
#50737=CARTESIAN_POINT('Ctrl Pts',(-6.12862601474739,-3.3684324096208,-14.9918035322684));
#50738=CARTESIAN_POINT('Ctrl Pts',(-6.13124318893959,-3.338961185371,-14.9757258483972));
#50739=CARTESIAN_POINT('Ctrl Pts',(-6.13449853919524,-3.30907413388349,
-14.9611603452345));
#50740=CARTESIAN_POINT('Ctrl Pts',(-6.13779129187055,-3.27884369444872,
-14.9464274913971));
#50741=CARTESIAN_POINT('Ctrl Pts',(-6.14173674640982,-3.24818868400451,
-14.9332418161091));
#50742=CARTESIAN_POINT('Ctrl Pts',(-6.14627441472987,-3.21736136586032,
-14.9216307439335));
#50743=CARTESIAN_POINT('Ctrl Pts',(-6.14957853519337,-3.19491433678491,
-14.9131760975221));
#50744=CARTESIAN_POINT('Ctrl Pts',(-6.15319626410588,-3.1723759686912,-14.9055552119477));
#50745=CARTESIAN_POINT('Ctrl Pts',(-6.15709971483306,-3.14983968148244,
-14.8987623755919));
#50746=CARTESIAN_POINT('Ctrl Pts',(-6.16255610037322,-3.11833763873896,
-14.8892671016255));
#50747=CARTESIAN_POINT('Ctrl Pts',(-6.16857091169139,-3.08684101637309,
-14.8813914186133));
#50748=CARTESIAN_POINT('Ctrl Pts',(-6.17505758164135,-3.05558476286159,
-14.8750798677663));
#50749=CARTESIAN_POINT('Ctrl Pts',(-6.18169263943854,-3.02361349714708,
-14.8686239350639));
#50750=CARTESIAN_POINT('Ctrl Pts',(-6.18882103907761,-2.99189436209302,
-14.8638040067938));
#50751=CARTESIAN_POINT('Ctrl Pts',(-6.19634461080315,-2.96064532558646,
-14.8605179833599));
#50752=CARTESIAN_POINT('Ctrl Pts',(-6.20397961974074,-2.92893343637719,
-14.8571832881909));
#50753=CARTESIAN_POINT('Ctrl Pts',(-6.21202124066049,-2.89770605675946,
-14.8554275574933));
#50754=CARTESIAN_POINT('Ctrl Pts',(-6.22036670484762,-2.86714907664217,
-14.8551100875152));
#50755=CARTESIAN_POINT('Ctrl Pts',(-6.22891230656577,-2.8358592914443,-14.854785004101));
#50756=CARTESIAN_POINT('Ctrl Pts',(-6.23777617294652,-2.80527266144069,
-14.8559672194602));
#50757=CARTESIAN_POINT('Ctrl Pts',(-6.2468530507251,-2.775540419464,-14.8584817266279));
#50758=CARTESIAN_POINT('Ctrl Pts',(-6.2478814089936,-2.77217192672634,-14.8587666058893));
#50759=CARTESIAN_POINT('Ctrl Pts',(-6.24891250958138,-2.76881434916645,
-14.8590685685164));
#50760=CARTESIAN_POINT('Ctrl Pts',(-6.2499462061289,-2.76546786755201,-14.8593873480964));
#50761=CARTESIAN_POINT('Ctrl Pts',(6.24994601332121,-2.76546575790955,-14.8593877960249));
#50762=CARTESIAN_POINT('Ctrl Pts',(6.23073047753292,-2.76025017414552,-14.8660101204524));
#50763=CARTESIAN_POINT('Ctrl Pts',(6.21150010023597,-2.75505455214819,-14.8726007831637));
#50764=CARTESIAN_POINT('Ctrl Pts',(6.19225495680607,-2.74987900475405,-14.8791597838055));
#50765=CARTESIAN_POINT('Ctrl Pts',(5.87844425507332,-2.66548669219361,-14.9861106413847));
#50766=CARTESIAN_POINT('Ctrl Pts',(5.560709433538,-2.58643024421835,-15.0846465181307));
#50767=CARTESIAN_POINT('Ctrl Pts',(5.23942746496503,-2.51325265395543,-15.1747448746766));
#50768=CARTESIAN_POINT('Ctrl Pts',(5.1126024482369,-2.48436603716071,-15.2103109091692));
#50769=CARTESIAN_POINT('Ctrl Pts',(4.9852244466522,-2.45639572037815,-15.2445617066485));
#50770=CARTESIAN_POINT('Ctrl Pts',(4.85731578768611,-2.42937608683371,-15.2774940624876));
#50771=CARTESIAN_POINT('Ctrl Pts',(4.70825219270268,-2.39788765013344,-15.3158731323045));
#50772=CARTESIAN_POINT('Ctrl Pts',(4.55847124802094,-2.36768574506229,-15.3524616131821));
#50773=CARTESIAN_POINT('Ctrl Pts',(4.40800948962857,-2.33881486398786,-15.3872540434359));
#50774=CARTESIAN_POINT('Ctrl Pts',(4.32035481797119,-2.32199552312626,-15.4075231076994));
#50775=CARTESIAN_POINT('Ctrl Pts',(4.23246905680847,-2.30562793676945,-15.4271825781245));
#50776=CARTESIAN_POINT('Ctrl Pts',(4.14436205067732,-2.28971964526396,-15.4462315091494));
#50777=CARTESIAN_POINT('Ctrl Pts',(4.02468944586554,-2.26811198015124,-15.4721049929362));
#50778=CARTESIAN_POINT('Ctrl Pts',(3.90460700146106,-2.2473522258916,-15.4968523834063));
#50779=CARTESIAN_POINT('Ctrl Pts',(3.7841358923644,-2.2274589624909,-15.5204711633146));
#50780=CARTESIAN_POINT('Ctrl Pts',(3.72390033781608,-2.21751233079056,-15.5322805532687));
#50781=CARTESIAN_POINT('Ctrl Pts',(3.66356761388492,-2.20778231952401,-15.5438077759747));
#50782=CARTESIAN_POINT('Ctrl Pts',(3.6031404319624,-2.19827105127879,-15.5550524434222));
#50783=CARTESIAN_POINT('Ctrl Pts',(3.57292684100114,-2.19351541715618,-15.5606747771459));
#50784=CARTESIAN_POINT('Ctrl Pts',(3.54268963537251,-2.18881446865928,-15.5662264711738));
#50785=CARTESIAN_POINT('Ctrl Pts',(3.5124291552237,-2.18416846515596,-15.5717074721342));
#50786=CARTESIAN_POINT('Ctrl Pts',(3.49729891514929,-2.18184546340429,-15.5744479726143));
#50787=CARTESIAN_POINT('Ctrl Pts',(3.4821628564358,-2.1795361978934,-15.5771707997731));
#50788=CARTESIAN_POINT('Ctrl Pts',(3.46702102182034,-2.17724070036537,-15.5798759466597));
#50789=CARTESIAN_POINT('Ctrl Pts',(3.45945010451261,-2.17609295160136,-15.581228520103));
#50790=CARTESIAN_POINT('Ctrl Pts',(3.45187774322886,-2.1749486448326,-15.5825766734749));
#50791=CARTESIAN_POINT('Ctrl Pts',(3.4443039433257,-2.17380778398253,-15.5839204058893));
#50792=CARTESIAN_POINT('Ctrl Pts',(3.43673014342255,-2.17266692313246,-15.5852641383038));
#50793=CARTESIAN_POINT('Ctrl Pts',(3.43037813366342,-2.17171258314623,-15.5863879362203));
#50794=CARTESIAN_POINT('Ctrl Pts',(3.42157823311786,-2.17039554309748,-15.5879383393621));
#50795=CARTESIAN_POINT('Ctrl Pts',(3.12618810143945,-2.12618588056643,-15.6399814034683));
#50796=CARTESIAN_POINT('Ctrl Pts',(2.82944930104073,-2.0874553149349,-15.6851449519319));
#50797=CARTESIAN_POINT('Ctrl Pts',(2.5316589119422,-2.05443685070837,-15.7234683965577));
#50798=CARTESIAN_POINT('Ctrl Pts',(2.45451197504621,-2.04588293671605,-15.7333966429767));
#50799=CARTESIAN_POINT('Ctrl Pts',(2.3772943200674,-2.03771250803676,-15.742865620832));
#50800=CARTESIAN_POINT('Ctrl Pts',(2.3000108328019,-2.02992988165436,-15.7518755957562));
#50801=CARTESIAN_POINT('Ctrl Pts',(2.0056692737147,-2.00028900409772,-15.7861909477202));
#50802=CARTESIAN_POINT('Ctrl Pts',(1.71037431067632,-1.97627097834048,-15.813851236479));
#50803=CARTESIAN_POINT('Ctrl Pts',(1.41448173569927,-1.95793907528011,-15.8348961980598));
#50804=CARTESIAN_POINT('Ctrl Pts',(1.11826650418036,-1.93958718216609,-15.8559641081533));
#50805=CARTESIAN_POINT('Ctrl Pts',(0.82145181565684,-1.92693366275149,-15.8704022996846));
#50806=CARTESIAN_POINT('Ctrl Pts',(0.524379711120614,-1.92007368135013,
-15.8782121451863));
#50807=CARTESIAN_POINT('Ctrl Pts',(0.350504318392921,-1.91605855525094,
-15.8827832238335));
#50808=CARTESIAN_POINT('Ctrl Pts',(0.176540502814779,-1.91402874194139,
-15.8850828882085));
#50809=CARTESIAN_POINT('Ctrl Pts',(0.00255561583708888,-1.9140086853341,
-15.8851052067127));
#50810=CARTESIAN_POINT('Ctrl Pts',(0.0020716235670054,-1.9140086295405,
-15.8851052687984));
#50811=CARTESIAN_POINT('Ctrl Pts',(0.00158763113357761,-1.91400858930194,
-15.8851053132581));
#50812=CARTESIAN_POINT('Ctrl Pts',(0.00110363853824586,-1.91400856461776,
-15.8851053400918));
#50813=CARTESIAN_POINT('Ctrl Pts',(-0.295367109470143,-1.91399344426611,
-15.8851217771233));
#50814=CARTESIAN_POINT('Ctrl Pts',(-0.591802808432749,-1.91978340639987,
-15.8785311956525));
#50815=CARTESIAN_POINT('Ctrl Pts',(-0.887865890379048,-1.93130552535533,
-15.865347476795));
#50816=CARTESIAN_POINT('Ctrl Pts',(-1.1648013594823,-1.94208324001336,-15.8530155124639));
#50817=CARTESIAN_POINT('Ctrl Pts',(-1.44141105838077,-1.95787681441081,
-15.8349144089549));
#50818=CARTESIAN_POINT('Ctrl Pts',(-1.71740521728641,-1.97865173277633,
-15.8110257152412));
#50819=CARTESIAN_POINT('Ctrl Pts',(-1.91042473226883,-1.99318089775074,
-15.7943188976315));
#50820=CARTESIAN_POINT('Ctrl Pts',(-2.10314787222578,-2.01013167948437,
-15.7747822528312));
#50821=CARTESIAN_POINT('Ctrl Pts',(-2.29547328915249,-2.02947446977817,
-15.7524039455861));
#50822=CARTESIAN_POINT('Ctrl Pts',(-2.38764658058091,-2.03874463632858,
-15.7416789864604));
#50823=CARTESIAN_POINT('Ctrl Pts',(-2.47972848825322,-2.04856429938607,
-15.7303012338651));
#50824=CARTESIAN_POINT('Ctrl Pts',(-2.57171070235722,-2.05892465772404,
-15.7182703465243));
#50825=CARTESIAN_POINT('Ctrl Pts',(-2.71366517039613,-2.07491360918477,
-15.6997032982191));
#50826=CARTESIAN_POINT('Ctrl Pts',(-2.85537926672626,-2.09219563824349,
-15.6795803778416));
#50827=CARTESIAN_POINT('Ctrl Pts',(-2.99681541196094,-2.1107489567871,-15.6578985020398));
#50828=CARTESIAN_POINT('Ctrl Pts',(-3.06753348457829,-2.1200256160589,-15.6470575641389));
#50829=CARTESIAN_POINT('Ctrl Pts',(-3.13818206762113,-2.12962009476506,
-15.6358268636259));
#50830=CARTESIAN_POINT('Ctrl Pts',(-3.20875652118209,-2.13952927635221,
-15.624205909158));
#50831=CARTESIAN_POINT('Ctrl Pts',(-3.24404374796257,-2.14448386714579,
-15.618395431924));
#50832=CARTESIAN_POINT('Ctrl Pts',(-3.27931244221733,-2.14951713346246,
-15.6124873896378));
#50833=CARTESIAN_POINT('Ctrl Pts',(-3.3145620252032,-2.15462867384623,-15.6064817125059));
#50834=CARTESIAN_POINT('Ctrl Pts',(-3.33218681669613,-2.15718444403811,
-15.6034788739399));
#50835=CARTESIAN_POINT('Ctrl Pts',(-3.34980683035885,-2.15975978273357,
-15.6004516265627));
#50836=CARTESIAN_POINT('Ctrl Pts',(-3.36742199402595,-2.1623546383924,-15.5973999611852));
#50837=CARTESIAN_POINT('Ctrl Pts',(-3.3762295758595,-2.16365206622181,-15.5958741284965));
#50838=CARTESIAN_POINT('Ctrl Pts',(-3.38503594519326,-2.16495437329122,
-15.5943421913015));
#50839=CARTESIAN_POINT('Ctrl Pts',(-3.39384109301869,-2.16626155306888,
-15.5928041484225));
#50840=CARTESIAN_POINT('Ctrl Pts',(-3.40264624084412,-2.16756873284654,
-15.5912661055435));
#50841=CARTESIAN_POINT('Ctrl Pts',(-3.41267288227766,-2.16906370843053,
-15.5895066228579));
#50842=CARTESIAN_POINT('Ctrl Pts',(-3.42025286296309,-2.17019770396608,
-15.5881717015338));
#50843=CARTESIAN_POINT('Ctrl Pts',(-3.7512914807498,-2.21972240993068,-15.5298720134026));
#50844=CARTESIAN_POINT('Ctrl Pts',(-4.079618287111,-2.27588861931481,-15.4631235878544));
#50845=CARTESIAN_POINT('Ctrl Pts',(-4.40475725936993,-2.3382578308419,-15.3879956510477));
#50846=CARTESIAN_POINT('Ctrl Pts',(-4.72371670931558,-2.39944166636925,
-15.3142955798661));
#50847=CARTESIAN_POINT('Ctrl Pts',(-5.03960868942063,-2.4665955473129,-15.2325312282107));
#50848=CARTESIAN_POINT('Ctrl Pts',(-5.35209806335916,-2.53926302950475,
-15.1427479434758));
#50849=CARTESIAN_POINT('Ctrl Pts',(-5.63433594988217,-2.60489571433585,
-15.0616564035962));
#50850=CARTESIAN_POINT('Ctrl Pts',(-5.91379807239021,-2.67502673187186,
-14.9740228129603));
#50851=CARTESIAN_POINT('Ctrl Pts',(-6.19021699498113,-2.7493336727775,-14.8798537270554));
#50852=CARTESIAN_POINT('Ctrl Pts',(-6.21014258404868,-2.75469007007286,
-14.8730655719934));
#50853=CARTESIAN_POINT('Ctrl Pts',(-6.23005235057421,-2.76006817087034,
-14.8662434464133));
#50854=CARTESIAN_POINT('Ctrl Pts',(-6.2499462061289,-2.76546786755201,-14.8593873480964));
#50855=CARTESIAN_POINT('Ctrl Pts',(-6.25025869058268,-3.90195425102708,
-15.8298806636529));
#50856=CARTESIAN_POINT('Ctrl Pts',(-6.29004325280698,-3.91230167814786,
-15.8159179950948));
#50857=CARTESIAN_POINT('Ctrl Pts',(-6.41684493426804,-3.95321250785999,
-15.7689312449806));
#50858=CARTESIAN_POINT('Ctrl Pts',(-6.61884385638551,-4.06299859433413,
-15.6800117310403));
#50859=CARTESIAN_POINT('Ctrl Pts',(-6.82673050587102,-4.25689239114287,
-15.5624948978267));
#50860=CARTESIAN_POINT('Ctrl Pts',(-6.9795005695021,-4.49148568888774,-15.4459527338404));
#50861=CARTESIAN_POINT('Ctrl Pts',(-7.07130089065108,-4.73958816623202,
-15.3403618218109));
#50862=CARTESIAN_POINT('Ctrl Pts',(-7.10319232002285,-4.94126548594463,
-15.2651787834553));
#50863=CARTESIAN_POINT('Ctrl Pts',(-7.1060521427303,-5.05547800808013,-15.2264033130095));
#50864=CARTESIAN_POINT('Ctrl Pts',(-7.10556044294757,-5.0897512085814,-15.2151090406844));
#50865=CARTESIAN_POINT('Ctrl Pts',(-6.05195504581396,-3.8612747752879,-15.216963146136));
#50866=CARTESIAN_POINT('Ctrl Pts',(-6.08716037978976,-3.87017573546989,
-15.2045780432604));
#50867=CARTESIAN_POINT('Ctrl Pts',(-6.1995564342606,-3.90545408683933,-15.162827533509));
#50868=CARTESIAN_POINT('Ctrl Pts',(-6.37953440856656,-4.00078013167406,
-15.0834346606072));
#50869=CARTESIAN_POINT('Ctrl Pts',(-6.5657926704312,-4.17048213829989,-14.9781170113052));
#50870=CARTESIAN_POINT('Ctrl Pts',(-6.70320606919983,-4.3769561365539,-14.8736153645538));
#50871=CARTESIAN_POINT('Ctrl Pts',(-6.78592821391996,-4.59600742080904,
-14.7791864889897));
#50872=CARTESIAN_POINT('Ctrl Pts',(-6.81464125639214,-4.77415894173948,
-14.7123493325573));
#50873=CARTESIAN_POINT('Ctrl Pts',(-6.81720646837307,-4.87487688660176,
-14.6781178958172));
#50874=CARTESIAN_POINT('Ctrl Pts',(-6.81676488843804,-4.90507416047635,
-14.6681734327106));
#50875=CARTESIAN_POINT('Ctrl Pts',(-6.04007731699225,-3.3653514635855,-14.8038119958432));
#50876=CARTESIAN_POINT('Ctrl Pts',(-6.08856713435085,-3.37753324040758,
-14.7871067961518));
#50877=CARTESIAN_POINT('Ctrl Pts',(-6.24254103358638,-3.425594380489,-14.7312217087171));
#50878=CARTESIAN_POINT('Ctrl Pts',(-6.48501737959783,-3.55339098767982,
-14.6272481342667));
#50879=CARTESIAN_POINT('Ctrl Pts',(-6.73142927381077,-3.77609611461869,
-14.4922306969956));
#50880=CARTESIAN_POINT('Ctrl Pts',(-6.91088322984329,-4.04290408094191,
-14.3598675521506));
#50881=CARTESIAN_POINT('Ctrl Pts',(-7.01826470959118,-4.32360657295049,
-14.240582028433));
#50882=CARTESIAN_POINT('Ctrl Pts',(-7.05564360353183,-4.55181817515552,
-14.1555764233942));
#50883=CARTESIAN_POINT('Ctrl Pts',(-7.05902455314479,-4.6816266250268,-14.111509966447));
#50884=CARTESIAN_POINT('Ctrl Pts',(-7.05844486989701,-4.7206606857481,-14.0986455118703));
#50885=CARTESIAN_POINT('Ctrl Pts',(-6.2228042713461,-2.74964964265847,-14.8703245545406));
#50886=CARTESIAN_POINT('Ctrl Pts',(-6.2934601889109,-2.76762147752745,-14.846322496578));
#50887=CARTESIAN_POINT('Ctrl Pts',(-6.51688325161155,-2.8382386871185,-14.7664886202973));
#50888=CARTESIAN_POINT('Ctrl Pts',(-6.86412034506044,-3.02348438622559,
-14.6204460875284));
#50889=CARTESIAN_POINT('Ctrl Pts',(-7.21179661010534,-3.34055464141455,
-14.4339095029604));
#50890=CARTESIAN_POINT('Ctrl Pts',(-7.46226391480826,-3.71536132613924,
-14.2526191794921));
#50891=CARTESIAN_POINT('Ctrl Pts',(-7.61136964107686,-4.10673862760579,
-14.0892628607977));
#50892=CARTESIAN_POINT('Ctrl Pts',(-7.66339948514605,-4.42475343273525,
-13.9718572663327));
#50893=CARTESIAN_POINT('Ctrl Pts',(-7.66815498236441,-4.60657091398318,
-13.9102256869705));
#50894=CARTESIAN_POINT('Ctrl Pts',(-7.66734234719229,-4.66138037255722,
-13.8921454958944));
#50895=CARTESIAN_POINT('',(-7.00000966899638,-4.92966193733403,-14.7967990230951));
#50896=CARTESIAN_POINT('',(-6.99999994660866,-3.16612878336916,-14.5427417016117));
#50897=CARTESIAN_POINT('Ctrl Pts',(-7.,-4.92966193738822,-14.7967990231518));
#50898=CARTESIAN_POINT('Ctrl Pts',(-7.,-4.82655938421173,-14.7559075381302));
#50899=CARTESIAN_POINT('Ctrl Pts',(-7.,-4.73328972165707,-14.7213201925373));
#50900=CARTESIAN_POINT('Ctrl Pts',(-7.,-4.65148596355912,-14.6933836120477));
#50901=CARTESIAN_POINT('Ctrl Pts',(-7.,-4.61058408451014,-14.6794153218028));
#50902=CARTESIAN_POINT('Ctrl Pts',(-7.,-4.57256028200403,-14.6670630335082));
#50903=CARTESIAN_POINT('Ctrl Pts',(-7.,-4.53765362432334,-14.6561593075045));
#50904=CARTESIAN_POINT('Ctrl Pts',(-7.,-4.520200295483,-14.6507074445026));
#50905=CARTESIAN_POINT('Ctrl Pts',(-7.,-4.50352626970067,-14.6456161316604));
#50906=CARTESIAN_POINT('Ctrl Pts',(-7.,-4.48766007054382,-14.6408574818086));
#50907=CARTESIAN_POINT('Ctrl Pts',(-7.,-4.4797269709654,-14.6384781568827));
#50908=CARTESIAN_POINT('Ctrl Pts',(-7.,-4.47199582804335,-14.6361819977044));
#50909=CARTESIAN_POINT('Ctrl Pts',(-7.,-4.46446994884579,-14.6339652362007));
#50910=CARTESIAN_POINT('Ctrl Pts',(-7.,-4.46070700924702,-14.6328568554488));
#50911=CARTESIAN_POINT('Ctrl Pts',(-7.,-4.45699538557936,-14.6317683241155));
#50912=CARTESIAN_POINT('Ctrl Pts',(-7.,-4.45333548850481,-14.6306991714511));
#50913=CARTESIAN_POINT('Ctrl Pts',(-7.,-4.44967559143025,-14.6296300187866));
#50914=CARTESIAN_POINT('Ctrl Pts',(-7.,-4.44768768929838,-14.629049949197));
#50915=CARTESIAN_POINT('Ctrl Pts',(-7.,-4.44251138169973,-14.6275493766042));
#50916=CARTESIAN_POINT('Ctrl Pts',(-7.,-4.35969046012135,-14.6035402151185));
#50917=CARTESIAN_POINT('Ctrl Pts',(-7.,-4.27942521485861,-14.583045316773));
#50918=CARTESIAN_POINT('Ctrl Pts',(-7.,-4.20233627926549,-14.5661438464499));
#50919=CARTESIAN_POINT('Ctrl Pts',(-7.,-4.12524734367237,-14.5492423761268));
#50920=CARTESIAN_POINT('Ctrl Pts',(-7.,-4.05295709621141,-14.5361569482499));
#50921=CARTESIAN_POINT('Ctrl Pts',(-7.,-3.98143433660398,-14.5256713498039));
#50922=CARTESIAN_POINT('Ctrl Pts',(-7.,-3.83838881738911,-14.5047001529118));
#50923=CARTESIAN_POINT('Ctrl Pts',(-7.,-3.69587225506059,-14.4945152230835));
#50924=CARTESIAN_POINT('Ctrl Pts',(-7.,-3.55821948693664,-14.4973989631904));
#50925=CARTESIAN_POINT('Ctrl Pts',(-7.,-3.42056671881268,-14.5002827032973));
#50926=CARTESIAN_POINT('Ctrl Pts',(-7.,-3.28800980542072,-14.5162054735111));
#50927=CARTESIAN_POINT('Ctrl Pts',(-7.,-3.1661290724247,-14.5427417758091));
#50928=CARTESIAN_POINT('Ctrl Pts',(-6.24994600940207,-2.76546774305749,
-14.8593866792155));
#50929=CARTESIAN_POINT('Ctrl Pts',(-6.29984424415668,-2.77900840334636,
-14.8421907554761));
#50930=CARTESIAN_POINT('Ctrl Pts',(-6.3487263309393,-2.79444082765551,-14.824724359647));
#50931=CARTESIAN_POINT('Ctrl Pts',(-6.39660944973819,-2.81168414910411,
-14.8069977010491));
#50932=CARTESIAN_POINT('Ctrl Pts',(-6.40679347373321,-2.81535154596111,
-14.8032275056014));
#50933=CARTESIAN_POINT('Ctrl Pts',(-6.41693226861308,-2.81910103784002,
-14.7994454978845));
#50934=CARTESIAN_POINT('Ctrl Pts',(-6.42702592397545,-2.82293213144578,
-14.7956517160494));
#50935=CARTESIAN_POINT('Ctrl Pts',(-6.47528669444697,-2.84124973022688,
-14.777512515949));
#50936=CARTESIAN_POINT('Ctrl Pts',(-6.52251730631065,-2.86142901124132,
-14.7591047840457));
#50937=CARTESIAN_POINT('Ctrl Pts',(-6.56875184392231,-2.88342099387357,
-14.7404224436367));
#50938=CARTESIAN_POINT('Ctrl Pts',(-6.59562994595511,-2.89620586820405,
-14.7295616050155));
#50939=CARTESIAN_POINT('Ctrl Pts',(-6.62217102362711,-2.90960426555278,
-14.7186078033138));
#50940=CARTESIAN_POINT('Ctrl Pts',(-6.6483778235703,-2.92361352158998,-14.7075588234604));
#50941=CARTESIAN_POINT('Ctrl Pts',(-6.6940303125624,-2.94801777576873,-14.6883113978981));
#50942=CARTESIAN_POINT('Ctrl Pts',(-6.73865998128682,-2.97426707548207,
-14.668779879028));
#50943=CARTESIAN_POINT('Ctrl Pts',(-6.78225031116346,-3.00237511820988,
-14.648952239572));
#50944=CARTESIAN_POINT('Ctrl Pts',(-6.80367803687637,-3.01619220634853,
-14.6392055544471));
#50945=CARTESIAN_POINT('Ctrl Pts',(-6.82485408960695,-3.03045902932654,
-14.6293872670855));
#50946=CARTESIAN_POINT('Ctrl Pts',(-6.84577313284396,-3.0451803876863,-14.6194957968782));
#50947=CARTESIAN_POINT('Ctrl Pts',(-6.88817037401047,-3.07501659833921,
-14.5994484628238));
#50948=CARTESIAN_POINT('Ctrl Pts',(-6.92951466896079,-3.10671819929499,
-14.5791004207225));
#50949=CARTESIAN_POINT('Ctrl Pts',(-6.96976417942069,-3.14033372433756,
-14.5584342379362));
#50950=CARTESIAN_POINT('Ctrl Pts',(-6.97991293236787,-3.14880974441703,
-14.5532233426716));
#50951=CARTESIAN_POINT('Ctrl Pts',(-6.98999186172936,-3.15740758124442,
-14.5479922288204));
#50952=CARTESIAN_POINT('Ctrl Pts',(-6.99999983624227,-3.16612827049482,
-14.5427406396167));
#50953=CARTESIAN_POINT('Ctrl Pts',(-6.26385672821774,-3.90575168809173,
-15.8144219056792));
#50954=CARTESIAN_POINT('Ctrl Pts',(-6.29496070557119,-3.91447746283058,
-15.7944156170949));
#50955=CARTESIAN_POINT('Ctrl Pts',(-6.32584063897265,-3.92481222694173,
-15.7736495821958));
#50956=CARTESIAN_POINT('Ctrl Pts',(-6.35632273915694,-3.93678606640697,
-15.7521476173342));
#50957=CARTESIAN_POINT('Ctrl Pts',(-6.40025562382785,-3.95404358164096,
-15.7211575170211));
#50958=CARTESIAN_POINT('Ctrl Pts',(-6.44336383185676,-3.97470665376692,
-15.688637704132));
#50959=CARTESIAN_POINT('Ctrl Pts',(-6.48515831758161,-3.99873227768996,
-15.6546924201779));
#50960=CARTESIAN_POINT('Ctrl Pts',(-6.51589372349728,-4.01640057270173,
-15.6297292686244));
#50961=CARTESIAN_POINT('Ctrl Pts',(-6.54591786321893,-4.03588708150959,
-15.6039955938197));
#50962=CARTESIAN_POINT('Ctrl Pts',(-6.57501945966857,-4.05717477201828,
-15.5775396377571));
#50963=CARTESIAN_POINT('Ctrl Pts',(-6.57561881429194,-4.05761319730362,
-15.5769947707561));
#50964=CARTESIAN_POINT('Ctrl Pts',(-6.57621777705022,-4.05805238665068,
-15.5764495976003));
#50965=CARTESIAN_POINT('Ctrl Pts',(-6.57681634635688,-4.0584923394855,-15.5759041187764));
#50966=CARTESIAN_POINT('Ctrl Pts',(-6.61481470367452,-4.0864214110811,-15.5412760497653));
#50967=CARTESIAN_POINT('Ctrl Pts',(-6.65123111078806,-4.11742775113867,
-15.505414438286));
#50968=CARTESIAN_POINT('Ctrl Pts',(-6.68563918955076,-4.15136225110879,
-15.4684540374091));
#50969=CARTESIAN_POINT('Ctrl Pts',(-6.71047710027362,-4.17585830293707,
-15.441773700399));
#50970=CARTESIAN_POINT('Ctrl Pts',(-6.73426779502671,-4.20187999599657,
-15.4145211940823));
#50971=CARTESIAN_POINT('Ctrl Pts',(-6.75683528395995,-4.2293715007421,-15.3867541360492));
#50972=CARTESIAN_POINT('Ctrl Pts',(-6.76261505054204,-4.23641235853934,
-15.3796427062141));
#50973=CARTESIAN_POINT('Ctrl Pts',(-6.76831450584281,-4.24354963337093,
-15.3724975569579));
#50974=CARTESIAN_POINT('Ctrl Pts',(-6.77393124261298,-4.25078171331711,
-15.3653197709766));
#50975=CARTESIAN_POINT('Ctrl Pts',(-6.78358602365561,-4.26321315727118,
-15.3529816545836));
#50976=CARTESIAN_POINT('Ctrl Pts',(-6.79299642325081,-4.27592472578274,
-15.3405470914351));
#50977=CARTESIAN_POINT('Ctrl Pts',(-6.80214982425869,-4.28890819117643,
-15.3280217832807));
#50978=CARTESIAN_POINT('Ctrl Pts',(-6.80672652476263,-4.29539992387327,
-15.3217591292036));
#50979=CARTESIAN_POINT('Ctrl Pts',(-6.81123897066713,-4.30195963441504,
-15.3154737890702));
#50980=CARTESIAN_POINT('Ctrl Pts',(-6.81568553119839,-4.30858628652225,
-15.3091665045848));
#50981=CARTESIAN_POINT('Ctrl Pts',(-6.81790881146402,-4.31189961257586,
-15.3060128623421));
#50982=CARTESIAN_POINT('Ctrl Pts',(-6.82011562004755,-4.31522967427845,
-15.3028537340249));
#50983=CARTESIAN_POINT('Ctrl Pts',(-6.82230575025301,-4.31857634267313,
-15.2996892133226));
#50984=CARTESIAN_POINT('Ctrl Pts',(-6.82390724309922,-4.32102353301795,
-15.2973752151623));
#50985=CARTESIAN_POINT('Ctrl Pts',(-6.82591988230215,-4.32413073507111,
-15.2944445695705));
#50986=CARTESIAN_POINT('Ctrl Pts',(-6.82742098616778,-4.32647033414201,
-15.2922436785592));
#50987=CARTESIAN_POINT('Ctrl Pts',(-6.82797272501414,-4.3273302664371,-15.2914347291618));
#50988=CARTESIAN_POINT('Ctrl Pts',(-6.82845586142347,-4.32808612215464,
-15.2907243891491));
#50989=CARTESIAN_POINT('Ctrl Pts',(-6.82882589711254,-4.32866603950762,
-15.2901795682984));
#50990=CARTESIAN_POINT('Ctrl Pts',(-6.84354636430377,-4.35173585309678,
-15.2685059360108));
#50991=CARTESIAN_POINT('Ctrl Pts',(-6.85802914311084,-4.37643135241196,
-15.2457503303666));
#50992=CARTESIAN_POINT('Ctrl Pts',(-6.8719932617384,-4.40284622357026,-15.2219432148758));
#50993=CARTESIAN_POINT('Ctrl Pts',(-6.87753155881442,-4.41332260289653,
-15.2125010952815));
#50994=CARTESIAN_POINT('Ctrl Pts',(-6.88298778531057,-4.42406926830202,
-15.2028937746778));
#50995=CARTESIAN_POINT('Ctrl Pts',(-6.88834236978538,-4.43509135495778,
-15.1931240035397));
#50996=CARTESIAN_POINT('Ctrl Pts',(-6.90122774509452,-4.46161511677671,
-15.1696138379252));
#50997=CARTESIAN_POINT('Ctrl Pts',(-6.91352688599134,-4.48973564698527,
-15.1451614820643));
#50998=CARTESIAN_POINT('Ctrl Pts',(-6.92496496488142,-4.5194897156191,-15.1198210062146));
#50999=CARTESIAN_POINT('Ctrl Pts',(-6.93265775367141,-4.53950109758651,
-15.1027780280691));
#51000=CARTESIAN_POINT('Ctrl Pts',(-6.93996038631962,-4.56025090255248,
-15.0853337152217));
#51001=CARTESIAN_POINT('Ctrl Pts',(-6.94677915170763,-4.58174363379248,
-15.0675102808871));
#51002=CARTESIAN_POINT('Ctrl Pts',(-6.95371914500644,-4.60361847510039,
-15.0493699713434));
#51003=CARTESIAN_POINT('Ctrl Pts',(-6.96015804529918,-4.62626292645609,
-15.0308368775598));
#51004=CARTESIAN_POINT('Ctrl Pts',(-6.96598676876777,-4.64967549092573,
-15.0119400880676));
#51005=CARTESIAN_POINT('Ctrl Pts',(-6.97384657551408,-4.68124642290739,
-14.9864585028913));
#51006=CARTESIAN_POINT('Ctrl Pts',(-6.98059788182425,-4.71421565278788,
-14.9603145265921));
#51007=CARTESIAN_POINT('Ctrl Pts',(-6.98597534825046,-4.74853165282223,
-14.9336023621482));
#51008=CARTESIAN_POINT('Ctrl Pts',(-6.99135281467668,-4.78284765285657,
-14.9068901977044));
#51009=CARTESIAN_POINT('Ctrl Pts',(-6.99535715189965,-4.81851060906578,
-14.8796095675904));
#51010=CARTESIAN_POINT('Ctrl Pts',(-6.99768410298933,-4.85543612803544,
-14.8518810527172));
#51011=CARTESIAN_POINT('Ctrl Pts',(-6.99920998548749,-4.8796497882972,-14.8336982659226));
#51012=CARTESIAN_POINT('Ctrl Pts',(-7.00001358933039,-4.90440581697676,
-14.8153234008063));
#51013=CARTESIAN_POINT('Ctrl Pts',(-7.00001301944785,-4.92966193744617,
-14.7967990231449));
#51014=CARTESIAN_POINT('Ctrl Pts',(-6.22833844179566,-8.85454586402646,
-25.6432279269192));
#51015=CARTESIAN_POINT('Ctrl Pts',(-6.2291146949257,-8.44340768883296,-25.3458769589811));
#51016=CARTESIAN_POINT('Ctrl Pts',(-6.23070504669655,-7.53909867425292,
-24.6003976212981));
#51017=CARTESIAN_POINT('Ctrl Pts',(-6.23225398339099,-6.30570986941791,
-23.2360111793486));
#51018=CARTESIAN_POINT('Ctrl Pts',(-6.23180618158922,-5.23101094495107,
-21.5552478274574));
#51019=CARTESIAN_POINT('Ctrl Pts',(-6.22991430233278,-4.44858169421722,
-19.7183955817659));
#51020=CARTESIAN_POINT('Ctrl Pts',(-6.22625526139252,-3.98055545467836,
-17.7796362264324));
#51021=CARTESIAN_POINT('Ctrl Pts',(-6.22146023609855,-3.85842008520426,
-16.046045618656));
#51022=CARTESIAN_POINT('Ctrl Pts',(-6.21819598059103,-3.92587530766592,
-14.9770433487066));
#51023=CARTESIAN_POINT('Ctrl Pts',(-6.21685873948199,-3.97244993924363,
-14.5712621246747));
#51024=CARTESIAN_POINT('Ctrl Pts',(-6.72318434148056,-8.92252624598781,
-25.5491630136165));
#51025=CARTESIAN_POINT('Ctrl Pts',(-6.72388041677531,-8.51560341410963,
-25.2543690324476));
#51026=CARTESIAN_POINT('Ctrl Pts',(-6.72525502274418,-7.62056569287233,
-24.5154728102739));
#51027=CARTESIAN_POINT('Ctrl Pts',(-6.72662850357054,-6.40000803919394,
-23.1640897398429));
#51028=CARTESIAN_POINT('Ctrl Pts',(-6.72623178592576,-5.33567942894206,
-21.499981562341));
#51029=CARTESIAN_POINT('Ctrl Pts',(-6.7245683841393,-4.56007598310717,-19.6816180801987));
#51030=CARTESIAN_POINT('Ctrl Pts',(-6.72135051761313,-4.09475438480478,
-17.7621504532083));
#51031=CARTESIAN_POINT('Ctrl Pts',(-6.71710127101458,-3.97131583603131,
-16.0452264577192));
#51032=CARTESIAN_POINT('Ctrl Pts',(-6.7142340588082,-4.03648107493104,-14.9860221510941));
#51033=CARTESIAN_POINT('Ctrl Pts',(-6.71304026512286,-4.0819462151573,-14.5839118639174));
#51034=CARTESIAN_POINT('Ctrl Pts',(-7.02734369613163,-9.16102046075851,
-25.2191575822356));
#51035=CARTESIAN_POINT('Ctrl Pts',(-7.02772459263739,-8.76821649492092,
-24.9342613568181));
#51036=CARTESIAN_POINT('Ctrl Pts',(-7.02841406477176,-7.90406911102415,
-24.2201590873639));
#51037=CARTESIAN_POINT('Ctrl Pts',(-7.02914679556069,-6.72625932453338,
-22.9153222295337));
#51038=CARTESIAN_POINT('Ctrl Pts',(-7.02893559561167,-5.69830277108108,
-21.3083981705397));
#51039=CARTESIAN_POINT('Ctrl Pts',(-7.02806566033587,-4.94894652445456,
-19.5531153239726));
#51040=CARTESIAN_POINT('Ctrl Pts',(-7.02638186928547,-4.49837668820159,
-17.6999558310792));
#51041=CARTESIAN_POINT('Ctrl Pts',(-7.02411819232694,-4.3775348597053,-16.0419479461919));
#51042=CARTESIAN_POINT('Ctrl Pts',(-7.02262219464857,-4.43938017157472,
-15.0186573153932));
#51043=CARTESIAN_POINT('Ctrl Pts',(-7.0219754326037,-4.48283582413942,-14.6302246026994));
#51044=CARTESIAN_POINT('Ctrl Pts',(-6.99838063008314,-9.45820150649603,
-24.80794711765));
#51045=CARTESIAN_POINT('Ctrl Pts',(-6.99835913457881,-9.08279985143789,
-24.5356483641088));
#51046=CARTESIAN_POINT('Ctrl Pts',(-6.99821532661173,-8.25667795636497,
-23.852925090981));
#51047=CARTESIAN_POINT('Ctrl Pts',(-6.99814245618034,-7.13148909047522,
-22.6063522236937));
#51048=CARTESIAN_POINT('Ctrl Pts',(-6.99816421970605,-6.14885192790038,
-21.070328455353));
#51049=CARTESIAN_POINT('Ctrl Pts',(-6.99828069432312,-5.43285699584306,
-19.3931406078209));
#51050=CARTESIAN_POINT('Ctrl Pts',(-6.9985045724283,-5.00216845859944,-17.6222147600737));
#51051=CARTESIAN_POINT('Ctrl Pts',(-6.9987352379504,-4.88660477512488,-16.0377473888359));
#51052=CARTESIAN_POINT('Ctrl Pts',(-6.99894168315531,-4.94565629452344,
-15.0596464715112));
#51053=CARTESIAN_POINT('Ctrl Pts',(-6.99898903503866,-4.98714444952959,
-14.6884846237969));
#51054=CARTESIAN_POINT('',(-7.00000308919771,-9.33251796322024,-24.7867179209035));
#51055=CARTESIAN_POINT('Origin',(-5.99998370363197,-9.33252808557812,-24.7867138051333));
#51056=CARTESIAN_POINT('Ctrl Pts',(-7.00001101651463,-9.33251828870258,
-24.7867134185486));
#51057=CARTESIAN_POINT('Ctrl Pts',(-7.00001786889538,-9.17932096987487,
-24.6735525287245));
#51058=CARTESIAN_POINT('Ctrl Pts',(-7.00001802523764,-9.03121143047395,
-24.5580142123416));
#51059=CARTESIAN_POINT('Ctrl Pts',(-7.00001556839827,-8.88816514599322,
-24.4406109868492));
#51060=CARTESIAN_POINT('Ctrl Pts',(-7.00001306417584,-8.74236004418057,
-24.320943500845));
#51061=CARTESIAN_POINT('Ctrl Pts',(-7.00000784356451,-8.60181528010428,
-24.1993384527498));
#51062=CARTESIAN_POINT('Ctrl Pts',(-7.00000354838409,-8.4664713655905,-24.0762961134802));
#51063=CARTESIAN_POINT('Ctrl Pts',(-7.00000225630549,-8.42575713295274,
-24.0392824476401));
#51064=CARTESIAN_POINT('Ctrl Pts',(-7.00000104345516,-8.38551332065751,
-24.0021384319859));
#51065=CARTESIAN_POINT('Ctrl Pts',(-6.99999999753994,-8.34573775429907,
-23.9648769595113));
#51066=CARTESIAN_POINT('Ctrl Pts',(-6.99999887666334,-8.30311144841288,
-23.924944934178));
#51067=CARTESIAN_POINT('Ctrl Pts',(-6.99999794690503,-8.26102290376838,
-23.8848780147828));
#51068=CARTESIAN_POINT('Ctrl Pts',(-6.99999718086759,-8.21946689146059,
-23.8446913566483));
#51069=CARTESIAN_POINT('Ctrl Pts',(-6.9999946221417,-8.08066108527976,-23.7104594809152));
#51070=CARTESIAN_POINT('Ctrl Pts',(-6.99999387750149,-7.94779827828375,
-23.5748953731845));
#51071=CARTESIAN_POINT('Ctrl Pts',(-6.99999403434654,-7.82067002322657,
-23.4385317151514));
#51072=CARTESIAN_POINT('Ctrl Pts',(-6.99999406716621,-7.79406856362658,
-23.4099977567608));
#51073=CARTESIAN_POINT('Ctrl Pts',(-6.99999414003161,-7.76771812286174,
-23.3814286214255));
#51074=CARTESIAN_POINT('Ctrl Pts',(-6.99999424548565,-7.74161668390431,
-23.3528289250926));
#51075=CARTESIAN_POINT('Ctrl Pts',(-6.99999432422097,-7.7221285250655,-23.3314754883804));
#51076=CARTESIAN_POINT('Ctrl Pts',(-6.99999441863014,-7.70323909902872,
-23.3106151714184));
#51077=CARTESIAN_POINT('Ctrl Pts',(-6.9999945313887,-7.68388254652659,-23.2890698050573));
#51078=CARTESIAN_POINT('Ctrl Pts',(-6.99999463682047,-7.66578373583508,
-23.2689244043199));
#51079=CARTESIAN_POINT('Ctrl Pts',(-6.99999475847151,-7.64727658542074,
-23.2481799736132));
#51080=CARTESIAN_POINT('Ctrl Pts',(-6.99999490350817,-7.62752046923564,
-23.2258462598882));
#51081=CARTESIAN_POINT('Ctrl Pts',(-6.99999520366053,-7.58663532381801,
-23.1796267942398));
#51082=CARTESIAN_POINT('Ctrl Pts',(-6.99999556265644,-7.5462152748296,-23.1331495451411));
#51083=CARTESIAN_POINT('Ctrl Pts',(-6.99999595370125,-7.50626142519057,
-23.0864243731837));
#51084=CARTESIAN_POINT('Ctrl Pts',(-6.99999673579089,-7.42635372591251,
-22.9929740292688));
#51085=CARTESIAN_POINT('Ctrl Pts',(-6.9999976453721,-7.34831082403186,-22.8985319939186));
#51086=CARTESIAN_POINT('Ctrl Pts',(-6.99999847632113,-7.27213997300368,
-22.8031750086351));
#51087=CARTESIAN_POINT('Ctrl Pts',(-6.99999902465851,-7.22187536817392,
-22.7402496097675));
#51088=CARTESIAN_POINT('Ctrl Pts',(-6.99999953897951,-7.17242592969274,
-22.6769257410983));
#51089=CARTESIAN_POINT('Ctrl Pts',(-6.9999999627666,-7.12379334406456,-22.6132249099148));
#51090=CARTESIAN_POINT('Ctrl Pts',(-7.00000126736881,-6.97408094982872,
-22.4171258576411));
#51091=CARTESIAN_POINT('Ctrl Pts',(-7.00000171385125,-6.83211151967692,
-22.2174579363025));
#51092=CARTESIAN_POINT('Ctrl Pts',(-7.00000170643198,-6.69789034495963,
-22.014913879793));
#51093=CARTESIAN_POINT('Ctrl Pts',(-7.00000169893338,-6.56223404405374,
-21.810204171847));
#51094=CARTESIAN_POINT('Ctrl Pts',(-7.00000122940867,-6.4344925417275,-21.6025564694009));
#51095=CARTESIAN_POINT('Ctrl Pts',(-7.00000072341992,-6.31464617992324,
-21.392638892529));
#51096=CARTESIAN_POINT('Ctrl Pts',(-7.00000046988391,-6.25459471218963,
-21.2874554025634));
#51097=CARTESIAN_POINT('Ctrl Pts',(-7.00000020716497,-6.19652510160297,
-21.1817012804143));
#51098=CARTESIAN_POINT('Ctrl Pts',(-6.99999998766523,-6.14043258691257,
-21.0754562422842));
#51099=CARTESIAN_POINT('Ctrl Pts',(-6.99999993929019,-6.12807048608338,
-21.0520411416916));
#51100=CARTESIAN_POINT('Ctrl Pts',(-6.99999989300829,-6.11580440838993,
-21.0286021859978));
#51101=CARTESIAN_POINT('Ctrl Pts',(-6.99999984878697,-6.10363415345454,
-21.0051402391711));
#51102=CARTESIAN_POINT('Ctrl Pts',(-6.99999965374735,-6.0499568442152,-20.9016605518631));
#51103=CARTESIAN_POINT('Ctrl Pts',(-6.99999949863779,-5.99814361467508,
-20.7977338296875));
#51104=CARTESIAN_POINT('Ctrl Pts',(-6.9999993818455,-5.94817680819026,-20.6934325636233));
#51105=CARTESIAN_POINT('Ctrl Pts',(-6.99999932344936,-5.92319340494786,
-20.6412819305913));
#51106=CARTESIAN_POINT('Ctrl Pts',(-6.99999927466384,-5.89867160746928,
-20.5890376615871));
#51107=CARTESIAN_POINT('Ctrl Pts',(-6.99999923547135,-5.8746091259089,-20.5367085252783));
#51108=CARTESIAN_POINT('Ctrl Pts',(-6.9999992158751,-5.86257788512872,-20.5105439571239));
#51109=CARTESIAN_POINT('Ctrl Pts',(-6.99999919867913,-5.85066147332808,
-20.4843581721434));
#51110=CARTESIAN_POINT('Ctrl Pts',(-6.99999918389319,-5.83885960187496,
-20.4581522577767));
#51111=CARTESIAN_POINT('Ctrl Pts',(-6.99999917282788,-5.8300274615195,-20.4385405957831));
#51112=CARTESIAN_POINT('Ctrl Pts',(-6.99999916268463,-5.82084773603849,
-20.4179924260146));
#51113=CARTESIAN_POINT('Ctrl Pts',(-6.99999915445597,-5.81224570769022,
-20.3985849979498));
#51114=CARTESIAN_POINT('Ctrl Pts',(-6.99999915168916,-5.80935334977234,
-20.3920594174755));
#51115=CARTESIAN_POINT('Ctrl Pts',(-6.99999914912877,-5.80652589333689,
-20.3856629904652));
#51116=CARTESIAN_POINT('Ctrl Pts',(-6.99999914678332,-5.80379731854171,
-20.3794752090212));
#51117=CARTESIAN_POINT('Ctrl Pts',(-6.99999907528831,-5.72062372100036,
-20.1908565776373));
#51118=CARTESIAN_POINT('Ctrl Pts',(-6.99999912491173,-5.64168485177726,
-19.9974675568945));
#51119=CARTESIAN_POINT('Ctrl Pts',(-6.99999933315401,-5.56752053115335,
-19.799448619423));
#51120=CARTESIAN_POINT('Ctrl Pts',(-6.99999947285253,-5.51776768741775,
-19.6666083915368));
#51121=CARTESIAN_POINT('Ctrl Pts',(-6.99999968442923,-5.47016412906179,
-19.5316853935006));
#51122=CARTESIAN_POINT('Ctrl Pts',(-6.99999998816759,-5.42488006699747,
-19.3947330698664));
#51123=CARTESIAN_POINT('Ctrl Pts',(-7.00000042904109,-5.35915065807392,
-19.1959480034915));
#51124=CARTESIAN_POINT('Ctrl Pts',(-7.00000106781889,-5.29830713940259,
-18.9928852940146));
#51125=CARTESIAN_POINT('Ctrl Pts',(-7.0000015333283,-5.24286447796379,-18.7857677797069));
#51126=CARTESIAN_POINT('Ctrl Pts',(-7.00000199136861,-5.18831139407053,
-18.581973466076));
#51127=CARTESIAN_POINT('Ctrl Pts',(-7.00000228134199,-5.13898725835631,
-18.374253365063));
#51128=CARTESIAN_POINT('Ctrl Pts',(-7.00000202664206,-5.09540487226898,
-18.1628646067693));
#51129=CARTESIAN_POINT('Ctrl Pts',(-7.00000181210231,-5.05869440086198,
-17.9848068714367));
#51130=CARTESIAN_POINT('Ctrl Pts',(-7.0000012106348,-5.02605811693811,-17.8041468995805));
#51131=CARTESIAN_POINT('Ctrl Pts',(-6.99999998662388,-4.99781498742711,
-17.621064245929));
#51132=CARTESIAN_POINT('Ctrl Pts',(-6.99999852879686,-4.96417672770832,
-17.4030083165697));
#51133=CARTESIAN_POINT('Ctrl Pts',(-6.99999617281986,-4.93677080969977,
-17.1815144133228));
#51134=CARTESIAN_POINT('Ctrl Pts',(-6.99999449839166,-4.91605443570459,
-16.9569257573727));
#51135=CARTESIAN_POINT('Ctrl Pts',(-6.99999284818615,-4.89563774996922,
-16.735586057224));
#51136=CARTESIAN_POINT('Ctrl Pts',(-6.99999186150181,-4.88171848710305,
-16.5112404439615));
#51137=CARTESIAN_POINT('Ctrl Pts',(-6.99999320063151,-4.87474450353124,
-16.2842667780983));
#51138=CARTESIAN_POINT('Ctrl Pts',(-6.99999413392965,-4.86988402894972,
-16.1260788898933));
#51139=CARTESIAN_POINT('Ctrl Pts',(-6.9999962001064,-4.86839730041592,-15.9666154928942));
#51140=CARTESIAN_POINT('Ctrl Pts',(-6.9999999996549,-4.87043884390324,-15.8060192338875));
#51141=CARTESIAN_POINT('Ctrl Pts',(-7.00000506889263,-4.87316260680444,
-15.5917567726317));
#51142=CARTESIAN_POINT('Ctrl Pts',(-7.00001329864277,-4.88216671047696,
-15.3754753996994));
#51143=CARTESIAN_POINT('Ctrl Pts',(-7.00001657746181,-4.89779557086446,
-15.1576383695357));
#51144=CARTESIAN_POINT('Ctrl Pts',(-7.00001838122561,-4.90639341427219,
-15.0378005421243));
#51145=CARTESIAN_POINT('Ctrl Pts',(-7.00001867170191,-4.91699624108351,
-14.917492806888));
#51146=CARTESIAN_POINT('Ctrl Pts',(-7.00001598754129,-4.92966193716263,
-14.7967990229923));
#51147=CARTESIAN_POINT('Origin',(-5.9999949808,-9.33250914740362,-24.7867195890602));
#51148=CARTESIAN_POINT('Origin',(-6.,-9.33251101143268,-24.7867243677925));
#51149=CARTESIAN_POINT('Ctrl Pts',(-7.10572058681599,-7.15917451980105,
-14.3583562946813));
#51150=CARTESIAN_POINT('Ctrl Pts',(-7.10645540380474,-7.20568112961659,
-14.3348966367294));
#51151=CARTESIAN_POINT('Ctrl Pts',(-7.10076650948181,-7.33448368577117,
-14.271997245283));
#51152=CARTESIAN_POINT('Ctrl Pts',(-7.05594826294389,-7.55240332663308,
-14.1748898295926));
#51153=CARTESIAN_POINT('Ctrl Pts',(-6.95114004312909,-7.80056170268336,
-14.0785538117247));
#51154=CARTESIAN_POINT('Ctrl Pts',(-6.79944482822535,-8.0256849068933,-14.0064757496486));
#51155=CARTESIAN_POINT('Ctrl Pts',(-6.6208277696206,-8.20816691621563,-13.9635191964736));
#51156=CARTESIAN_POINT('Ctrl Pts',(-6.43625208840588,-8.34296075927564,
-13.94674598393));
#51157=CARTESIAN_POINT('Ctrl Pts',(-6.30967320710823,-8.40903533450593,
-13.9489256328214));
#51158=CARTESIAN_POINT('Ctrl Pts',(-6.24787426415866,-8.43565318561558,
-13.9529403897452));
#51159=CARTESIAN_POINT('Ctrl Pts',(-6.24577684234737,-8.4365502147327,-13.9530799785798));
#51160=CARTESIAN_POINT('Ctrl Pts',(-6.81553757384515,-6.90211824706944,
-13.8389932456361));
#51161=CARTESIAN_POINT('Ctrl Pts',(-6.81619657719427,-6.94305640662117,
-13.8183320344138));
#51162=CARTESIAN_POINT('Ctrl Pts',(-6.81109453262395,-7.0566538750647,-13.7629367837621));
#51163=CARTESIAN_POINT('Ctrl Pts',(-6.77074846063708,-7.2494690894213,-13.6776278902152));
#51164=CARTESIAN_POINT('Ctrl Pts',(-6.67638498400727,-7.4692644419055,-13.5936470267869));
#51165=CARTESIAN_POINT('Ctrl Pts',(-6.5401230543666,-7.6684107429182,-13.5316591804317));
#51166=CARTESIAN_POINT('Ctrl Pts',(-6.38028567734501,-7.82939787216426,
-13.4955946842181));
#51167=CARTESIAN_POINT('Ctrl Pts',(-6.21586083447959,-7.94790647752958,
-13.4824388050648));
#51168=CARTESIAN_POINT('Ctrl Pts',(-6.10363915270979,-8.00579354685784,
-13.4852140513868));
#51169=CARTESIAN_POINT('Ctrl Pts',(-6.04899678238557,-8.02908142810832,
-13.4890768959804));
#51170=CARTESIAN_POINT('Ctrl Pts',(-6.04714241757874,-8.02986619471148,
-13.4892108277678));
#51171=CARTESIAN_POINT('Ctrl Pts',(-7.05965280425926,-6.62889424957639,
-13.3045937670833));
#51172=CARTESIAN_POINT('Ctrl Pts',(-7.060521616384,-6.68192398646321,-13.2778453838265));
#51173=CARTESIAN_POINT('Ctrl Pts',(-7.05379562531041,-6.82834107794673,
-13.2063351599417));
#51174=CARTESIAN_POINT('Ctrl Pts',(-7.00126479150212,-7.07498363172971,
-13.0963249144846));
#51175=CARTESIAN_POINT('Ctrl Pts',(-6.87846148914097,-7.35614255519393,
-12.9869832809918));
#51176=CARTESIAN_POINT('Ctrl Pts',(-6.69976369750449,-7.6127989981063,-12.9046724354872));
#51177=CARTESIAN_POINT('Ctrl Pts',(-6.48751180965009,-7.82290039043415,
-12.8552879569376));
#51178=CARTESIAN_POINT('Ctrl Pts',(-6.26592339562598,-7.97997497096265,
-12.8360886525733));
#51179=CARTESIAN_POINT('Ctrl Pts',(-6.11233174024832,-8.05802853807378,
-12.8390651949399));
#51180=CARTESIAN_POINT('Ctrl Pts',(-6.03689908271419,-8.08970313051234,
-12.8440931022415));
#51181=CARTESIAN_POINT('Ctrl Pts',(-6.03433843459531,-8.0907708844276,-12.8442677853705));
#51182=CARTESIAN_POINT('Ctrl Pts',(-7.67146636779035,-6.52533423325674,
-13.1186084728563));
#51183=CARTESIAN_POINT('Ctrl Pts',(-7.67268761324267,-6.59987309890137,
-13.0810367414559));
#51184=CARTESIAN_POINT('Ctrl Pts',(-7.66323370103255,-6.80476224377587,
-12.9807776285539));
#51185=CARTESIAN_POINT('Ctrl Pts',(-7.59016592525227,-7.14747102909554,
-12.8264048102834));
#51186=CARTESIAN_POINT('Ctrl Pts',(-7.41942193955388,-7.53789024560707,
-12.6712749171081));
#51187=CARTESIAN_POINT('Ctrl Pts',(-7.16934195304591,-7.89634143968295,
-12.5520822507266));
#51188=CARTESIAN_POINT('Ctrl Pts',(-6.86920496992593,-8.19268769913783,
-12.4782464203487));
#51189=CARTESIAN_POINT('Ctrl Pts',(-6.55209859046718,-8.41689177268628,
-12.447463467991));
#51190=CARTESIAN_POINT('Ctrl Pts',(-6.32960538007574,-8.52972012494187,
-12.4501105372351));
#51191=CARTESIAN_POINT('Ctrl Pts',(-6.2196050747502,-8.57578171275077,-12.4568267120036));
#51192=CARTESIAN_POINT('Ctrl Pts',(-6.2158701662133,-8.57733481926968,-12.4570607901429));
#51193=CARTESIAN_POINT('',(-6.26383832463082,-8.42072097704164,-13.9442592301454));
#51194=CARTESIAN_POINT('',(-6.24991285392751,-8.55170704998985,-12.4626562658216));
#51195=CARTESIAN_POINT('Origin',(-6.527651908718,-9.09524965967693,-13.2547563604596));
#51196=CARTESIAN_POINT('',(-6.99999988440685,-8.04449912265075,-12.5220505110564));
#51197=CARTESIAN_POINT('Ctrl Pts',(-6.99999985665133,-8.04449905185795,
-12.5220503391613));
#51198=CARTESIAN_POINT('Ctrl Pts',(-6.96289538607134,-8.08112540801169,
-12.5129574216944));
#51199=CARTESIAN_POINT('Ctrl Pts',(-6.92537693594424,-8.11580955524739,
-12.5049945056296));
#51200=CARTESIAN_POINT('Ctrl Pts',(-6.88761335220619,-8.14868195423147,
-12.4980582408632));
#51201=CARTESIAN_POINT('Ctrl Pts',(-6.87240071834141,-8.16192422947395,
-12.4952640448194));
#51202=CARTESIAN_POINT('Ctrl Pts',(-6.85714770636048,-8.17487251418294,
-12.4926365701431));
#51203=CARTESIAN_POINT('Ctrl Pts',(-6.84186306168057,-8.1875353341046,-12.4901695537855));
#51204=CARTESIAN_POINT('Ctrl Pts',(-6.81126970633746,-8.2128809118149,-12.4852316367028));
#51205=CARTESIAN_POINT('Ctrl Pts',(-6.78055089186904,-8.23708299873428,
-12.4809361823432));
#51206=CARTESIAN_POINT('Ctrl Pts',(-6.74977181316329,-8.26021088679133,
-12.4772329615929));
#51207=CARTESIAN_POINT('Ctrl Pts',(-6.70541234527646,-8.2935432947352,-12.4718958004802));
#51208=CARTESIAN_POINT('Ctrl Pts',(-6.66093157460354,-8.32464562527117,
-12.4677866114349));
#51209=CARTESIAN_POINT('Ctrl Pts',(-6.61657594962318,-8.35365273204861,
-12.464775146045));
#51210=CARTESIAN_POINT('Ctrl Pts',(-6.58742401213129,-8.37271713174924,
-12.4627959145305));
#51211=CARTESIAN_POINT('Ctrl Pts',(-6.55832498198079,-8.3908767719984,-12.4612909391321));
#51212=CARTESIAN_POINT('Ctrl Pts',(-6.52933699125688,-8.40817228213706,
-12.4602244920139));
#51213=CARTESIAN_POINT('Ctrl Pts',(-6.51858346639462,-8.41458830800284,
-12.4598288776469));
#51214=CARTESIAN_POINT('Ctrl Pts',(-6.50784513713682,-8.42088543195715,
-12.4594936210241));
#51215=CARTESIAN_POINT('Ctrl Pts',(-6.49712495711951,-8.42706586839688,
-12.4592167863404));
#51216=CARTESIAN_POINT('Ctrl Pts',(-6.45533111070439,-8.45116100587812,
-12.4581375147016));
#51217=CARTESIAN_POINT('Ctrl Pts',(-6.41381168142764,-8.47347393917319,
-12.4579532736844));
#51218=CARTESIAN_POINT('Ctrl Pts',(-6.37260897169576,-8.49418774960732,
-12.4585576701757));
#51219=CARTESIAN_POINT('Ctrl Pts',(-6.33140626196388,-8.51490156004145,
-12.459162066667));
#51220=CARTESIAN_POINT('Ctrl Pts',(-6.29051957134565,-8.53401642514046,
-12.4605551619981));
#51221=CARTESIAN_POINT('Ctrl Pts',(-6.24994618220503,-8.5516924285248,-12.4626545731639));
#51222=CARTESIAN_POINT('',(-7.000009545786,-6.97711952667737,-13.9487142983806));
#51223=CARTESIAN_POINT('Ctrl Pts',(-7.000009545786,-6.97711952667737,-13.9487142983806));
#51224=CARTESIAN_POINT('Ctrl Pts',(-7.,-7.01445409933478,-13.8623191189325));
#51225=CARTESIAN_POINT('Ctrl Pts',(-7.,-7.07990718347488,-13.7190290853873));
#51226=CARTESIAN_POINT('Ctrl Pts',(-7.,-7.14556603609682,-13.589566730198));
#51227=CARTESIAN_POINT('Ctrl Pts',(-7.,-7.18313577273348,-13.518974611728));
#51228=CARTESIAN_POINT('Ctrl Pts',(-7.,-7.1919711816871,-13.5026286632352));
#51229=CARTESIAN_POINT('Ctrl Pts',(-7.,-7.28162969860235,-13.3396969995268));
#51230=CARTESIAN_POINT('Ctrl Pts',(-7.,-7.36735477671998,-13.2056608545378));
#51231=CARTESIAN_POINT('Ctrl Pts',(-7.,-7.63341057490925,-12.8482930275621));
#51232=CARTESIAN_POINT('Ctrl Pts',(-7.,-7.82956349063113,-12.660130291256));
#51233=CARTESIAN_POINT('Ctrl Pts',(-6.999999792337,-8.04449878994872,-12.5220500366276));
#51234=CARTESIAN_POINT('Ctrl Pts',(-7.00001601661457,-6.97711952672703,
-13.9487142980922));
#51235=CARTESIAN_POINT('Ctrl Pts',(-7.00001543846632,-7.01692337104545,
-13.9425963489463));
#51236=CARTESIAN_POINT('Ctrl Pts',(-6.99868096797267,-7.05610076819487,
-13.9368182972979));
#51237=CARTESIAN_POINT('Ctrl Pts',(-6.99616776089911,-7.09452829561729,
-13.9314343716914));
#51238=CARTESIAN_POINT('Ctrl Pts',(-6.99356689649137,-7.13429612430183,
-13.9258626618902));
#51239=CARTESIAN_POINT('Ctrl Pts',(-6.9897046355072,-7.17326074439687,-13.9207129642798));
#51240=CARTESIAN_POINT('Ctrl Pts',(-6.98475617023165,-7.21131869021076,
-13.9160002389077));
#51241=CARTESIAN_POINT('Ctrl Pts',(-6.9797033920153,-7.25017889208334,-13.9111881699584));
#51242=CARTESIAN_POINT('Ctrl Pts',(-6.97351904010826,-7.28809395023687,
-13.9068312712364));
#51243=CARTESIAN_POINT('Ctrl Pts',(-6.9663780349945,-7.32498745762988,-13.9029032827295));
#51244=CARTESIAN_POINT('Ctrl Pts',(-6.95898554961068,-7.36318022038742,
-13.8988369647304));
#51245=CARTESIAN_POINT('Ctrl Pts',(-6.95056864272973,-7.40027848783653,
-13.8952297705182));
#51246=CARTESIAN_POINT('Ctrl Pts',(-6.94129566725109,-7.43623003030209,
-13.8920150836015));
#51247=CARTESIAN_POINT('Ctrl Pts',(-6.93784226353682,-7.44961895714337,
-13.8908178830089));
#51248=CARTESIAN_POINT('Ctrl Pts',(-6.93426982004788,-7.46284913304693,
-13.8896747998003));
#51249=CARTESIAN_POINT('Ctrl Pts',(-6.93058586859352,-7.47591881634163,
-13.8885813742623));
#51250=CARTESIAN_POINT('Ctrl Pts',(-6.91970525354453,-7.51452035452792,
-13.8853519228128));
#51251=CARTESIAN_POINT('Ctrl Pts',(-6.90786941662626,-7.55171553530684,
-13.8826092506353));
#51252=CARTESIAN_POINT('Ctrl Pts',(-6.89530214052475,-7.58746826104597,
-13.8803240339689));
#51253=CARTESIAN_POINT('Ctrl Pts',(-6.88388401452961,-7.6199517621533,-13.8782477772198));
#51254=CARTESIAN_POINT('Ctrl Pts',(-6.87186213916831,-7.65124527796107,
-13.8765482707761));
#51255=CARTESIAN_POINT('Ctrl Pts',(-6.859384598782,-7.68134460616923,-13.8751816781369));
#51256=CARTESIAN_POINT('Ctrl Pts',(-6.84627917222293,-7.7129585719907,-13.8737463167664));
#51257=CARTESIAN_POINT('Ctrl Pts',(-6.83267337671324,-7.74325449253608,
-13.8726829358396));
#51258=CARTESIAN_POINT('Ctrl Pts',(-6.81872866685287,-7.77224538414329,
-13.8719470606914));
#51259=CARTESIAN_POINT('Ctrl Pts',(-6.81175631192269,-7.78674082994689,
-13.8715791231173));
#51260=CARTESIAN_POINT('Ctrl Pts',(-6.80469903051961,-7.80091023832986,
-13.8712930411406));
#51261=CARTESIAN_POINT('Ctrl Pts',(-6.79757576494785,-7.81475652551018,
-13.871083086116));
#51262=CARTESIAN_POINT('Ctrl Pts',(-6.79401413216197,-7.82167966910034,
-13.8709781086038));
#51263=CARTESIAN_POINT('Ctrl Pts',(-6.79043600023178,-7.82852203040168,
-13.8708921649966));
#51264=CARTESIAN_POINT('Ctrl Pts',(-6.78684364094681,-7.83528407274267,
-13.8708245202887));
#51265=CARTESIAN_POINT('Ctrl Pts',(-6.7844031629649,-7.83987788258651,-13.8707785656925));
#51266=CARTESIAN_POINT('Ctrl Pts',(-6.78226604253571,-7.84386068729018,
-13.8707466372644));
#51267=CARTESIAN_POINT('Ctrl Pts',(-6.77980273810643,-7.84840303797618,
-13.8707160597476));
#51268=CARTESIAN_POINT('Ctrl Pts',(-6.77864008294754,-7.8505469822633,-13.8707016274642));
#51269=CARTESIAN_POINT('Ctrl Pts',(-6.77740428166745,-7.85281534857401,
-13.870687857321));
#51270=CARTESIAN_POINT('Ctrl Pts',(-6.77602613363967,-7.85532970183153,
-13.8706757544928));
#51271=CARTESIAN_POINT('Ctrl Pts',(-6.75125394113064,-7.90052516826551,
-13.8704582063179));
#51272=CARTESIAN_POINT('Ctrl Pts',(-6.72490412475708,-7.94384710910138,
-13.8710746067399));
#51273=CARTESIAN_POINT('Ctrl Pts',(-6.69725567797657,-7.98518156062326,
-13.8725531445371));
#51274=CARTESIAN_POINT('Ctrl Pts',(-6.66792060847387,-8.02903751455356,
-13.8741218767479));
#51275=CARTESIAN_POINT('Ctrl Pts',(-6.63712435813431,-8.07065602654574,
-13.8766608669807));
#51276=CARTESIAN_POINT('Ctrl Pts',(-6.60519224452536,-8.10994500446146,
-13.8801627385162));
#51277=CARTESIAN_POINT('Ctrl Pts',(-6.57239250576793,-8.15030150035343,
-13.8837597591497));
#51278=CARTESIAN_POINT('Ctrl Pts',(-6.53839480749624,-8.18820041717145,
-13.8883721273538));
#51279=CARTESIAN_POINT('Ctrl Pts',(-6.50353422891246,-8.22358513606488,
-13.8939568293774));
#51280=CARTESIAN_POINT('Ctrl Pts',(-6.46687694718795,-8.26079357212403,
-13.8998293651684));
#51281=CARTESIAN_POINT('Ctrl Pts',(-6.42926589159602,-8.29522210847277,
-13.906776585492));
#51282=CARTESIAN_POINT('Ctrl Pts',(-6.39106504384856,-8.32684898034795,
-13.9147183184548));
#51283=CARTESIAN_POINT('Ctrl Pts',(-6.35949181868436,-8.35298877581938,
-13.9212822074209));
#51284=CARTESIAN_POINT('Ctrl Pts',(-6.32751518914135,-8.37721562678356,
-13.9285247897248));
#51285=CARTESIAN_POINT('Ctrl Pts',(-6.29532684358237,-8.39953711567565,
-13.9363895287864));
#51286=CARTESIAN_POINT('Ctrl Pts',(-6.28485853259168,-8.40679652225402,
-13.9389473034383));
#51287=CARTESIAN_POINT('Ctrl Pts',(-6.27436773210387,-8.41385453303562,
-13.9415708157395));
#51288=CARTESIAN_POINT('Ctrl Pts',(-6.2638607595696,-8.42071177891138,-13.9442579405079));
#51289=CARTESIAN_POINT('Ctrl Pts',(-6.22267017867758,-7.49367493044375,
-13.1134074242241));
#51290=CARTESIAN_POINT('Ctrl Pts',(-6.22400572031555,-7.81349993090739,
-13.3673840000309));
#51291=CARTESIAN_POINT('Ctrl Pts',(-6.22726530830951,-8.61699726505343,
-14.0755228901556));
#51292=CARTESIAN_POINT('Ctrl Pts',(-6.23205383335972,-9.75631816520924,
-15.3875907763663));
#51293=CARTESIAN_POINT('Ctrl Pts',(-6.2357076456412,-10.7961446862802,-17.0892605390954));
#51294=CARTESIAN_POINT('Ctrl Pts',(-6.23759681166444,-11.5416365780555,
-18.9411597533656));
#51295=CARTESIAN_POINT('Ctrl Pts',(-6.23804400737905,-11.9701361487446,
-20.8893389967195));
#51296=CARTESIAN_POINT('Ctrl Pts',(-6.23649715758559,-12.0627637107556,
-22.726022856573));
#51297=CARTESIAN_POINT('Ctrl Pts',(-6.23490937071487,-11.9504775464553,
-23.8924618957293));
#51298=CARTESIAN_POINT('Ctrl Pts',(-6.23413407861479,-11.8700328552509,
-24.3933786980252));
#51299=CARTESIAN_POINT('Ctrl Pts',(-6.71589117748943,-7.42368469516801,
-13.2016814708845));
#51300=CARTESIAN_POINT('Ctrl Pts',(-6.71707990387349,-7.74006673352331,
-13.4537919778345));
#51301=CARTESIAN_POINT('Ctrl Pts',(-6.71993443015081,-8.53486089184209,
-14.1564716232462));
#51302=CARTESIAN_POINT('Ctrl Pts',(-6.72416527772874,-9.6612568988981,-15.4574021509406));
#51303=CARTESIAN_POINT('Ctrl Pts',(-6.72736893457949,-10.6891558328984,
-17.1431718671125));
#51304=CARTESIAN_POINT('Ctrl Pts',(-6.72902498583597,-11.4262572324651,
-18.976798290278));
#51305=CARTESIAN_POINT('Ctrl Pts',(-6.72941998203574,-11.8502291076773,
-20.9054815431427));
#51306=CARTESIAN_POINT('Ctrl Pts',(-6.72805245035654,-11.9427115601072,
-22.7235295090814));
#51307=CARTESIAN_POINT('Ctrl Pts',(-6.72668417717144,-11.8323436962498,
-23.8785261271082));
#51308=CARTESIAN_POINT('Ctrl Pts',(-6.72599103236445,-11.7530854106976,
-24.3745537247135));
#51309=CARTESIAN_POINT('Ctrl Pts',(-7.02184860947709,-7.17355734656295,
-13.5171494444303));
#51310=CARTESIAN_POINT('Ctrl Pts',(-7.02249156717522,-7.47887520271202,
-13.7610265541486));
#51311=CARTESIAN_POINT('Ctrl Pts',(-7.02397822748931,-8.24599816030359,
-14.4407082883408));
#51312=CARTESIAN_POINT('Ctrl Pts',(-7.02622826305931,-9.33267501545243,
-15.6982405691599));
#51313=CARTESIAN_POINT('Ctrl Pts',(-7.02790160720142,-10.3242144174604,
-17.326828018892));
#51314=CARTESIAN_POINT('Ctrl Pts',(-7.02876614498039,-11.0353387540962,
-19.0974438565416));
#51315=CARTESIAN_POINT('Ctrl Pts',(-7.02897606416112,-11.4446315866814,
-20.9601358899923));
#51316=CARTESIAN_POINT('Ctrl Pts',(-7.02824776303995,-11.5344312606834,
-22.715199240432));
#51317=CARTESIAN_POINT('Ctrl Pts',(-7.02756281917417,-11.4283599706227,
-23.8309174048354));
#51318=CARTESIAN_POINT('Ctrl Pts',(-7.02718413556234,-11.3520773735171,
-24.3100040140441));
#51319=CARTESIAN_POINT('Ctrl Pts',(-6.99898915817327,-6.85988136608093,
-13.9127665215165));
#51320=CARTESIAN_POINT('Ctrl Pts',(-6.99894180086011,-7.15167011659703,
-14.1458817646929));
#51321=CARTESIAN_POINT('Ctrl Pts',(-6.99873531791728,-7.88504935784626,
-14.7957491612715));
#51322=CARTESIAN_POINT('Ctrl Pts',(-6.99850468722686,-8.92372185170608,
-15.9978535584084));
#51323=CARTESIAN_POINT('Ctrl Pts',(-6.99828080837736,-9.87141300061994,
-17.5546303803054));
#51324=CARTESIAN_POINT('Ctrl Pts',(-6.9981643412379,-10.5510791282796,-19.2468664456477));
#51325=CARTESIAN_POINT('Ctrl Pts',(-6.99814257227861,-10.9423826236159,
-21.0278289503835));
#51326=CARTESIAN_POINT('Ctrl Pts',(-6.99821545942191,-11.0282139102074,
-22.7049145045068));
#51327=CARTESIAN_POINT('Ctrl Pts',(-6.99835922294982,-10.9268166228346,
-23.7718253449984));
#51328=CARTESIAN_POINT('Ctrl Pts',(-6.99838072371096,-10.8539128981486,
-24.2298152697073));
#51329=CARTESIAN_POINT('',(-7.00000355772223,-10.9277699390017,-24.1259406808672));
#51330=CARTESIAN_POINT('Ctrl Pts',(-7.00001601661457,-6.97711952672703,
-13.9487142980922));
#51331=CARTESIAN_POINT('Ctrl Pts',(-7.00002088999339,-7.14852816441581,
-14.0875641829895));
#51332=CARTESIAN_POINT('Ctrl Pts',(-7.0000159830912,-7.3142134747507,-14.2303294324432));
#51333=CARTESIAN_POINT('Ctrl Pts',(-7.00000988157515,-7.47407280375667,
-14.3764170928589));
#51334=CARTESIAN_POINT('Ctrl Pts',(-7.00000652467619,-7.56202334106749,
-14.4567908083494));
#51335=CARTESIAN_POINT('Ctrl Pts',(-7.00000279094438,-7.64821100818324,
-14.5381709027261));
#51336=CARTESIAN_POINT('Ctrl Pts',(-6.99999999965531,-7.73262304327109,
-14.6204637380433));
#51337=CARTESIAN_POINT('Ctrl Pts',(-6.99999455422802,-7.89729950162332,
-14.7810059243999));
#51338=CARTESIAN_POINT('Ctrl Pts',(-6.99999266081079,-8.05521661797847,
-14.9450193659817));
#51339=CARTESIAN_POINT('Ctrl Pts',(-6.99999257345288,-8.20640348779146,
-15.1118936930631));
#51340=CARTESIAN_POINT('Ctrl Pts',(-6.99999248483003,-8.35977953074498,
-15.281184346345));
#51341=CARTESIAN_POINT('Ctrl Pts',(-6.99999425319322,-8.50622906277903,
-15.4534193548216));
#51342=CARTESIAN_POINT('Ctrl Pts',(-6.99999619757759,-8.6458124013378,-15.6280063527474));
#51343=CARTESIAN_POINT('Ctrl Pts',(-6.99999754424624,-8.74248696251648,
-15.7489242329634));
#51344=CARTESIAN_POINT('Ctrl Pts',(-6.99999897835358,-8.83586853326925,
-15.8709712717052));
#51345=CARTESIAN_POINT('Ctrl Pts',(-6.99999998662288,-8.92598514844779,
-15.9939628974921));
#51346=CARTESIAN_POINT('Ctrl Pts',(-7.00000143709196,-9.05562448575202,
-16.1708953402985));
#51347=CARTESIAN_POINT('Ctrl Pts',(-7.00000201442316,-9.17850663798034,
-16.3497801253261));
#51348=CARTESIAN_POINT('Ctrl Pts',(-7.00000210876032,-9.29479658368068,
-16.5300359468127));
#51349=CARTESIAN_POINT('Ctrl Pts',(-7.00000220461162,-9.4129530146951,-16.7131849233487));
#51350=CARTESIAN_POINT('Ctrl Pts',(-7.00000180217023,-9.52430397773151,
-16.8977493304543));
#51351=CARTESIAN_POINT('Ctrl Pts',(-7.00000129011944,-9.6290403473303,-17.0831707166954));
#51352=CARTESIAN_POINT('Ctrl Pts',(-7.00000086167034,-9.71667658275699,
-17.2383186592871));
#51353=CARTESIAN_POINT('Ctrl Pts',(-7.00000035619251,-9.79968215285438,
-17.3940675430476));
#51354=CARTESIAN_POINT('Ctrl Pts',(-6.9999999881668,-9.87817778643373,-17.5501167577466));
#51355=CARTESIAN_POINT('Ctrl Pts',(-6.99999970373346,-9.93884413335317,
-17.6707213743825));
#51356=CARTESIAN_POINT('Ctrl Pts',(-6.99999950019769,-9.99681685740602,
-17.7915058719012));
#51357=CARTESIAN_POINT('Ctrl Pts',(-6.99999936067301,-10.0521635852022,
-17.9123403180643));
#51358=CARTESIAN_POINT('Ctrl Pts',(-6.99999924478733,-10.0981331762724,
-18.0127023502653));
#51359=CARTESIAN_POINT('Ctrl Pts',(-6.99999917321297,-10.1422912472031,
-18.1130989925497));
#51360=CARTESIAN_POINT('Ctrl Pts',(-6.99999913936348,-10.1846774398662,
-18.2134600445155));
#51361=CARTESIAN_POINT('Ctrl Pts',(-6.99999912243874,-10.2058705361977,
-18.2636405704984));
#51362=CARTESIAN_POINT('Ctrl Pts',(-6.99999911498655,-10.2266206629623,
-18.3138121989017));
#51363=CARTESIAN_POINT('Ctrl Pts',(-6.99999911639989,-10.2469328611172,
-18.3639665749347));
#51364=CARTESIAN_POINT('Ctrl Pts',(-6.99999911710655,-10.2570889601946,
-18.3890437629512));
#51365=CARTESIAN_POINT('Ctrl Pts',(-6.9999991200318,-10.2671355771195,-18.4141166378752));
#51366=CARTESIAN_POINT('Ctrl Pts',(-6.99999912511194,-10.2770733440966,
-18.4391841663968));
#51367=CARTESIAN_POINT('Ctrl Pts',(-6.99999912765202,-10.2820422275851,
-18.4517179306576));
#51368=CARTESIAN_POINT('Ctrl Pts',(-6.99999913073094,-10.2869838985867,
-18.4642503583179));
#51369=CARTESIAN_POINT('Ctrl Pts',(-6.99999913434145,-10.2918984364191,
-18.4767813216805));
#51370=CARTESIAN_POINT('Ctrl Pts',(-6.99999913749775,-10.2961947269233,
-18.4877358937565));
#51371=CARTESIAN_POINT('Ctrl Pts',(-6.99999914056827,-10.2999248799151,
-18.4972872811118));
#51372=CARTESIAN_POINT('Ctrl Pts',(-6.99999914483355,-10.3045195397806,
-18.5091123716368));
#51373=CARTESIAN_POINT('Ctrl Pts',(-6.99999914544734,-10.3051807232324,
-18.5108140327825));
#51374=CARTESIAN_POINT('Ctrl Pts',(-6.99999914608781,-10.3058597282213,
-18.5125628090823));
#51375=CARTESIAN_POINT('Ctrl Pts',(-6.9999991467609,-10.3065607298115,-18.5143696916144));
#51376=CARTESIAN_POINT('Ctrl Pts',(-6.99999923697261,-10.4005127250538,
-18.756537785691));
#51377=CARTESIAN_POINT('Ctrl Pts',(-6.99999952144542,-10.4851669254592,
-19.0001638726786));
#51378=CARTESIAN_POINT('Ctrl Pts',(-6.99999999018441,-10.5606727034661,
-19.2445345426536));
#51379=CARTESIAN_POINT('Ctrl Pts',(-7.00000044364527,-10.6337174393521,
-19.4809401730273));
#51380=CARTESIAN_POINT('Ctrl Pts',(-7.00000106797182,-10.6982012753055,
-19.7180425300442));
#51381=CARTESIAN_POINT('Ctrl Pts',(-7.00000142593368,-10.7543687395633,
-19.9551823301155));
#51382=CARTESIAN_POINT('Ctrl Pts',(-7.000001787659,-10.8111267256216,-20.194815321282));
#51383=CARTESIAN_POINT('Ctrl Pts',(-7.00000187627587,-10.8593925727004,
-20.4344865835451));
#51384=CARTESIAN_POINT('Ctrl Pts',(-7.00000131559613,-10.899424908229,-20.6735687764459));
#51385=CARTESIAN_POINT('Ctrl Pts',(-7.00000103873707,-10.919192546995,-20.7916256013166));
#51386=CARTESIAN_POINT('Ctrl Pts',(-7.00000060481242,-10.9369527001568,
-20.9095395989653));
#51387=CARTESIAN_POINT('Ctrl Pts',(-6.99999997635826,-10.9527370390027,
-21.0272398759844));
#51388=CARTESIAN_POINT('Ctrl Pts',(-6.99999887928051,-10.9802913904854,
-21.2327064992163));
#51389=CARTESIAN_POINT('Ctrl Pts',(-6.99999719586421,-11.0018248530504,
-21.4375204977235));
#51390=CARTESIAN_POINT('Ctrl Pts',(-6.99999590263484,-11.017557252248,-21.6413538404685));
#51391=CARTESIAN_POINT('Ctrl Pts',(-6.99999568171157,-11.0202448288404,
-21.6761748308222));
#51392=CARTESIAN_POINT('Ctrl Pts',(-6.99999546001773,-11.0229065623117,
-21.7128795454964));
#51393=CARTESIAN_POINT('Ctrl Pts',(-6.99999525388096,-11.0254108578281,
-21.7501378180189));
#51394=CARTESIAN_POINT('Ctrl Pts',(-6.99999512029513,-11.0270337530759,
-21.7742828412477));
#51395=CARTESIAN_POINT('Ctrl Pts',(-6.99999499323631,-11.0285915172457,
-21.7986602431002));
#51396=CARTESIAN_POINT('Ctrl Pts',(-6.99999487630838,-11.0300601234091,
-21.8229071175643));
#51397=CARTESIAN_POINT('Ctrl Pts',(-6.99999457894853,-11.0337949410457,
-21.8845694315598));
#51398=CARTESIAN_POINT('Ctrl Pts',(-6.99999434327763,-11.0369990630641,
-21.9460663067667));
#51399=CARTESIAN_POINT('Ctrl Pts',(-6.99999419420638,-11.0396820529461,
-22.0073884932679));
#51400=CARTESIAN_POINT('Ctrl Pts',(-6.99999365474403,-11.0493913156715,
-22.2293025689177));
#51401=CARTESIAN_POINT('Ctrl Pts',(-6.99999426201427,-11.0522757589082,
-22.4489298924521));
#51402=CARTESIAN_POINT('Ctrl Pts',(-6.99999708881797,-11.0487792584282,
-22.665896946056));
#51403=CARTESIAN_POINT('Ctrl Pts',(-6.99999738657107,-11.0484109647727,
-22.6887505363071));
#51404=CARTESIAN_POINT('Ctrl Pts',(-6.99999770879678,-11.0479718686333,
-22.7115746583192));
#51405=CARTESIAN_POINT('Ctrl Pts',(-6.99999805664087,-11.0474624838517,
-22.734368908558));
#51406=CARTESIAN_POINT('Ctrl Pts',(-6.99999863108936,-11.0466212583313,
-22.7720125636346));
#51407=CARTESIAN_POINT('Ctrl Pts',(-6.99999927541492,-11.0455883348251,
-22.809574746992));
#51408=CARTESIAN_POINT('Ctrl Pts',(-6.99999999465529,-11.0443660217701,
-22.8470536786943));
#51409=CARTESIAN_POINT('Ctrl Pts',(-7.00000393353041,-11.0376721003838,
-23.0523047160112));
#51410=CARTESIAN_POINT('Ctrl Pts',(-7.00001006486665,-11.0252993377964,
-23.2550548353964));
#51411=CARTESIAN_POINT('Ctrl Pts',(-7.00001375755606,-11.0076805209828,
-23.4549602553255));
#51412=CARTESIAN_POINT('Ctrl Pts',(-7.00001750473177,-10.9898017353607,
-23.6578153156528));
#51413=CARTESIAN_POINT('Ctrl Pts',(-7.00001874206597,-10.9665209565483,
-23.8577411890485));
#51414=CARTESIAN_POINT('Ctrl Pts',(-7.00001328550256,-10.9382750849474,
-24.054429846901));
#51415=CARTESIAN_POINT('Ctrl Pts',(-7.00001262289278,-10.9348450889235,
-24.0783144458225));
#51416=CARTESIAN_POINT('Ctrl Pts',(-7.00001186234173,-10.9313418586631,
-24.102151368649));
#51417=CARTESIAN_POINT('Ctrl Pts',(-7.00001099698758,-10.9277661612435,
-24.1259401133012));
#51418=CARTESIAN_POINT('',(-6.271594443024,-11.8794941632625,-24.2690120587724));
#51419=CARTESIAN_POINT('Origin',(-5.99998362344205,-10.9277594519405,-24.1259473036685));
#51420=CARTESIAN_POINT('Ctrl Pts',(-6.26386063113558,-8.42071912122325,
-13.9442659510471));
#51421=CARTESIAN_POINT('Ctrl Pts',(-6.26455155145855,-8.59292897217472,
-14.1129997319506));
#51422=CARTESIAN_POINT('Ctrl Pts',(-6.2652098889244,-8.75835742010234,-14.2852520702197));
#51423=CARTESIAN_POINT('Ctrl Pts',(-6.2658356434991,-8.91700591634091,-14.4604178426464));
#51424=CARTESIAN_POINT('Ctrl Pts',(-6.2664706971121,-9.07801201171459,-14.6381866695197));
#51425=CARTESIAN_POINT('Ctrl Pts',(-6.2670721922411,-9.23203520058945,-14.8189561782818));
#51426=CARTESIAN_POINT('Ctrl Pts',(-6.26764012885049,-9.37910898118983,
-15.0021375673763));
#51427=CARTESIAN_POINT('Ctrl Pts',(-6.26812470388292,-9.50459531333848,
-15.1584316433261));
#51428=CARTESIAN_POINT('Ctrl Pts',(-6.26858484882168,-9.62502315723059,
-15.3164822997201));
#51429=CARTESIAN_POINT('Ctrl Pts',(-6.26902056364464,-9.74043079708379,
-15.4759481443977));
#51430=CARTESIAN_POINT('Ctrl Pts',(-6.26953467308444,-9.87660279295714,
-15.6641053787974));
#51431=CARTESIAN_POINT('Ctrl Pts',(-6.27001477053663,-10.0057860138603,
-15.8542312106714));
#51432=CARTESIAN_POINT('Ctrl Pts',(-6.27046085596489,-10.1281597369355,
-16.0457357401779));
#51433=CARTESIAN_POINT('Ctrl Pts',(-6.27062083627522,-10.1720468154061,
-16.1144153071855));
#51434=CARTESIAN_POINT('Ctrl Pts',(-6.27077644207497,-10.2150582315774,
-16.1832726641688));
#51435=CARTESIAN_POINT('Ctrl Pts',(-6.27092767336246,-10.2572027535103,
-16.2522821457338));
#51436=CARTESIAN_POINT('Ctrl Pts',(-6.27136815356596,-10.3799539904141,
-16.4532809667355));
#51437=CARTESIAN_POINT('Ctrl Pts',(-6.27177152312615,-10.4953497486126,
-16.6555662199662));
#51438=CARTESIAN_POINT('Ctrl Pts',(-6.27213778204303,-10.6036186334423,
-16.8585417460444));
#51439=CARTESIAN_POINT('Ctrl Pts',(-6.2725040409599,-10.711887518272,-17.0615172721226));
#51440=CARTESIAN_POINT('Ctrl Pts',(-6.27283318923347,-10.8130296334295,
-17.265183259542));
#51441=CARTESIAN_POINT('Ctrl Pts',(-6.27312522686372,-10.9072901272152,
-17.4689978455677));
#51442=CARTESIAN_POINT('Ctrl Pts',(-6.27334042001379,-10.9767476576266,
-17.6191822678916));
#51443=CARTESIAN_POINT('Ctrl Pts',(-6.27353526248212,-11.0423478968138,
-17.7691758821825));
#51444=CARTESIAN_POINT('Ctrl Pts',(-6.2737099759448,-11.1043414808216,-17.9190756114325));
#51445=CARTESIAN_POINT('Ctrl Pts',(-6.27388468940749,-11.1663350648294,
-18.0689753406825));
#51446=CARTESIAN_POINT('Ctrl Pts',(-6.27403927386453,-11.2247220378057,
-18.2187816105632));
#51447=CARTESIAN_POINT('Ctrl Pts',(-6.27417395099203,-11.279707421021,-18.368626212332));
#51448=CARTESIAN_POINT('Ctrl Pts',(-6.27427013615269,-11.3189774738988,
-18.4756438430332));
#51449=CARTESIAN_POINT('Ctrl Pts',(-6.27435616721267,-11.3565115886943,
-18.5826817408085));
#51450=CARTESIAN_POINT('Ctrl Pts',(-6.2744321249255,-11.3923814106472,-18.6897928669546));
#51451=CARTESIAN_POINT('Ctrl Pts',(-6.27457884404932,-11.4616671836455,
-18.8966875981714));
#51452=CARTESIAN_POINT('Ctrl Pts',(-6.27469165391534,-11.5261459268611,
-19.1080568290295));
#51453=CARTESIAN_POINT('Ctrl Pts',(-6.27477055452358,-11.5853121282286,
-19.3236963875817));
#51454=CARTESIAN_POINT('Ctrl Pts',(-6.27484862770157,-11.6438578539663,
-19.5370745352639));
#51455=CARTESIAN_POINT('Ctrl Pts',(-6.27489349910493,-11.6972018816246,
-19.7546340252876));
#51456=CARTESIAN_POINT('Ctrl Pts',(-6.27490516873366,-11.7448338103361,
-19.9761311914299));
#51457=CARTESIAN_POINT('Ctrl Pts',(-6.27491664477165,-11.791675559668,-20.1939538791694));
#51458=CARTESIAN_POINT('Ctrl Pts',(-6.27489601148479,-11.8329931384633,
-20.4155847332407));
#51459=CARTESIAN_POINT('Ctrl Pts',(-6.27484326887307,-11.8682812257124,
-20.6407463058143));
#51460=CARTESIAN_POINT('Ctrl Pts',(-6.27479056635055,-11.9035424907943,
-20.8657367350417));
#51461=CARTESIAN_POINT('Ctrl Pts',(-6.27470580329666,-11.9327834609942,
-21.0942526911029));
#51462=CARTESIAN_POINT('Ctrl Pts',(-6.27458897971139,-11.9554797335007,
-21.3259694684535));
#51463=CARTESIAN_POINT('Ctrl Pts',(-6.27454781352703,-11.963477424515,-21.4076216070384));
#51464=CARTESIAN_POINT('Ctrl Pts',(-6.27450266640086,-11.9706622677186,
-21.4896707456406));
#51465=CARTESIAN_POINT('Ctrl Pts',(-6.27445353832076,-11.9770107062944,
-21.5721011963521));
#51466=CARTESIAN_POINT('Ctrl Pts',(-6.27431624074768,-11.9947526006979,
-21.8024684488204));
#51467=CARTESIAN_POINT('Ctrl Pts',(-6.27414785084326,-12.0059621178477,
-22.0358175491883));
#51468=CARTESIAN_POINT('Ctrl Pts',(-6.27394836834336,-12.0102364733222,
-22.271764620327));
#51469=CARTESIAN_POINT('Ctrl Pts',(-6.27375072689948,-12.014471380084,-22.5055340980757));
#51470=CARTESIAN_POINT('Ctrl Pts',(-6.27352256412883,-12.0118985210674,
-22.7418539062483));
#51471=CARTESIAN_POINT('Ctrl Pts',(-6.27326387977453,-12.0021219113766,
-22.9803002635899));
#51472=CARTESIAN_POINT('Ctrl Pts',(-6.27300884338782,-11.9924831714667,
-23.215384049643));
#51473=CARTESIAN_POINT('Ctrl Pts',(-6.27272414017866,-11.9758423964283,
-23.4525348737001));
#51474=CARTESIAN_POINT('Ctrl Pts',(-6.27240976990089,-11.951816352854,-23.6912964437234));
#51475=CARTESIAN_POINT('Ctrl Pts',(-6.27215746684018,-11.932533854605,-23.8829184867648));
#51476=CARTESIAN_POINT('Ctrl Pts',(-6.27188605483419,-11.908494333709,-24.0755771130839));
#51477=CARTESIAN_POINT('Ctrl Pts',(-6.27159553375568,-11.8794980525036,
-24.2690121689631));
#51478=CARTESIAN_POINT('Origin',(-5.999994993365,-10.9277770074801,-24.1259380195517));
#51479=CARTESIAN_POINT('',(-5.98852246669736,-11.3308498388635,-25.0410395151954));
#51480=CARTESIAN_POINT('Origin',(-5.999994993365,-10.9277770074801,-24.1259380195517));
#51481=CARTESIAN_POINT('Origin',(-6.,-10.9277790633915,-24.1259427050578));
#51482=CARTESIAN_POINT('Ctrl Pts',(-5.98841833134383,-11.3313022800093,
-25.0408390134412));
#51483=CARTESIAN_POINT('Ctrl Pts',(-5.98810627250749,-11.2108442555167,
-25.0938945834082));
#51484=CARTESIAN_POINT('Ctrl Pts',(-5.9872640505444,-10.7897532280987,-25.2768814426322));
#51485=CARTESIAN_POINT('Ctrl Pts',(-5.98726405054346,-10.2439465927857,
-25.5029619533741));
#51486=CARTESIAN_POINT('Ctrl Pts',(-5.98810627252732,-9.8167990201698,-25.6713270262117));
#51487=CARTESIAN_POINT('Ctrl Pts',(-5.98841833138136,-9.69410637653267,
-25.7189877605115));
#51488=CARTESIAN_POINT('Ctrl Pts',(-6.58019637611207,-11.334065277118,-25.0471116847692));
#51489=CARTESIAN_POINT('Ctrl Pts',(-6.57988216872294,-11.2136609913595,
-25.1003453887717));
#51490=CARTESIAN_POINT('Ctrl Pts',(-6.57903377743291,-10.7926927015607,
-25.2838224191463));
#51491=CARTESIAN_POINT('Ctrl Pts',(-6.57903377743206,-10.2467760827226,
-25.5099484865553));
#51492=CARTESIAN_POINT('Ctrl Pts',(-6.57988216874175,-9.81936869536461,
-25.6778801674394));
#51493=CARTESIAN_POINT('Ctrl Pts',(-6.58019637614898,-9.69658809095763,
-25.7253769429152));
#51494=CARTESIAN_POINT('Ctrl Pts',(-7.00079677429184,-11.1662377629886,
-24.6661026395446));
#51495=CARTESIAN_POINT('Ctrl Pts',(-7.0006124896366,-11.0471442760462,-24.7189023979519));
#51496=CARTESIAN_POINT('Ctrl Pts',(-7.00011448915241,-10.6307100868985,
-24.9007955995176));
#51497=CARTESIAN_POINT('Ctrl Pts',(-7.00011448915238,-10.0904742265319,
-25.1245686197181));
#51498=CARTESIAN_POINT('Ctrl Pts',(-7.00061248964771,-9.66739286861664,
-25.2904141433636));
#51499=CARTESIAN_POINT('Ctrl Pts',(-7.00079677431298,-9.54584598485692,
-25.3372908899495));
#51500=CARTESIAN_POINT('Ctrl Pts',(-6.99999917318423,-10.9276780868235,
-24.1245144806664));
#51501=CARTESIAN_POINT('Ctrl Pts',(-6.99999957776486,-10.8103725307965,
-24.1765264252412));
#51502=CARTESIAN_POINT('Ctrl Pts',(-7.00000004362129,-10.4001860019773,
-24.3557042159038));
#51503=CARTESIAN_POINT('Ctrl Pts',(-7.0000000436221,-9.86804155661048,-24.576125662278));
#51504=CARTESIAN_POINT('Ctrl Pts',(-6.99999957776511,-9.45129804718398,
-24.7394735083839));
#51505=CARTESIAN_POINT('Ctrl Pts',(-6.99999917318347,-9.33157249006586,
-24.7856430653755));
#51506=CARTESIAN_POINT('Origin',(-5.98852353414945,4.75229019615101,11.4730434493167));
#51507=CARTESIAN_POINT('Origin',(-7.00021006963517,4.74293535319878,11.4504589429759));
#51508=CARTESIAN_POINT('Ctrl Pts',(-6.05505067658424,-11.6467908023141,
-24.9010149462025));
#51509=CARTESIAN_POINT('Ctrl Pts',(-4.03670045105583,-12.172766115143,-24.6398353500469));
#51510=CARTESIAN_POINT('Ctrl Pts',(7.59697248924746E-7,-12.7121382468122,
-24.4085103636044));
#51511=CARTESIAN_POINT('Ctrl Pts',(4.03670197045045,-12.1727659121264,-24.6398354371181));
#51512=CARTESIAN_POINT('Ctrl Pts',(6.05505295567616,-11.6467902083882,-24.9010152411215));
#51513=CARTESIAN_POINT('Ctrl Pts',(-6.05505067658424,-10.8984856531672,
-25.2386153210465));
#51514=CARTESIAN_POINT('Ctrl Pts',(-4.03670045105583,-11.0706898476697,
-25.1429607074797));
#51515=CARTESIAN_POINT('Ctrl Pts',(7.59697248924746E-7,-11.3017449371971,
-25.1800056309795));
#51516=CARTESIAN_POINT('Ctrl Pts',(4.03670197045045,-11.0706897606967,-25.1429606935417));
#51517=CARTESIAN_POINT('Ctrl Pts',(6.05505295567616,-10.8984854587184,-25.2386154290685));
#51518=CARTESIAN_POINT('Ctrl Pts',(-6.05505067658424,-10.1393891149069,
-25.5530359782357));
#51519=CARTESIAN_POINT('Ctrl Pts',(-4.03670045105583,-9.94969139606472,
-25.6072809456058));
#51520=CARTESIAN_POINT('Ctrl Pts',(7.59697248924746E-7,-9.81219809096102,
-25.7969458341962));
#51521=CARTESIAN_POINT('Ctrl Pts',(4.03670197045045,-9.94969144781643,-25.6072808742153));
#51522=CARTESIAN_POINT('Ctrl Pts',(6.05505295567616,-10.1393893291101,-25.5530359169843));
#51523=CARTESIAN_POINT('Ctrl Pts',(-6.05505067658424,-9.37153325114741,
-25.8434352094466));
#51524=CARTESIAN_POINT('Ctrl Pts',(-4.03670045105583,-8.81463489221611,
-26.0307812750284));
#51525=CARTESIAN_POINT('Ctrl Pts',(7.59697248924746E-7,-8.26934125243994,
-26.2486262267072));
#51526=CARTESIAN_POINT('Ctrl Pts',(4.03670197045045,-8.81463509746334,-26.0307811930261));
#51527=CARTESIAN_POINT('Ctrl Pts',(6.05505295567616,-9.37153387998869,-25.8434349978963));
#51528=CARTESIAN_POINT('Ctrl Pts',(-5.98852262888498,-11.3308502499308,
-25.0410393032242));
#51529=CARTESIAN_POINT('Ctrl Pts',(-5.93914474648228,-11.3464662790723,
-25.0335418651297));
#51530=CARTESIAN_POINT('Ctrl Pts',(-5.88279573443552,-11.3641427248077,
-25.025075083296));
#51531=CARTESIAN_POINT('Ctrl Pts',(-5.81940484978196,-11.3837118309506,
-25.0157333886925));
#51532=CARTESIAN_POINT('Ctrl Pts',(-5.75829929351482,-11.4025754439613,
-25.0067284749995));
#51533=CARTESIAN_POINT('Ctrl Pts',(-5.6906501886918,-11.4231976271372,-24.9969107663179));
#51534=CARTESIAN_POINT('Ctrl Pts',(-5.61638362618853,-11.4453877159357,
-24.9863837755093));
#51535=CARTESIAN_POINT('Ctrl Pts',(-5.54072805448531,-11.4679928264674,
-24.9756598981533));
#51536=CARTESIAN_POINT('Ctrl Pts',(-5.45820496082235,-11.4922253843586,
-24.9641999665009));
#51537=CARTESIAN_POINT('Ctrl Pts',(-5.36872850713851,-11.517838641789,-24.9521323326467));
#51538=CARTESIAN_POINT('Ctrl Pts',(-5.32399028029659,-11.5306452705042,
-24.9460985157196));
#51539=CARTESIAN_POINT('Ctrl Pts',(-5.27751361435665,-11.5437963423677,
-24.9399130655401));
#51540=CARTESIAN_POINT('Ctrl Pts',(-5.22928736241266,-11.557256449084,-24.9335937406877));
#51541=CARTESIAN_POINT('Ctrl Pts',(-5.20517423644066,-11.5639865024422,
-24.9304340782615));
#51542=CARTESIAN_POINT('Ctrl Pts',(-5.18062371398836,-11.5707938128604,
-24.9272409434839));
#51543=CARTESIAN_POINT('Ctrl Pts',(-5.15563438617454,-11.5776735871523,
-24.9240166902759));
#51544=CARTESIAN_POINT('Ctrl Pts',(-5.13189984807928,-11.5842079071722,
-24.9209543365718));
#51545=CARTESIAN_POINT('Ctrl Pts',(-5.10666091671902,-11.5911088858746,
-24.917722934394));
#51546=CARTESIAN_POINT('Ctrl Pts',(-5.08307503754699,-11.5975138749284,
-24.9147262027041));
#51547=CARTESIAN_POINT('Ctrl Pts',(-5.08182810707926,-11.5978524917736,
-24.9145677724831));
#51548=CARTESIAN_POINT('Ctrl Pts',(-5.0805858005279,-11.5981897325559,-24.9144099927714));
#51549=CARTESIAN_POINT('Ctrl Pts',(-5.07934858564891,-11.5985254731791,
-24.9142529214491));
#51550=CARTESIAN_POINT('Ctrl Pts',(-5.06433554014817,-11.6025995344745,
-24.9123469316755));
#51551=CARTESIAN_POINT('Ctrl Pts',(-5.04943318285377,-11.6066254144498,
-24.9104644360685));
#51552=CARTESIAN_POINT('Ctrl Pts',(-5.03464184082257,-11.610603820394,-24.9086050215558));
#51553=CARTESIAN_POINT('Ctrl Pts',(-4.91702209136905,-11.6422398348539,
-24.8938190833598));
#51554=CARTESIAN_POINT('Ctrl Pts',(-4.8064247394437,-11.6708766576423,-24.880490587538));
#51555=CARTESIAN_POINT('Ctrl Pts',(-4.70298901342678,-11.6968548640577,
-24.8684336938881));
#51556=CARTESIAN_POINT('Ctrl Pts',(-4.59988945574151,-11.7227486407442,
-24.8564159854017));
#51557=CARTESIAN_POINT('Ctrl Pts',(-4.50390473923413,-11.7460013235489,
-24.8456616465603));
#51558=CARTESIAN_POINT('Ctrl Pts',(-4.41514467568984,-11.7669144905269,
-24.836011384925));
#51559=CARTESIAN_POINT('Ctrl Pts',(-4.38360632213252,-11.7743453871241,
-24.8325824400682));
#51560=CARTESIAN_POINT('Ctrl Pts',(-4.35297986818637,-11.7814805642034,
-24.8292931152813));
#51561=CARTESIAN_POINT('Ctrl Pts',(-4.32326949058923,-11.7883323671655,
-24.8261370134803));
#51562=CARTESIAN_POINT('Ctrl Pts',(-4.28864225633674,-11.7963180948946,
-24.8224585992282));
#51563=CARTESIAN_POINT('Ctrl Pts',(-4.25525940838751,-11.8039189234467,
-24.8189611357159));
#51564=CARTESIAN_POINT('Ctrl Pts',(-4.22312693762557,-11.8111532657858,
-24.8156351724646));
#51565=CARTESIAN_POINT('Ctrl Pts',(-4.2070607022446,-11.8147704369554,-24.8139721908389));
#51566=CARTESIAN_POINT('Ctrl Pts',(-4.19130706116087,-11.8182959875239,
-24.8123520863462));
#51567=CARTESIAN_POINT('Ctrl Pts',(-4.17586669210795,-11.8217320788189,
-24.8107737565214));
#51568=CARTESIAN_POINT('Ctrl Pts',(-4.16814650758149,-11.8234501244665,
-24.8099845916091));
#51569=CARTESIAN_POINT('Ctrl Pts',(-4.16050464106272,-11.8251458053497,
-24.8092058704814));
#51570=CARTESIAN_POINT('Ctrl Pts',(-4.15294117552302,-11.8268193877146,
-24.8084374579634));
#51571=CARTESIAN_POINT('Ctrl Pts',(-4.14915944275316,-11.827656178897,-24.8080532517044));
#51572=CARTESIAN_POINT('Ctrl Pts',(-4.14539731022808,-11.828487445453,-24.8076716226047));
#51573=CARTESIAN_POINT('Ctrl Pts',(-4.14165478808721,-11.8293132201818,
-24.8072925540389));
#51574=CARTESIAN_POINT('Ctrl Pts',(-4.13978352701677,-11.8297261075463,
-24.807103019756));
#51575=CARTESIAN_POINT('Ctrl Pts',(-4.13791716854239,-11.8301376219541,
-24.806914125607));
#51576=CARTESIAN_POINT('Ctrl Pts',(-4.13605571391661,-11.8305477674734,
-24.8067258695314));
#51577=CARTESIAN_POINT('Ctrl Pts',(-4.13419425929082,-11.8309579129926,
-24.8065376134559));
#51578=CARTESIAN_POINT('Ctrl Pts',(-4.13409016851678,-11.8309811013436,
-24.8065269615135));
#51579=CARTESIAN_POINT('Ctrl Pts',(-4.13048606283315,-11.8317741014242,
-24.806163013471));
#51580=CARTESIAN_POINT('Ctrl Pts',(-4.08691193608046,-11.8413615799999,
-24.8017628322536));
#51581=CARTESIAN_POINT('Ctrl Pts',(-4.04447551158591,-11.8505510334919,
-24.7975506165548));
#51582=CARTESIAN_POINT('Ctrl Pts',(-4.00318382527373,-11.859363884762,-24.7935152675936));
#51583=CARTESIAN_POINT('Ctrl Pts',(-3.90005318300528,-11.8813749744723,
-24.7834365285712));
#51584=CARTESIAN_POINT('Ctrl Pts',(-3.80406510876868,-11.9010396405033,
-24.7744594735136));
#51585=CARTESIAN_POINT('Ctrl Pts',(-3.71531264757601,-11.9186665884889,
-24.7664288201101));
#51586=CARTESIAN_POINT('Ctrl Pts',(-3.6270765161079,-11.9361909892655,-24.758444886144));
#51587=CARTESIAN_POINT('Ctrl Pts',(-3.54599178802324,-11.9517014694679,
-24.7513963839144));
#51588=CARTESIAN_POINT('Ctrl Pts',(-3.4721292318734,-11.9654603838603,-24.7451537349961));
#51589=CARTESIAN_POINT('Ctrl Pts',(-3.41383650114598,-11.9763189938731,
-24.7402270025435));
#51590=CARTESIAN_POINT('Ctrl Pts',(-3.36004163248443,-11.986085873297,-24.7358026394847));
#51591=CARTESIAN_POINT('Ctrl Pts',(-3.3107717495728,-11.9948708904099,-24.7318271128458));
#51592=CARTESIAN_POINT('Ctrl Pts',(-3.27749896763286,-12.0008035604602,
-24.7291423727341));
#51593=CARTESIAN_POINT('Ctrl Pts',(-3.24628968207182,-12.0062880984038,
-24.726662511234));
#51594=CARTESIAN_POINT('Ctrl Pts',(-3.21715071542865,-12.0113537837853,
-24.7243733815959));
#51595=CARTESIAN_POINT('Ctrl Pts',(-3.20258123210707,-12.013886626476,-24.7232288167768));
#51596=CARTESIAN_POINT('Ctrl Pts',(-3.18852932852064,-12.0163147568122,
-24.7221319365904));
#51597=CARTESIAN_POINT('Ctrl Pts',(-3.17499573068162,-12.0186414143701,
-24.7210811821799));
#51598=CARTESIAN_POINT('Ctrl Pts',(-3.16822893176211,-12.019804743149,-24.7205558049746));
#51599=CARTESIAN_POINT('Ctrl Pts',(-3.16159170927972,-12.0209427037737,
-24.7200419592991));
#51600=CARTESIAN_POINT('Ctrl Pts',(-3.15508415103286,-12.0220556892655,
-24.7195394565085));
#51601=CARTESIAN_POINT('Ctrl Pts',(-3.15183037190943,-12.0226121820114,
-24.7192882051131));
#51602=CARTESIAN_POINT('Ctrl Pts',(-3.14860900884489,-12.0231624309762,
-24.7190397894436));
#51603=CARTESIAN_POINT('Ctrl Pts',(-3.14542007238591,-12.0237064837776,
-24.7187941866655));
#51604=CARTESIAN_POINT('Ctrl Pts',(-3.14223113592693,-12.024250536579,-24.7185485838875));
#51605=CARTESIAN_POINT('Ctrl Pts',(-3.13737712873962,-12.0250773021456,
-24.7181753876997));
#51606=CARTESIAN_POINT('Ctrl Pts',(-3.13595055324829,-12.0253201008564,
-24.7180657944062));
#51607=CARTESIAN_POINT('Ctrl Pts',(-3.12014621424304,-12.0280099501904,
-24.7168516633817));
#51608=CARTESIAN_POINT('Ctrl Pts',(-3.09726104736722,-12.031904238561,-24.7150939460526));
#51609=CARTESIAN_POINT('Ctrl Pts',(-3.06727915293222,-12.0369286672949,
-24.7128278062112));
#51610=CARTESIAN_POINT('Ctrl Pts',(-3.03741245210651,-12.0419337916422,
-24.7105703731186));
#51611=CARTESIAN_POINT('Ctrl Pts',(-3.00050337107899,-12.0480604207122,
-24.7078084254843));
#51612=CARTESIAN_POINT('Ctrl Pts',(-2.95652738924272,-12.0551889523713,
-24.7045982342559));
#51613=CARTESIAN_POINT('Ctrl Pts',(-2.93861217079074,-12.0580930194684,
-24.7032904458966));
#51614=CARTESIAN_POINT('Ctrl Pts',(-2.91952400847139,-12.0611628292699,
-24.7019085134711));
#51615=CARTESIAN_POINT('Ctrl Pts',(-2.89926087788367,-12.0643880612036,
-24.7004572665812));
#51616=CARTESIAN_POINT('Ctrl Pts',(-2.84967927860436,-12.0722798406417,
-24.6969062288261));
#51617=CARTESIAN_POINT('Ctrl Pts',(-2.79306320304649,-12.081105438518,-24.692938717703));
#51618=CARTESIAN_POINT('Ctrl Pts',(-2.72937889016979,-12.0906809535796,
-24.688640353631));
#51619=CARTESIAN_POINT('Ctrl Pts',(-2.66611327954161,-12.1001935129539,
-24.6843702498105));
#51620=CARTESIAN_POINT('Ctrl Pts',(-2.59587189460584,-12.1104462002574,
-24.679773650128));
#51621=CARTESIAN_POINT('Ctrl Pts',(-2.51861770667281,-12.1212119874621,
-24.6749552284126));
#51622=CARTESIAN_POINT('Ctrl Pts',(-2.46588273788183,-12.1285608894109,
-24.6716660951555));
#51623=CARTESIAN_POINT('Ctrl Pts',(-2.40987996295885,-12.1361479142357,
-24.6682740289955));
#51624=CARTESIAN_POINT('Ctrl Pts',(-2.35059722570636,-12.1438880278938,
-24.6648178614771));
#51625=CARTESIAN_POINT('Ctrl Pts',(-2.31881048271695,-12.1480381905711,
-24.6629647029738));
#51626=CARTESIAN_POINT('Ctrl Pts',(-2.28608075398001,-12.1522321864854,
-24.6610931921645));
#51627=CARTESIAN_POINT('Ctrl Pts',(-2.25240618558163,-12.1564556378308,
-24.6592098515184));
#51628=CARTESIAN_POINT('Ctrl Pts',(-2.23556890138244,-12.1585673635036,
-24.6582681811953));
#51629=CARTESIAN_POINT('Ctrl Pts',(-2.21849540726422,-12.1606864526718,
-24.6573235526666));
#51630=CARTESIAN_POINT('Ctrl Pts',(-2.20118547572961,-12.1628110079849,
-24.6563768240204));
#51631=CARTESIAN_POINT('Ctrl Pts',(-2.19253050996231,-12.1638732856414,
-24.6559034596973));
#51632=CARTESIAN_POINT('Ctrl Pts',(-2.18381643484066,-12.16493692981,-24.6554295702951));
#51633=CARTESIAN_POINT('Ctrl Pts',(-2.1750432221839,-12.1660017003922,-24.6549552641153));
#51634=CARTESIAN_POINT('Ctrl Pts',(-2.16846331269133,-12.1668002783289,
-24.6545995344804));
#51635=CARTESIAN_POINT('Ctrl Pts',(-2.16185013833523,-12.1675994898712,
-24.6542435704039));
#51636=CARTESIAN_POINT('Ctrl Pts',(-2.1552036872966,-12.1683992325303,-24.6538874180593));
#51637=CARTESIAN_POINT('Ctrl Pts',(-2.15298820361706,-12.1686658134167,
-24.6537687006112));
#51638=CARTESIAN_POINT('Ctrl Pts',(-2.14946255514892,-12.1690891997327,
-24.6535801640996));
#51639=CARTESIAN_POINT('Ctrl Pts',(-2.14854614359989,-12.1691991483266,
-24.6535312047162));
#51640=CARTESIAN_POINT('Ctrl Pts',(-2.01285727760659,-12.1854787336713,
-24.6462820127763));
#51641=CARTESIAN_POINT('Ctrl Pts',(-1.87311902797097,-12.200646089438,-24.6395546412827));
#51642=CARTESIAN_POINT('Ctrl Pts',(-1.72934488862509,-12.2144325023485,
-24.6334653588438));
#51643=CARTESIAN_POINT('Ctrl Pts',(-1.55033452716363,-12.2315976947092,
-24.6258837126911));
#51644=CARTESIAN_POINT('Ctrl Pts',(-1.3650667468862,-12.2466229246189,-24.6192915670951));
#51645=CARTESIAN_POINT('Ctrl Pts',(-1.17358542883385,-12.2589711971898,
-24.613901599077));
#51646=CARTESIAN_POINT('Ctrl Pts',(-0.995034417419455,-12.2704856184357,
-24.6088756035861));
#51647=CARTESIAN_POINT('Ctrl Pts',(-0.811080765511128,-12.279672079365,
-24.6048950353104));
#51648=CARTESIAN_POINT('Ctrl Pts',(-0.621784930580049,-12.2860629160544,
-24.6021354957624));
#51649=CARTESIAN_POINT('Ctrl Pts',(-0.437714167124175,-12.2922773485535,
-24.5994521268886));
#51650=CARTESIAN_POINT('Ctrl Pts',(-0.248590430429552,-12.2958477298752,
-24.5979230997908));
#51651=CARTESIAN_POINT('Ctrl Pts',(-0.0545586007863394,-12.2963375937408,
-24.5977237909786));
#51652=CARTESIAN_POINT('Ctrl Pts',(0.0790391870814224,-12.2966748823647,
-24.5975865598012));
#51653=CARTESIAN_POINT('Ctrl Pts',(0.214962940974409,-12.2955512908672,
-24.5980798261454));
#51654=CARTESIAN_POINT('Ctrl Pts',(0.353152334498822,-12.2928182131356,
-24.5992620301425));
#51655=CARTESIAN_POINT('Ctrl Pts',(0.484530631885856,-12.2902198436815,
-24.600385965521));
#51656=CARTESIAN_POINT('Ctrl Pts',(0.617956409124449,-12.286166616767,-24.6021323416886));
#51657=CARTESIAN_POINT('Ctrl Pts',(0.753387341602309,-12.2805320625146,
-24.6045701077575));
#51658=CARTESIAN_POINT('Ctrl Pts',(0.832599513683294,-12.2772364691603,
-24.6059959322853));
#51659=CARTESIAN_POINT('Ctrl Pts',(0.912497523784989,-12.2733998517983,
-24.6076583513174));
#51660=CARTESIAN_POINT('Ctrl Pts',(0.993071860718278,-12.2689964190193,
-24.6095717929907));
#51661=CARTESIAN_POINT('Ctrl Pts',(1.03335902918492,-12.2667947026297,-24.6105285138274));
#51662=CARTESIAN_POINT('Ctrl Pts',(1.07381527937235,-12.2644512842182,-24.6115479940166));
#51663=CARTESIAN_POINT('Ctrl Pts',(1.11443933315437,-12.2619628983529,-24.6126320861955));
#51664=CARTESIAN_POINT('Ctrl Pts',(1.13475136004538,-12.2607187054203,-24.613174132285));
#51665=CARTESIAN_POINT('Ctrl Pts',(1.1551053378358,-12.2594382707433,-24.6137323316115));
#51666=CARTESIAN_POINT('Ctrl Pts',(1.17550110411703,-12.258121185405,-24.6143069179415));
#51667=CARTESIAN_POINT('Ctrl Pts',(1.18569898725765,-12.2574626427358,-24.6145942111066));
#51668=CARTESIAN_POINT('Ctrl Pts',(1.19590731752102,-12.2567949374089,-24.6148856010378));
#51669=CARTESIAN_POINT('Ctrl Pts',(1.20612607429678,-12.2561180181637,-24.6151811171442));
#51670=CARTESIAN_POINT('Ctrl Pts',(1.21003383986061,-12.2558591567607,-24.6152941257703));
#51671=CARTESIAN_POINT('Ctrl Pts',(1.21394313017906,-12.2555989479443,-24.6154077377951));
#51672=CARTESIAN_POINT('Ctrl Pts',(1.21785394409128,-12.2553373888361,-24.6155219548719));
#51673=CARTESIAN_POINT('Ctrl Pts',(1.21905649426289,-12.2552569610894,-24.6155570758897));
#51674=CARTESIAN_POINT('Ctrl Pts',(1.22025918849377,-12.2551764056696,-24.6155922541167));
#51675=CARTESIAN_POINT('Ctrl Pts',(1.22146202675023,-12.2550957224978,-24.6156274895932));
#51676=CARTESIAN_POINT('Ctrl Pts',(1.22401932127499,-12.2549241860237,-24.6157024019855));
#51677=CARTESIAN_POINT('Ctrl Pts',(1.22657726680809,-12.254752072081,-24.6157775731603));
#51678=CARTESIAN_POINT('Ctrl Pts',(1.22913586302588,-12.2545793799462,-24.615853003491));
#51679=CARTESIAN_POINT('Ctrl Pts',(1.23169445924366,-12.2544066878115,-24.6159284338216));
#51680=CARTESIAN_POINT('Ctrl Pts',(1.23563112026502,-12.2541398736881,-24.6160449895183));
#51681=CARTESIAN_POINT('Ctrl Pts',(1.23681360340771,-12.2540595681746,-24.6160800723573));
#51682=CARTESIAN_POINT('Ctrl Pts',(1.30415698594497,-12.2494861034709,-24.6180780687402));
#51683=CARTESIAN_POINT('Ctrl Pts',(1.37864973085997,-12.2440404697575,-24.6204626949177));
#51684=CARTESIAN_POINT('Ctrl Pts',(1.46026015657689,-12.2374742450696,-24.6233466830752));
#51685=CARTESIAN_POINT('Ctrl Pts',(1.54192304891292,-12.2309037990141,-24.6262325253231));
#51686=CARTESIAN_POINT('Ctrl Pts',(1.63071299872235,-12.2232112393102,-24.6296183548054));
#51687=CARTESIAN_POINT('Ctrl Pts',(1.72658504127951,-12.2141023251319,-24.6336393175605));
#51688=CARTESIAN_POINT('Ctrl Pts',(1.81123505362126,-12.2060596290858,-24.6371896179166));
#51689=CARTESIAN_POINT('Ctrl Pts',(1.90140617161389,-12.1969120518504,-24.6412353762544));
#51690=CARTESIAN_POINT('Ctrl Pts',(1.99705663526021,-12.1864285395999,-24.6458841574754));
#51691=CARTESIAN_POINT('Ctrl Pts',(2.1063311141233,-12.1744518037413,-24.6511950898631));
#51692=CARTESIAN_POINT('Ctrl Pts',(2.22275766737551,-12.1607320046081,-24.6572926544663));
#51693=CARTESIAN_POINT('Ctrl Pts',(2.34625419832298,-12.1448874689547,-24.6643580022169));
#51694=CARTESIAN_POINT('Ctrl Pts',(2.46249284595542,-12.1299741156598,-24.6710081199268));
#51695=CARTESIAN_POINT('Ctrl Pts',(2.58499494385502,-12.113177944025,-24.6785157979436));
#51696=CARTESIAN_POINT('Ctrl Pts',(2.71367114819397,-12.0941490502631,-24.6870505947827));
#51697=CARTESIAN_POINT('Ctrl Pts',(2.74257980860118,-12.0898739798994,-24.6889680397736));
#51698=CARTESIAN_POINT('Ctrl Pts',(2.77180000479066,-12.0854860993413,-24.6909373986732));
#51699=CARTESIAN_POINT('Ctrl Pts',(2.80133057466338,-12.0809812862044,-24.692960694511));
#51700=CARTESIAN_POINT('Ctrl Pts',(2.82674885367853,-12.0771037925522,-24.6947022355093));
#51701=CARTESIAN_POINT('Ctrl Pts',(2.85519249015935,-12.0727095378522,-24.6966769976858));
#51702=CARTESIAN_POINT('Ctrl Pts',(2.8838692040386,-12.0682098270556,-24.6987006235588));
#51703=CARTESIAN_POINT('Ctrl Pts',(2.89904593783843,-12.0658284205519,-24.6997715981242));
#51704=CARTESIAN_POINT('Ctrl Pts',(2.91428809658606,-12.0634182291851,-24.7008559061583));
#51705=CARTESIAN_POINT('Ctrl Pts',(2.92918282625697,-12.0610456032668,-24.7019236870447));
#51706=CARTESIAN_POINT('Ctrl Pts',(3.02452065291981,-12.0458589564775,-24.708758313205));
#51707=CARTESIAN_POINT('Ctrl Pts',(3.11288303257106,-12.031070308535,-24.7154292262998));
#51708=CARTESIAN_POINT('Ctrl Pts',(3.19431902969002,-12.0169622138921,-24.7218050079397));
#51709=CARTESIAN_POINT('Ctrl Pts',(3.25134055683339,-12.0070837187538,-24.7262693335292));
#51710=CARTESIAN_POINT('Ctrl Pts',(3.3049662326169,-11.9975378488254,-24.7305893943761));
#51711=CARTESIAN_POINT('Ctrl Pts',(3.35521234116895,-11.9884076807588,-24.7347260891693));
#51712=CARTESIAN_POINT('Ctrl Pts',(3.42777530415416,-11.9752223403105,-24.7407001006861));
#51713=CARTESIAN_POINT('Ctrl Pts',(3.49329025741202,-11.9629060207124,-24.7462907649862));
#51714=CARTESIAN_POINT('Ctrl Pts',(3.55180244408811,-11.9516685494414,-24.7513984144608));
#51715=CARTESIAN_POINT('Ctrl Pts',(3.61060203492046,-11.9403758811912,-24.756531152037));
#51716=CARTESIAN_POINT('Ctrl Pts',(3.66233004929159,-11.9301726003974,-24.7611761093311));
#51717=CARTESIAN_POINT('Ctrl Pts',(3.7070253556445,-11.9212240723819,-24.7652538073756));
#51718=CARTESIAN_POINT('Ctrl Pts',(3.75194669933796,-11.9122302890221,-24.7693521275411));
#51719=CARTESIAN_POINT('Ctrl Pts',(3.78976414426838,-11.9045039244158,-24.7728774247372));
#51720=CARTESIAN_POINT('Ctrl Pts',(3.82050797835506,-11.8981660086328,-24.7757709934024));
#51721=CARTESIAN_POINT('Ctrl Pts',(3.82703718787525,-11.8968199962925,-24.7763855138953));
#51722=CARTESIAN_POINT('Ctrl Pts',(3.83324732017357,-11.8955364413545,-24.7769716204608));
#51723=CARTESIAN_POINT('Ctrl Pts',(3.83913860511669,-11.894316236168,-24.7775288783472));
#51724=CARTESIAN_POINT('Ctrl Pts',(3.85140018573146,-11.8917766129102,-24.7786887038459));
#51725=CARTESIAN_POINT('Ctrl Pts',(3.86228059655449,-11.8895115217444,-24.7797235077149));
#51726=CARTESIAN_POINT('Ctrl Pts',(3.87178159558094,-11.8875277080389,-24.7806299973009));
#51727=CARTESIAN_POINT('Ctrl Pts',(3.87653209509417,-11.8865358011862,-24.781083242094));
#51728=CARTESIAN_POINT('Ctrl Pts',(3.88093774165891,-11.8856142138884,-24.781504408725));
#51729=CARTESIAN_POINT('Ctrl Pts',(3.88499870666068,-11.8847635947793,-24.7818931792817));
#51730=CARTESIAN_POINT('Ctrl Pts',(3.88702918916156,-11.8843382852248,-24.78208756456));
#51731=CARTESIAN_POINT('Ctrl Pts',(3.88897350127174,-11.8839307177306,-24.7822738508481));
#51732=CARTESIAN_POINT('Ctrl Pts',(3.89083166298951,-11.8835409680762,-24.7824520010861));
#51733=CARTESIAN_POINT('Ctrl Pts',(3.89176074384839,-11.8833460932489,-24.7825410762051));
#51734=CARTESIAN_POINT('Ctrl Pts',(3.89266828710916,-11.8831556728825,-24.7826281173135));
#51735=CARTESIAN_POINT('Ctrl Pts',(3.89355429510512,-11.8829697157939,-24.7827131200975));
#51736=CARTESIAN_POINT('Ctrl Pts',(3.89399729910309,-11.8828767372495,-24.7827556214894));
#51737=CARTESIAN_POINT('Ctrl Pts',(3.89443491926945,-11.8827848744668,-24.7827976133288));
#51738=CARTESIAN_POINT('Ctrl Pts',(3.89486446602496,-11.8826946941185,-24.7828388365331));
#51739=CARTESIAN_POINT('Ctrl Pts',(3.89529401278048,-11.8826045137702,-24.7828800597375));
#51740=CARTESIAN_POINT('Ctrl Pts',(3.89572088452154,-11.8825149548244,-24.7829209970462));
#51741=CARTESIAN_POINT('Ctrl Pts',(3.89744544075142,-11.8821526702451,-24.7830866116476));
#51742=CARTESIAN_POINT('Ctrl Pts',(3.90615289621541,-11.880323459469,-24.7839228161979));
#51743=CARTESIAN_POINT('Ctrl Pts',(3.91484190904383,-11.878492241168,-24.7847601238004));
#51744=CARTESIAN_POINT('Ctrl Pts',(3.92351248770123,-11.8766590889184,-24.7855985015432));
#51745=CARTESIAN_POINT('Ctrl Pts',(4.08352426403357,-11.8428290575766,-24.8010703999214));
#51746=CARTESIAN_POINT('Ctrl Pts',(4.23725683184937,-11.808344456804,-24.8169055229193));
#51747=CARTESIAN_POINT('Ctrl Pts',(4.38477077580503,-11.773645900217,-24.8329066121935));
#51748=CARTESIAN_POINT('Ctrl Pts',(4.40473563417751,-11.7689497220158,-24.8350722344567));
#51749=CARTESIAN_POINT('Ctrl Pts',(4.42458660093341,-11.7642495521737,-24.8372409190368));
#51750=CARTESIAN_POINT('Ctrl Pts',(4.44432384241394,-11.7595464156776,-24.8394121977579));
#51751=CARTESIAN_POINT('Ctrl Pts',(4.59308111763143,-11.7240994272611,-24.8557768709375));
#51752=CARTESIAN_POINT('Ctrl Pts',(4.73537748962768,-11.6884880158654,-24.8722877337365));
#51753=CARTESIAN_POINT('Ctrl Pts',(4.87128883771487,-11.6531251539034,-24.8887562362082));
#51754=CARTESIAN_POINT('Ctrl Pts',(4.89544337944055,-11.6468403679984,-24.8916830641421));
#51755=CARTESIAN_POINT('Ctrl Pts',(4.91939627029786,-11.6405633068695,-24.8946085907191));
#51756=CARTESIAN_POINT('Ctrl Pts',(4.94314796326616,-11.634296127747,-24.8975318051419));
#51757=CARTESIAN_POINT('Ctrl Pts',(5.07995159612902,-11.5981987904793,-24.914368767173));
#51758=CARTESIAN_POINT('Ctrl Pts',(5.21008001675493,-11.562433404087,-24.931127948449));
#51759=CARTESIAN_POINT('Ctrl Pts',(5.33362132823233,-11.5273836985521,-24.947629563727));
#51760=CARTESIAN_POINT('Ctrl Pts',(5.3698064122361,-11.5171176869329,-24.9524628646519));
#51761=CARTESIAN_POINT('Ctrl Pts',(5.40542643050983,-11.5069127441063,-24.9572741575169));
#51762=CARTESIAN_POINT('Ctrl Pts',(5.44048367932361,-11.4967777094823,-24.9620591479588));
#51763=CARTESIAN_POINT('Ctrl Pts',(5.5634076792632,-11.46124043723,-24.9788371378094));
#51764=CARTESIAN_POINT('Ctrl Pts',(5.67941229692956,-11.426566627261,-24.9952908229024));
#51765=CARTESIAN_POINT('Ctrl Pts',(5.78859481050879,-11.3931049741266,-25.0112500391612));
#51766=CARTESIAN_POINT('Ctrl Pts',(5.84240057663458,-11.3766148803953,-25.0191148320609));
#51767=CARTESIAN_POINT('Ctrl Pts',(5.89454960328078,-11.3604183740888,-25.0268597295277));
#51768=CARTESIAN_POINT('Ctrl Pts',(5.94505368243095,-11.3445527218703,-25.0344655498479));
#51769=CARTESIAN_POINT('Ctrl Pts',(5.95968231208449,-11.3399571970251,-25.0366685942464));
#51770=CARTESIAN_POINT('Ctrl Pts',(5.97417293278451,-11.3353894121292,-25.0388599757614));
#51771=CARTESIAN_POINT('Ctrl Pts',(5.98852581858904,-11.3308502293444,-25.0410392599613));
#51772=CARTESIAN_POINT('Ctrl Pts',(-6.39567215542467,-11.8440001024728,
-24.2657748968686));
#51773=CARTESIAN_POINT('Ctrl Pts',(-6.35564925618098,-11.8565901643257,
-24.2594187494307));
#51774=CARTESIAN_POINT('Ctrl Pts',(-5.98524940757696,-11.9719910115992,
-24.2012637897805));
#51775=CARTESIAN_POINT('Ctrl Pts',(-5.25616631904133,-12.1789676278653,
-24.0987566446471));
#51776=CARTESIAN_POINT('Ctrl Pts',(-4.1757614528087,-12.4300245021709,-23.9769546135746));
#51777=CARTESIAN_POINT('Ctrl Pts',(-3.01936948336144,-12.6350408997157,
-23.8792988421013));
#51778=CARTESIAN_POINT('Ctrl Pts',(-1.83578686335412,-12.7756187619401,
-23.8136687413269));
#51779=CARTESIAN_POINT('Ctrl Pts',(-0.697923544232415,-12.8441382007264,
-23.782558252307));
#51780=CARTESIAN_POINT('Ctrl Pts',(0.331409741550182,-12.8512034879543,
-23.7794557881091));
#51781=CARTESIAN_POINT('Ctrl Pts',(1.24580985113917,-12.8144571656071,-23.7959567162203));
#51782=CARTESIAN_POINT('Ctrl Pts',(2.0703011525311,-12.7465811278717,-23.8272319476035));
#51783=CARTESIAN_POINT('Ctrl Pts',(2.81706942635404,-12.6564395388812,-23.8693929263403));
#51784=CARTESIAN_POINT('Ctrl Pts',(3.49018596890746,-12.5517033164802,-23.9189811921973));
#51785=CARTESIAN_POINT('Ctrl Pts',(4.09497305511126,-12.4387782665359,-23.9729948461712));
#51786=CARTESIAN_POINT('Ctrl Pts',(4.65005393633298,-12.3195528639124,-24.0305544994279));
#51787=CARTESIAN_POINT('Ctrl Pts',(5.18050287209621,-12.1916401414439,-24.0928853069425));
#51788=CARTESIAN_POINT('Ctrl Pts',(5.70542267295585,-12.0514960850741,-24.1618790928945));
#51789=CARTESIAN_POINT('Ctrl Pts',(6.10978283806977,-11.9329730134373,-24.2209473269322));
#51790=CARTESIAN_POINT('Ctrl Pts',(6.34031611249689,-11.8614128328345,-24.2569837007452));
#51791=CARTESIAN_POINT('Ctrl Pts',(6.39541677164253,-11.8440802209038,-24.2657356729641));
#51792=CARTESIAN_POINT('Ctrl Pts',(-6.33018795450903,-11.8153030248918,
-24.6384814580648));
#51793=CARTESIAN_POINT('Ctrl Pts',(-6.29063921510137,-11.8278586316894,
-24.6322059111688));
#51794=CARTESIAN_POINT('Ctrl Pts',(-5.9246003059131,-11.9429535886473,-24.5747847388569));
#51795=CARTESIAN_POINT('Ctrl Pts',(-5.20363640375749,-12.1495431753517,
-24.4735093872846));
#51796=CARTESIAN_POINT('Ctrl Pts',(-4.13466319834969,-12.400333149385,-24.3531155353953));
#51797=CARTESIAN_POINT('Ctrl Pts',(-2.99013101626481,-12.6052506194047,
-24.2565628937697));
#51798=CARTESIAN_POINT('Ctrl Pts',(-1.81835018697561,-12.7458213587748,
-24.1916588641543));
#51799=CARTESIAN_POINT('Ctrl Pts',(-0.691526419463407,-12.8143591144599,
-24.1608816865859));
#51800=CARTESIAN_POINT('Ctrl Pts',(0.328410955103737,-12.8214279221244,
-24.1578109793223));
#51801=CARTESIAN_POINT('Ctrl Pts',(1.23410624365119,-12.7846688139739,-24.1741376713656));
#51802=CARTESIAN_POINT('Ctrl Pts',(2.05052545184689,-12.7167848350623,-24.2050718889341));
#51803=CARTESIAN_POINT('Ctrl Pts',(2.78983578881101,-12.6266522506618,-24.2467655952706));
#51804=CARTESIAN_POINT('Ctrl Pts',(3.45611831470981,-12.5219522866885,-24.2957971475504));
#51805=CARTESIAN_POINT('Ctrl Pts',(4.05467056771375,-12.4090965633996,-24.3491974594818));
#51806=CARTESIAN_POINT('Ctrl Pts',(4.60393606416149,-12.2899790555555,-24.4060956630845));
#51807=CARTESIAN_POINT('Ctrl Pts',(5.12872017337514,-12.1622243332721,-24.4676997961477));
#51808=CARTESIAN_POINT('Ctrl Pts',(5.64789136142997,-12.022309291172,-24.5358734405517));
#51809=CARTESIAN_POINT('Ctrl Pts',(6.04766215329681,-11.904040942247,-24.5942191807346));
#51810=CARTESIAN_POINT('Ctrl Pts',(6.27548786378983,-11.8326680689264,-24.6298017767411));
#51811=CARTESIAN_POINT('Ctrl Pts',(6.32993527380381,-11.8153829807007,-24.6384426479982));
#51812=CARTESIAN_POINT('Ctrl Pts',(-6.21932914003729,-11.6046077138231,
-24.933941067311));
#51813=CARTESIAN_POINT('Ctrl Pts',(-6.18048424948508,-11.6170331460216,
-24.9278367279444));
#51814=CARTESIAN_POINT('Ctrl Pts',(-5.82094614637916,-11.7309405707257,
-24.871982184622));
#51815=CARTESIAN_POINT('Ctrl Pts',(-5.11256398456841,-11.9354888600937,
-24.7734733502725));
#51816=CARTESIAN_POINT('Ctrl Pts',(-4.06219748998055,-12.1838752205529,
-24.656435331966));
#51817=CARTESIAN_POINT('Ctrl Pts',(-2.93773430970566,-12.3868544707923,
-24.5626392307631));
#51818=CARTESIAN_POINT('Ctrl Pts',(-1.78661004834439,-12.5261043229835,
-24.4996240375242));
#51819=CARTESIAN_POINT('Ctrl Pts',(-0.679627595412669,-12.5940042619886,
-24.469747090831));
#51820=CARTESIAN_POINT('Ctrl Pts',(0.32279241813113,-12.6010084102561,-24.4667652656686));
#51821=CARTESIAN_POINT('Ctrl Pts',(1.21265278063735,-12.5645895081712,-24.4826158046806));
#51822=CARTESIAN_POINT('Ctrl Pts',(2.01469390807635,-12.4973407985779,-24.5126460662249));
#51823=CARTESIAN_POINT('Ctrl Pts',(2.74097574449004,-12.40805553802,-24.5531296341404));
#51824=CARTESIAN_POINT('Ctrl Pts',(3.39554807864259,-12.3043438963876,-24.6007526810749));
#51825=CARTESIAN_POINT('Ctrl Pts',(3.98362077418606,-12.192558706476,-24.652636935921));
#51826=CARTESIAN_POINT('Ctrl Pts',(4.5233025684579,-12.0745788464337,-24.7079386489045));
#51827=CARTESIAN_POINT('Ctrl Pts',(5.03894734293331,-11.9480565297811,-24.7678332938225));
#51828=CARTESIAN_POINT('Ctrl Pts',(5.54906664696171,-11.8095120106988,-24.8341333987973));
#51829=CARTESIAN_POINT('Ctrl Pts',(5.94181973580656,-11.6924305250497,-24.8908864048995));
#51830=CARTESIAN_POINT('Ctrl Pts',(6.16560267824642,-11.6217926877057,-24.9254982178085));
#51831=CARTESIAN_POINT('Ctrl Pts',(6.21908066379017,-11.6046868956139,-24.9339032360192));
#51832=CARTESIAN_POINT('Ctrl Pts',(-6.09478101909931,-11.2722125663433,
-25.0678681419845));
#51833=CARTESIAN_POINT('Ctrl Pts',(-6.05666854227872,-11.2844493451113,
-25.0619766664134));
#51834=CARTESIAN_POINT('Ctrl Pts',(-5.70391349769389,-11.3966273350641,
-25.0080736685403));
#51835=CARTESIAN_POINT('Ctrl Pts',(-5.00898011870794,-11.5980641644672,
-24.9130750297103));
#51836=CARTESIAN_POINT('Ctrl Pts',(-3.97907763477767,-11.8425981319446,
-24.8003808773973));
#51837=CARTESIAN_POINT('Ctrl Pts',(-2.8771566178203,-12.0423546994034,-24.7102064331904));
#51838=CARTESIAN_POINT('Ctrl Pts',(-1.74963938185109,-12.1793480627038,
-24.6497026624673));
#51839=CARTESIAN_POINT('Ctrl Pts',(-0.66562847075,-12.2461366725668,-24.6210354030492));
#51840=CARTESIAN_POINT('Ctrl Pts',(0.316160263864133,-12.2530264963728,
-24.6181741642278));
#51841=CARTESIAN_POINT('Ctrl Pts',(1.18758201207714,-12.2172033812172,-24.6333828131016));
#51842=CARTESIAN_POINT('Ctrl Pts',(1.97304891122712,-12.1510512680947,-24.662204699665));
#51843=CARTESIAN_POINT('Ctrl Pts',(2.68445564141552,-12.0632090701854,-24.7010813430047));
#51844=CARTESIAN_POINT('Ctrl Pts',(3.32578864566661,-11.961154888898,-24.7468468918969));
#51845=CARTESIAN_POINT('Ctrl Pts',(3.90213225627227,-11.8511350032299,-24.7967459194263));
#51846=CARTESIAN_POINT('Ctrl Pts',(4.43120108774589,-11.7349969248286,-24.849972634402));
#51847=CARTESIAN_POINT('Ctrl Pts',(4.93684397707271,-11.6104287119617,-24.9076638088831));
#51848=CARTESIAN_POINT('Ctrl Pts',(5.43719497822094,-11.4740040324212,-24.9715726993592));
#51849=CARTESIAN_POINT('Ctrl Pts',(5.82250744905605,-11.3587019609412,-25.0263181394208));
#51850=CARTESIAN_POINT('Ctrl Pts',(6.04206764945466,-11.2891366012123,-25.0597197276758));
#51851=CARTESIAN_POINT('Ctrl Pts',(6.09453704716553,-11.2722905841804,-25.0678315745393));
#51852=CARTESIAN_POINT('',(6.27159454870591,-11.879492346709,-24.2690137147315));
#51853=CARTESIAN_POINT('Origin',(5.999999949022,-10.92778026693,-24.1259420051984));
#51854=CARTESIAN_POINT('Ctrl Pts',(-6.2715938732803,-11.8794984953269,-24.269012375374));
#51855=CARTESIAN_POINT('Ctrl Pts',(-6.13239663762701,-11.9224692223419,
-24.2474082712106));
#51856=CARTESIAN_POINT('Ctrl Pts',(-5.98564490228836,-11.9663158806333,
-24.2255025400386));
#51857=CARTESIAN_POINT('Ctrl Pts',(-5.8313286107345,-12.0105539104888,-24.2035349755448));
#51858=CARTESIAN_POINT('Ctrl Pts',(-5.67907405556145,-12.0542008999905,
-24.1818609077807));
#51859=CARTESIAN_POINT('Ctrl Pts',(-5.51945543077222,-12.0982289054275,
-24.1601268768661));
#51860=CARTESIAN_POINT('Ctrl Pts',(-5.35247238148756,-12.1421228678868,
-24.1385689856038));
#51861=CARTESIAN_POINT('Ctrl Pts',(-5.32566688848742,-12.1491690878984,
-24.1351083355211));
#51862=CARTESIAN_POINT('Ctrl Pts',(-5.29867164443853,-12.1562117478511,
-24.1316522325387));
#51863=CARTESIAN_POINT('Ctrl Pts',(-5.27148667848168,-12.1632485947852,
-24.1282016614138));
#51864=CARTESIAN_POINT('Ctrl Pts',(-5.14595415318808,-12.1957427743678,
-24.1122678946509));
#51865=CARTESIAN_POINT('Ctrl Pts',(-5.01637573150645,-12.2281142363005,
-24.0964517500017));
#51866=CARTESIAN_POINT('Ctrl Pts',(-4.882757385002,-12.26013253772,-24.0808623957014));
#51867=CARTESIAN_POINT('Ctrl Pts',(-4.711064069478,-12.301274555055,-24.0608308057534));
#51868=CARTESIAN_POINT('Ctrl Pts',(-4.5326954979539,-12.3418362421708,-24.0411729378986));
#51869=CARTESIAN_POINT('Ctrl Pts',(-4.34764548374925,-12.3812950798105,
-24.0221340537593));
#51870=CARTESIAN_POINT('Ctrl Pts',(-4.2958405153995,-12.3923416276523,-24.0168040958315));
#51871=CARTESIAN_POINT('Ctrl Pts',(-4.24351200589396,-12.4033014559238,
-24.0115227210219));
#51872=CARTESIAN_POINT('Ctrl Pts',(-4.19066006814981,-12.4141624244733,
-24.0062954756857));
#51873=CARTESIAN_POINT('Ctrl Pts',(-4.14338502638451,-12.4238773519424,
-24.0016198052726));
#51874=CARTESIAN_POINT('Ctrl Pts',(-4.09569119111324,-12.4335131772699,
-23.996987443632));
#51875=CARTESIAN_POINT('Ctrl Pts',(-4.04757899088175,-12.4430611425052,
-23.9924025353514));
#51876=CARTESIAN_POINT('Ctrl Pts',(-3.90056247343951,-12.4722368732097,
-23.978392424715));
#51877=CARTESIAN_POINT('Ctrl Pts',(-3.749635972985,-12.5005941111466,-23.9648249555871));
#51878=CARTESIAN_POINT('Ctrl Pts',(-3.59479966513697,-12.5278747715792,
-23.9518214668319));
#51879=CARTESIAN_POINT('Ctrl Pts',(-3.51738151121296,-12.5415151017955,
-23.9453197224542));
#51880=CARTESIAN_POINT('Ctrl Pts',(-3.43898589682887,-12.5548860374477,
-23.9389590687969));
#51881=CARTESIAN_POINT('Ctrl Pts',(-3.35961279462372,-12.5679537431773,
-23.9327552486077));
#51882=CARTESIAN_POINT('Ctrl Pts',(-3.31992624352115,-12.5744875960422,
-23.9296533385131));
#51883=CARTESIAN_POINT('Ctrl Pts',(-3.27999531807212,-12.5809456256128,
-23.926590634974));
#51884=CARTESIAN_POINT('Ctrl Pts',(-3.23982001430566,-12.5873234964514,
-23.9235691505921));
#51885=CARTESIAN_POINT('Ctrl Pts',(-3.21973236242243,-12.5905124318707,
-23.9220584084011));
#51886=CARTESIAN_POINT('Ctrl Pts',(-3.19958361581005,-12.5936813265724,
-23.9205579708818));
#51887=CARTESIAN_POINT('Ctrl Pts',(-3.17937377348063,-12.5968296320843,
-23.9190680904652));
#51888=CARTESIAN_POINT('Ctrl Pts',(-3.16169016144239,-12.5995843994072,
-23.9177644451007));
#51889=CARTESIAN_POINT('Ctrl Pts',(-3.14395977298706,-12.6023234030703,
-23.916468882511));
#51890=CARTESIAN_POINT('Ctrl Pts',(-3.12618260735964,-12.6050462727838,
-23.9151815725702));
#51891=CARTESIAN_POINT('Ctrl Pts',(-3.12364301227001,-12.6054352541714,
-23.9149976711501));
#51892=CARTESIAN_POINT('Ctrl Pts',(-3.11986203723764,-12.6060134334648,
-23.9147243465347));
#51893=CARTESIAN_POINT('Ctrl Pts',(-3.11856095818475,-12.606212228053,-23.9146303740971));
#51894=CARTESIAN_POINT('Ctrl Pts',(-3.09161304666525,-12.6103296557857,
-23.9126840196999));
#51895=CARTESIAN_POINT('Ctrl Pts',(-3.06343997575514,-12.6145807550419,
-23.9106767095399));
#51896=CARTESIAN_POINT('Ctrl Pts',(-3.03404177228778,-12.618950273952,-23.9086156635078));
#51897=CARTESIAN_POINT('Ctrl Pts',(-2.96197568736319,-12.6296616128679,
-23.9035632623108));
#51898=CARTESIAN_POINT('Ctrl Pts',(-2.88254751287245,-12.641087839082,-23.8981864399));
#51899=CARTESIAN_POINT('Ctrl Pts',(-2.79575688315666,-12.6529718125133,
-23.8926067538628));
#51900=CARTESIAN_POINT('Ctrl Pts',(-2.70929650814212,-12.6648105651863,
-23.8870482995824));
#51901=CARTESIAN_POINT('Ctrl Pts',(-2.61552935566523,-12.6771036167269,
-23.8812885584487));
#51902=CARTESIAN_POINT('Ctrl Pts',(-2.51445615805138,-12.6895496271244,
-23.8754690386501));
#51903=CARTESIAN_POINT('Ctrl Pts',(-2.50259521508505,-12.6910101668418,
-23.8747861178159));
#51904=CARTESIAN_POINT('Ctrl Pts',(-2.49063366414967,-12.6924727591018,
-23.8741023976447));
#51905=CARTESIAN_POINT('Ctrl Pts',(-2.4785715099771,-12.6939368738316,-23.8734181258235));
#51906=CARTESIAN_POINT('Ctrl Pts',(-2.37688568616911,-12.706279587274,-23.8676496086209));
#51907=CARTESIAN_POINT('Ctrl Pts',(-2.26804987401106,-12.7187343062723,
-23.8618405787172));
#51908=CARTESIAN_POINT('Ctrl Pts',(-2.15206286682857,-12.7309579443555,
-23.856152503585));
#51909=CARTESIAN_POINT('Ctrl Pts',(-2.11969742264863,-12.734368873611,-23.8545652820276));
#51910=CARTESIAN_POINT('Ctrl Pts',(-2.08677519359464,-12.7377615266798,
-23.852987599166));
#51911=CARTESIAN_POINT('Ctrl Pts',(-2.05329627361692,-12.7411277873687,
-23.8514232425027));
#51912=CARTESIAN_POINT('Ctrl Pts',(-1.97656814623441,-12.748842698098,-23.8478379966998));
#51913=CARTESIAN_POINT('Ctrl Pts',(-1.89691554157196,-12.7564195700983,
-23.8443225621781));
#51914=CARTESIAN_POINT('Ctrl Pts',(-1.81433841441059,-12.7637550184018,
-23.8409252171504));
#51915=CARTESIAN_POINT('Ctrl Pts',(-1.81240161146196,-12.7639270674714,
-23.8408455342153));
#51916=CARTESIAN_POINT('Ctrl Pts',(-1.8104631997204,-12.7640989833751,-23.8407659162187));
#51917=CARTESIAN_POINT('Ctrl Pts',(-1.80852317916683,-12.7642707647223,
-23.8406863638458));
#51918=CARTESIAN_POINT('Ctrl Pts',(-1.7691060435725,-12.7677610002474,-23.8390700270161));
#51919=CARTESIAN_POINT('Ctrl Pts',(-1.72902475054208,-12.7711957218126,
-23.8374807696023));
#51920=CARTESIAN_POINT('Ctrl Pts',(-1.68827932336461,-12.7745632602754,
-23.8359241929636));
#51921=CARTESIAN_POINT('Ctrl Pts',(-1.66690391177416,-12.7763299007471,
-23.8351075990872));
#51922=CARTESIAN_POINT('Ctrl Pts',(-1.64534571982271,-12.7780780454456,
-23.8342999985264));
#51923=CARTESIAN_POINT('Ctrl Pts',(-1.62360474836943,-12.7798059674892,
-23.8335022087749));
#51924=CARTESIAN_POINT('Ctrl Pts',(-1.61273426264279,-12.7806699285111,
-23.8331033138992));
#51925=CARTESIAN_POINT('Ctrl Pts',(-1.60181808200573,-12.781528833429,-23.8327068716795));
#51926=CARTESIAN_POINT('Ctrl Pts',(-1.5908562065608,-12.7823824635436,-23.8323129856623));
#51927=CARTESIAN_POINT('Ctrl Pts',(-1.58537526883834,-12.7828092786009,
-23.8321160426538));
#51928=CARTESIAN_POINT('Ctrl Pts',(-1.57988290741174,-12.7832347749296,
-23.8319197386929));
#51929=CARTESIAN_POINT('Ctrl Pts',(-1.57437912229396,-12.7836589250135,
-23.8317240868131));
#51930=CARTESIAN_POINT('Ctrl Pts',(-1.56887533717618,-12.7840830750973,
-23.8315284349333));
#51931=CARTESIAN_POINT('Ctrl Pts',(-1.56205961010252,-12.7846050491578,
-23.8312877046057));
#51932=CARTESIAN_POINT('Ctrl Pts',(-1.55783349587533,-12.7849273088989,
-23.8311391004704));
#51933=CARTESIAN_POINT('Ctrl Pts',(-1.33210031738351,-12.8021404535854,
-23.8232015763092));
#51934=CARTESIAN_POINT('Ctrl Pts',(-1.1100537646997,-12.8153351589271,-23.8171220363203));
#51935=CARTESIAN_POINT('Ctrl Pts',(-0.89169689626609,-12.8248709187615,
-23.8127291065153));
#51936=CARTESIAN_POINT('Ctrl Pts',(-0.848420677506258,-12.8267608141039,
-23.8118584703287));
#51937=CARTESIAN_POINT('Ctrl Pts',(-0.805289281811483,-12.8285068906274,
-23.8110541625113));
#51938=CARTESIAN_POINT('Ctrl Pts',(-0.762302580912269,-12.8301118030515,
-23.810314964591));
#51939=CARTESIAN_POINT('Ctrl Pts',(-0.724716128547589,-12.8315150967009,
-23.80966862917));
#51940=CARTESIAN_POINT('Ctrl Pts',(-0.687240284721794,-12.8328104687764,
-23.8090720400251));
#51941=CARTESIAN_POINT('Ctrl Pts',(-0.649875247251341,-12.833999670689,
-23.8085242653197));
#51942=CARTESIAN_POINT('Ctrl Pts',(-0.558064364505217,-12.8369216984653,
-23.8071783097778));
#51943=CARTESIAN_POINT('Ctrl Pts',(-0.466922522056544,-12.8392027905172,
-23.8061270352528));
#51944=CARTESIAN_POINT('Ctrl Pts',(-0.376448954449454,-12.8408704269592,
-23.8053581701341));
#51945=CARTESIAN_POINT('Ctrl Pts',(-0.312801781035167,-12.8420435911068,
-23.8048172818633));
#51946=CARTESIAN_POINT('Ctrl Pts',(-0.249485494921159,-12.8429131418327,
-23.8044160904582));
#51947=CARTESIAN_POINT('Ctrl Pts',(-0.186500096427085,-12.8434883989062,
-23.8041502796551));
#51948=CARTESIAN_POINT('Ctrl Pts',(-0.155007397180047,-12.843776027443,
-23.8040173742536));
#51949=CARTESIAN_POINT('Ctrl Pts',(-0.123597419714937,-12.8439900795261,
-23.8039183136937));
#51950=CARTESIAN_POINT('Ctrl Pts',(-0.0922701636528899,-12.8441317019992,
-23.8038525594803));
#51951=CARTESIAN_POINT('Ctrl Pts',(-0.0647192958780385,-12.8442562523914,
-23.8037947317013));
#51952=CARTESIAN_POINT('Ctrl Pts',(-0.038338203916619,-12.8443236937568,
-23.8037631767086));
#51953=CARTESIAN_POINT('Ctrl Pts',(-0.0102093991919666,-12.8443378682957,
-23.8037560881866));
#51954=CARTESIAN_POINT('Ctrl Pts',(-0.0063537932791852,-12.844339811195,
-23.8037551165653));
#51955=CARTESIAN_POINT('Ctrl Pts',(-0.00246535106877531,-12.8443406806773,
-23.8037546373443));
#51956=CARTESIAN_POINT('Ctrl Pts',(0.00146344077723272,-12.8443404157055,
-23.8037546778085));
#51957=CARTESIAN_POINT('Ctrl Pts',(0.123997928659108,-12.8443321515412,
-23.8037559398407));
#51958=CARTESIAN_POINT('Ctrl Pts',(0.246529019799122,-12.8432200162837,
-23.8042792014033));
#51959=CARTESIAN_POINT('Ctrl Pts',(0.369061817155031,-12.8410040026569,
-23.8053128196795));
#51960=CARTESIAN_POINT('Ctrl Pts',(0.644876546147541,-12.8360158753058,
-23.8076394387636));
#51961=CARTESIAN_POINT('Ctrl Pts',(0.920699733133829,-12.825437781153,-23.8125503711935));
#51962=CARTESIAN_POINT('Ctrl Pts',(1.19652079061211,-12.8092724576358,-23.8200737229866));
#51963=CARTESIAN_POINT('Ctrl Pts',(1.22211852101468,-12.8077722255758,-23.8207719319365));
#51964=CARTESIAN_POINT('Ctrl Pts',(1.2477162348584,-12.8062238382288,-23.8214926578109));
#51965=CARTESIAN_POINT('Ctrl Pts',(1.27331392444618,-12.8046272774463,-23.8222359333602));
#51966=CARTESIAN_POINT('Ctrl Pts',(1.37082860577193,-12.7985451615041,-23.8250674497781));
#51967=CARTESIAN_POINT('Ctrl Pts',(1.46834293639484,-12.7917639892806,-23.8282261876786));
#51968=CARTESIAN_POINT('Ctrl Pts',(1.56585686947366,-12.7842847835651,-23.83171014081));
#51969=CARTESIAN_POINT('Ctrl Pts',(1.74018067037264,-12.7709143499577,-23.8379383374672));
#51970=CARTESIAN_POINT('Ctrl Pts',(1.91450485624828,-12.7553132735693,-23.8452071705032));
#51971=CARTESIAN_POINT('Ctrl Pts',(2.08882858929884,-12.7374808031892,-23.8535163666922));
#51972=CARTESIAN_POINT('Ctrl Pts',(2.17523695513979,-12.7286416474558,-23.8576350489368));
#51973=CARTESIAN_POINT('Ctrl Pts',(2.26164519251036,-12.7192541347995,-23.8620094030456));
#51974=CARTESIAN_POINT('Ctrl Pts',(2.34805359245555,-12.709318748311,-23.8666392626566));
#51975=CARTESIAN_POINT('Ctrl Pts',(2.47841969335505,-12.6943290297391,-23.8736244255063));
#51976=CARTESIAN_POINT('Ctrl Pts',(2.60878583338074,-12.6780923255439,-23.8811913884885));
#51977=CARTESIAN_POINT('Ctrl Pts',(2.7391519852192,-12.6606086884026,-23.8893399953968));
#51978=CARTESIAN_POINT('Ctrl Pts',(2.77254675020636,-12.656130056908,-23.8914273532641));
#51979=CARTESIAN_POINT('Ctrl Pts',(2.80594152189464,-12.651569593432,-23.8935528679851));
#51980=CARTESIAN_POINT('Ctrl Pts',(2.83933628185077,-12.6469272782789,-23.8957165518898));
#51981=CARTESIAN_POINT('Ctrl Pts',(2.87112458799384,-12.6425082815413,-23.8977761518525));
#51982=CARTESIAN_POINT('Ctrl Pts',(2.90291288348001,-12.6380151185757,-23.8998703371182));
#51983=CARTESIAN_POINT('Ctrl Pts',(2.93470118431995,-12.6334478148393,-23.9019990914454));
#51984=CARTESIAN_POINT('Ctrl Pts',(2.98358847573866,-12.6264237492911,-23.9052729069815));
#51985=CARTESIAN_POINT('Ctrl Pts',(3.03247576368835,-12.6192243319166,-23.9086285031247));
#51986=CARTESIAN_POINT('Ctrl Pts',(3.08136305406435,-12.6118496261618,-23.9120658770569));
#51987=CARTESIAN_POINT('Ctrl Pts',(3.09765881752302,-12.6093913909102,-23.9132116683676));
#51988=CARTESIAN_POINT('Ctrl Pts',(3.11203760771907,-12.607207438777,-23.9142296216478));
#51989=CARTESIAN_POINT('Ctrl Pts',(3.13025034526784,-12.6044164915618,-23.9155305099189));
#51990=CARTESIAN_POINT('Ctrl Pts',(3.25877318570469,-12.5847214587502,-23.9247105607072));
#51991=CARTESIAN_POINT('Ctrl Pts',(3.38587636788282,-12.5640249808262,-23.9344227860646));
#51992=CARTESIAN_POINT('Ctrl Pts',(3.51154612818603,-12.5424083497868,-23.9446281308574));
#51993=CARTESIAN_POINT('Ctrl Pts',(3.71380564173032,-12.5076174082911,-23.9610531488439));
#51994=CARTESIAN_POINT('Ctrl Pts',(3.91235133346752,-12.4704440589107,-23.9787552448699));
#51995=CARTESIAN_POINT('Ctrl Pts',(4.10714944138902,-12.4312193029833,-23.9975754628997));
#51996=CARTESIAN_POINT('Ctrl Pts',(4.29250029057756,-12.3938968572064,-24.0154829437831));
#51997=CARTESIAN_POINT('Ctrl Pts',(4.47445852096732,-12.3547170216527,-24.0344028076301));
#51998=CARTESIAN_POINT('Ctrl Pts',(4.65301431239387,-12.3139520128374,-24.0542053141028));
#51999=CARTESIAN_POINT('Ctrl Pts',(4.83065430931525,-12.2733960836087,-24.0739062555326));
#52000=CARTESIAN_POINT('Ctrl Pts',(5.00492682818613,-12.2312711675382,-24.0944809142273));
#52001=CARTESIAN_POINT('Ctrl Pts',(5.17583782751897,-12.1878310093366,-24.1158115156527));
#52002=CARTESIAN_POINT('Ctrl Pts',(5.35320999676605,-12.1427486265601,-24.1379485054366));
#52003=CARTESIAN_POINT('Ctrl Pts',(5.52696176320015,-12.0962497351854,-24.1608998542789));
#52004=CARTESIAN_POINT('Ctrl Pts',(5.69711466993369,-12.0485999934587,-24.1845484510568));
#52005=CARTESIAN_POINT('Ctrl Pts',(5.87744654476362,-11.9980997262243,-24.2096117654364));
#52006=CARTESIAN_POINT('Ctrl Pts',(6.05373611657599,-11.9463068999075,-24.2354586152215));
#52007=CARTESIAN_POINT('Ctrl Pts',(6.22602222360087,-11.8935144278621,-24.2619713031445));
#52008=CARTESIAN_POINT('Ctrl Pts',(6.2412447323608,-11.8888498969719,-24.2643138578121));
#52009=CARTESIAN_POINT('Ctrl Pts',(6.25643599311294,-11.8841775483418,-24.2666616081869));
#52010=CARTESIAN_POINT('Ctrl Pts',(6.27159604017512,-11.8794975712383,-24.269014496721));
#52011=CARTESIAN_POINT('Origin',(5.999999999061,-10.9277802195584,-24.1259421376201));
#52012=CARTESIAN_POINT('Origin',(5.99996968604348,-10.92775528448,-24.1259230378048));
#52013=CARTESIAN_POINT('Ctrl Pts',(6.2506839997157,-8.43293793822341,-13.9512886376407));
#52014=CARTESIAN_POINT('Ctrl Pts',(6.30609107903449,-8.4089443361267,-13.9477561522565));
#52015=CARTESIAN_POINT('Ctrl Pts',(6.42571412640754,-8.34736363641913,-13.9452436913382));
#52016=CARTESIAN_POINT('Ctrl Pts',(6.60616709762988,-8.21875062808475,-13.9600011874018));
#52017=CARTESIAN_POINT('Ctrl Pts',(6.78564627982441,-8.04020051785475,-14.0007025637708));
#52018=CARTESIAN_POINT('Ctrl Pts',(6.94040491966306,-7.81754299922649,-14.0706916391873));
#52019=CARTESIAN_POINT('Ctrl Pts',(7.04958588954151,-7.56911744843866,-14.1659910151057));
#52020=CARTESIAN_POINT('Ctrl Pts',(7.09856303838754,-7.34590570822213,-14.2646458549881));
#52021=CARTESIAN_POINT('Ctrl Pts',(7.10550422945416,-7.21206930956354,-14.3297283067357));
#52022=CARTESIAN_POINT('Ctrl Pts',(7.10486447840068,-7.1618629058329,-14.35501317323));
#52023=CARTESIAN_POINT('Ctrl Pts',(6.05255921110257,-8.02911577078493,-13.4884779979374));
#52024=CARTESIAN_POINT('Ctrl Pts',(6.10163826062474,-8.00808629630007,-13.4850681496603));
#52025=CARTESIAN_POINT('Ctrl Pts',(6.20784989591504,-7.95404975929016,-13.4820617786761));
#52026=CARTESIAN_POINT('Ctrl Pts',(6.36880447954209,-7.84082091740601,-13.4935329138248));
#52027=CARTESIAN_POINT('Ctrl Pts',(6.52960557358651,-7.68309717847588,-13.527681476833));
#52028=CARTESIAN_POINT('Ctrl Pts',(6.66878769581625,-7.48587125691864,-13.5878974252917));
#52029=CARTESIAN_POINT('Ctrl Pts',(6.76721838514569,-7.26552280866674,-13.6710447620323));
#52030=CARTESIAN_POINT('Ctrl Pts',(6.81137640333751,-7.06770393936238,-13.7578157172582));
#52031=CARTESIAN_POINT('Ctrl Pts',(6.81761281966829,-6.94946218721919,-13.8152192041817));
#52032=CARTESIAN_POINT('Ctrl Pts',(6.81703837246853,-6.90519492478787,-13.8375220044062));
#52033=CARTESIAN_POINT('Ctrl Pts',(6.04144506586559,-8.08851582223875,-12.8459991592576));
#52034=CARTESIAN_POINT('Ctrl Pts',(6.10905976426781,-8.05997102346696,-12.8415739201359));
#52035=CARTESIAN_POINT('Ctrl Pts',(6.25426772822431,-7.98718898283285,-12.8382171896667));
#52036=CARTESIAN_POINT('Ctrl Pts',(6.47106155741839,-7.83717256794907,-12.8550776491995));
#52037=CARTESIAN_POINT('Ctrl Pts',(6.68448599491058,-7.63141480041554,-12.9018927977333));
#52038=CARTESIAN_POINT('Ctrl Pts',(6.86688747126734,-7.37739371601871,-12.9818716205382));
#52039=CARTESIAN_POINT('Ctrl Pts',(6.99483563759271,-7.09583628609421,-13.0900818015455));
#52040=CARTESIAN_POINT('Ctrl Pts',(7.05222134159964,-6.84322738167346,-13.2018442365124));
#52041=CARTESIAN_POINT('Ctrl Pts',(7.06042125079301,-6.69113539618814,-13.2758159416857));
#52042=CARTESIAN_POINT('Ctrl Pts',(7.05966442080613,-6.63389340780036,-13.304642630965));
#52043=CARTESIAN_POINT('Ctrl Pts',(6.22476564159013,-8.57073749841051,-12.4584449885852));
#52044=CARTESIAN_POINT('Ctrl Pts',(6.3232318544767,-8.52928566176545,-12.4525535946661));
#52045=CARTESIAN_POINT('Ctrl Pts',(6.53344505259971,-8.42415889175985,-12.4492269301855));
#52046=CARTESIAN_POINT('Ctrl Pts',(6.84361485042466,-8.21008811643112,-12.4765033513155));
#52047=CARTESIAN_POINT('Ctrl Pts',(7.14534003904336,-7.91995501597388,-12.5466286666515));
#52048=CARTESIAN_POINT('Ctrl Pts',(7.40049874768094,-7.56536280118761,-12.6625262804813));
#52049=CARTESIAN_POINT('Ctrl Pts',(7.57824979202421,-7.17474961980343,-12.8160459785316));
#52050=CARTESIAN_POINT('Ctrl Pts',(7.65795529133822,-6.82426150287073,-12.9727554779674));
#52051=CARTESIAN_POINT('Ctrl Pts',(7.66945774630811,-6.61179150649196,-13.0763256360123));
#52052=CARTESIAN_POINT('Ctrl Pts',(7.66839431346161,-6.53144498495453,-13.1167654130957));
#52053=CARTESIAN_POINT('',(7.00000000000021,-6.97709949620137,-13.9487329104921));
#52054=CARTESIAN_POINT('',(6.99999983297877,-8.0445005512629,-12.5220497591224));
#52055=CARTESIAN_POINT('Ctrl Pts',(7.,-6.97709949620152,-13.9487329104919));
#52056=CARTESIAN_POINT('Ctrl Pts',(7.,-7.02099172054913,-13.8471553853057));
#52057=CARTESIAN_POINT('Ctrl Pts',(7.,-7.06243364082271,-13.7568553945143));
#52058=CARTESIAN_POINT('Ctrl Pts',(7.,-7.10051939710644,-13.6792399036818));
#52059=CARTESIAN_POINT('Ctrl Pts',(7.,-7.1195622752483,-13.6404321582655));
#52060=CARTESIAN_POINT('Ctrl Pts',(7.,-7.13772767823402,-13.6047694443452));
#52061=CARTESIAN_POINT('Ctrl Pts',(7.,-7.15473399319081,-13.572301993779));
#52062=CARTESIAN_POINT('Ctrl Pts',(7.,-7.1632371506692,-13.5560682684958));
#52063=CARTESIAN_POINT('Ctrl Pts',(7.,-7.17144937268595,-13.5406322757568));
#52064=CARTESIAN_POINT('Ctrl Pts',(7.,-7.17933119800859,-13.5259946169535));
#52065=CARTESIAN_POINT('Ctrl Pts',(7.,-7.18327211066991,-13.5186757875519));
#52066=CARTESIAN_POINT('Ctrl Pts',(7.,-7.1871304241577,-13.5115565416342));
#52067=CARTESIAN_POINT('Ctrl Pts',(7.,-7.19090112056253,-13.5046366132084));
#52068=CARTESIAN_POINT('Ctrl Pts',(7.,-7.19278646876494,-13.5011766489955));
#52069=CARTESIAN_POINT('Ctrl Pts',(7.,-7.19464991269662,-13.4977665141556));
#52070=CARTESIAN_POINT('Ctrl Pts',(7.,-7.19649083259167,-13.4944061694443));
#52071=CARTESIAN_POINT('Ctrl Pts',(7.,-7.19833175248671,-13.4910458247329));
#52072=CARTESIAN_POINT('Ctrl Pts',(7.,-7.19934688844232,-13.4891942737903));
#52073=CARTESIAN_POINT('Ctrl Pts',(7.,-7.20194540134434,-13.4844744618343));
#52074=CARTESIAN_POINT('Ctrl Pts',(7.,-7.2435216077767,-13.4089574705386));
#52075=CARTESIAN_POINT('Ctrl Pts',(7.,-7.28577339769281,-13.3377261163259));
#52076=CARTESIAN_POINT('Ctrl Pts',(7.,-7.32833005782022,-13.2712688299823));
#52077=CARTESIAN_POINT('Ctrl Pts',(7.,-7.37088671794763,-13.2048115436386));
#52078=CARTESIAN_POINT('Ctrl Pts',(7.,-7.41277533743944,-13.1444121047124));
#52079=CARTESIAN_POINT('Ctrl Pts',(7.,-7.45594679397945,-13.0864207383147));
#52080=CARTESIAN_POINT('Ctrl Pts',(7.,-7.54228970705945,-12.9704380055194));
#52081=CARTESIAN_POINT('Ctrl Pts',(7.,-7.63586349310065,-12.8624797720249));
#52082=CARTESIAN_POINT('Ctrl Pts',(7.,-7.73523562504603,-12.7671941670015));
#52083=CARTESIAN_POINT('Ctrl Pts',(7.,-7.83460775699141,-12.6719085619781));
#52084=CARTESIAN_POINT('Ctrl Pts',(7.,-7.93958121382532,-12.589452238568));
#52085=CARTESIAN_POINT('Ctrl Pts',(7.,-8.04450023478728,-12.5220492664956));
#52086=CARTESIAN_POINT('',(6.24988067607176,-8.55172528393766,-12.4626549972234));
#52087=CARTESIAN_POINT('Ctrl Pts',(6.24994482956932,-8.55169717381052,-12.4626517783794));
#52088=CARTESIAN_POINT('Ctrl Pts',(6.29048458262229,-8.53403513767215,-12.4605545886541));
#52089=CARTESIAN_POINT('Ctrl Pts',(6.33134363509387,-8.51493349436176,-12.4591623965491));
#52090=CARTESIAN_POINT('Ctrl Pts',(6.37251646586922,-8.49423690369723,-12.4585572396575));
#52091=CARTESIAN_POINT('Ctrl Pts',(6.41368929664456,-8.47354031303271,-12.457952082766));
#52092=CARTESIAN_POINT('Ctrl Pts',(6.45517658069543,-8.45124860872904,-12.4581338983597));
#52093=CARTESIAN_POINT('Ctrl Pts',(6.49692908775461,-8.42718486597987,-12.4592076157083));
#52094=CARTESIAN_POINT('Ctrl Pts',(6.50031160745528,-8.4252353762449,-12.4592946013851));
#52095=CARTESIAN_POINT('Ctrl Pts',(6.50369585137872,-8.42327429550722,-12.4593874157455));
#52096=CARTESIAN_POINT('Ctrl Pts',(6.50708174191544,-8.42130154727401,-12.459486119114));
#52097=CARTESIAN_POINT('Ctrl Pts',(6.54999952146535,-8.39629602129426,-12.4607372314472));
#52098=CARTESIAN_POINT('Ctrl Pts',(6.59318572013806,-8.3694158784028,-12.4629336731219));
#52099=CARTESIAN_POINT('Ctrl Pts',(6.63647569728123,-8.34051133705735,-12.4661941145981));
#52100=CARTESIAN_POINT('Ctrl Pts',(6.67408360229115,-8.31540069212261,-12.46902660335));
#52101=CARTESIAN_POINT('Ctrl Pts',(6.71176939123371,-8.28876205909622,-12.4726622916301));
#52102=CARTESIAN_POINT('Ctrl Pts',(6.74939368103051,-8.26049889249528,-12.4771850108168));
#52103=CARTESIAN_POINT('Ctrl Pts',(6.77237300104314,-8.24323694938883,-12.4799472958214));
#52104=CARTESIAN_POINT('Ctrl Pts',(6.7953286993857,-8.22536928626321,-12.4830404776204));
#52105=CARTESIAN_POINT('Ctrl Pts',(6.818232101135,-8.20686687586236,-12.4864861196393));
#52106=CARTESIAN_POINT('Ctrl Pts',(6.85639403896923,-8.1760379255069,-12.4922272919754));
#52107=CARTESIAN_POINT('Ctrl Pts',(6.89441333319197,-8.14344663938261,-12.4989465132712));
#52108=CARTESIAN_POINT('Ctrl Pts',(6.9321382534014,-8.10896156348281,-12.5067449032162));
#52109=CARTESIAN_POINT('Ctrl Pts',(6.9548806557229,-8.08817229565011,-12.511446148987));
#52110=CARTESIAN_POINT('Ctrl Pts',(6.97751518344798,-8.06669475313748,-12.5165397978753));
#52111=CARTESIAN_POINT('Ctrl Pts',(6.99999949893631,-8.04450053061514,-12.5220497269843));
#52112=CARTESIAN_POINT('',(6.26382947399266,-8.42073790614957,-13.9442724045435));
#52113=CARTESIAN_POINT('Origin',(6.527587443497,-9.09528625386695,-13.2547537415242));
#52114=CARTESIAN_POINT('Ctrl Pts',(6.26386081927195,-8.42073287768038,-13.9442638625882));
#52115=CARTESIAN_POINT('Ctrl Pts',(6.30364635770537,-8.39476059044689,-13.9340836131071));
#52116=CARTESIAN_POINT('Ctrl Pts',(6.34318219371725,-8.36594610635673,-13.9248487614566));
#52117=CARTESIAN_POINT('Ctrl Pts',(6.38210302545369,-8.33427173662188,-13.9166477645883));
#52118=CARTESIAN_POINT('Ctrl Pts',(6.42102385719013,-8.30259736688704,-13.9084467677199));
#52119=CARTESIAN_POINT('Ctrl Pts',(6.4593294825228,-8.26806279443629,-13.9012800888418));
#52120=CARTESIAN_POINT('Ctrl Pts',(6.49663260666941,-8.230695113355,-13.8952081854052));
#52121=CARTESIAN_POINT('Ctrl Pts',(6.51075077335915,-8.21655251370995,-13.8929101434368));
#52122=CARTESIAN_POINT('Ctrl Pts',(6.52472513260001,-8.2020045811677,-13.8907685937496));
#52123=CARTESIAN_POINT('Ctrl Pts',(6.53853398200339,-8.1870546194782,-13.8887855340391));
#52124=CARTESIAN_POINT('Ctrl Pts',(6.57276742070081,-8.14999225591147,-13.8838693421791));
#52125=CARTESIAN_POINT('Ctrl Pts',(6.60598682438523,-8.11045658124235,-13.8799312016209));
#52126=CARTESIAN_POINT('Ctrl Pts',(6.6378660093174,-8.06853116995194,-13.8770019875818));
#52127=CARTESIAN_POINT('Ctrl Pts',(6.64639311847277,-8.05731687575912,-13.8762184754592));
#52128=CARTESIAN_POINT('Ctrl Pts',(6.65482425905276,-8.04593181774124,-13.8755069788649));
#52129=CARTESIAN_POINT('Ctrl Pts',(6.66315302408082,-8.0343780801965,-13.8748676892266));
#52130=CARTESIAN_POINT('Ctrl Pts',(6.68288623746992,-8.00700398960277,-13.8733530302335));
#52131=CARTESIAN_POINT('Ctrl Pts',(6.70204494706761,-7.97868286949254,-13.872244398396));
#52132=CARTESIAN_POINT('Ctrl Pts',(6.72054559570175,-7.9494469599469,-13.8715439793987));
#52133=CARTESIAN_POINT('Ctrl Pts',(6.72979592001882,-7.93482900517408,-13.8711937699));
#52134=CARTESIAN_POINT('Ctrl Pts',(6.73888182638716,-7.91998235042525,-13.8709456115201));
#52135=CARTESIAN_POINT('Ctrl Pts',(6.74779278023998,-7.90491194370508,-13.8707996343));
#52136=CARTESIAN_POINT('Ctrl Pts',(6.75224825716639,-7.89737674034499,-13.8707266456899));
#52137=CARTESIAN_POINT('Ctrl Pts',(6.75665999697761,-7.88978560334353,-13.8706791978952));
#52138=CARTESIAN_POINT('Ctrl Pts',(6.7610266857108,-7.88213918461823,-13.8706572814865));
#52139=CARTESIAN_POINT('Ctrl Pts',(6.76400979685793,-7.87691552011436,-13.8706423092532));
#52140=CARTESIAN_POINT('Ctrl Pts',(6.767263976232,-7.87114466561447,-13.8706383101171));
#52141=CARTESIAN_POINT('Ctrl Pts',(6.77018874126757,-7.86589465086422,-13.8706483529515));
#52142=CARTESIAN_POINT('Ctrl Pts',(6.77154525771907,-7.86345967530456,-13.870653010854));
#52143=CARTESIAN_POINT('Ctrl Pts',(6.77283150170764,-7.86113705674444,-13.8706602095793));
#52144=CARTESIAN_POINT('Ctrl Pts',(6.77399028875956,-7.85903475791193,-13.8706681031229));
#52145=CARTESIAN_POINT('Ctrl Pts',(6.79031634658572,-7.82941563828974,-13.8707793146253));
#52146=CARTESIAN_POINT('Ctrl Pts',(6.80638197979347,-7.79820326450054,-13.8712236235775));
#52147=CARTESIAN_POINT('Ctrl Pts',(6.8219998728032,-7.76535612977931,-13.8720923025352));
#52148=CARTESIAN_POINT('Ctrl Pts',(6.83722489386632,-7.73333527282491,-13.8729391296597));
#52149=CARTESIAN_POINT('Ctrl Pts',(6.85202408371635,-7.69976039894808,-13.8741898593545));
#52150=CARTESIAN_POINT('Ctrl Pts',(6.86618710318874,-7.66461800682303,-13.8759100776536));
#52151=CARTESIAN_POINT('Ctrl Pts',(6.87985159490252,-7.63071260078081,-13.8775697455472));
#52152=CARTESIAN_POINT('Ctrl Pts',(6.89292332203614,-7.59534777689527,-13.8796669331209));
#52153=CARTESIAN_POINT('Ctrl Pts',(6.90518551397339,-7.55854047945062,-13.8822346286123));
#52154=CARTESIAN_POINT('Ctrl Pts',(6.9139051923643,-7.53236670906778,-13.8840605239339));
#52155=CARTESIAN_POINT('Ctrl Pts',(6.92221488481856,-7.50546412122659,-13.8861238258106));
#52156=CARTESIAN_POINT('Ctrl Pts',(6.93003048544214,-7.47784944293239,-13.8884258882348));
#52157=CARTESIAN_POINT('Ctrl Pts',(6.94050147980807,-7.44085252423582,-13.89151008916));
#52158=CARTESIAN_POINT('Ctrl Pts',(6.95007987425218,-7.40257560652634,-13.8949948880792));
#52159=CARTESIAN_POINT('Ctrl Pts',(6.95858300270777,-7.36306946515618,-13.8989690474034));
#52160=CARTESIAN_POINT('Ctrl Pts',(6.96639277933585,-7.32678468583649,-13.9026191506294));
#52161=CARTESIAN_POINT('Ctrl Pts',(6.97329457265961,-7.28946289945377,-13.9066823481282));
#52162=CARTESIAN_POINT('Ctrl Pts',(6.97912057043595,-7.25117104072324,-13.9111965112778));
#52163=CARTESIAN_POINT('Ctrl Pts',(6.98481751717041,-7.21372738078283,-13.9156106816914));
#52164=CARTESIAN_POINT('Ctrl Pts',(6.98948502380683,-7.17535595748036,-13.9204564887435));
#52165=CARTESIAN_POINT('Ctrl Pts',(6.99295170328696,-7.13614918333898,-13.9257329552367));
#52166=CARTESIAN_POINT('Ctrl Pts',(6.99632248551628,-7.09802696918501,-13.9308634611258));
#52167=CARTESIAN_POINT('Ctrl Pts',(6.99855707282768,-7.05911499469893,-13.9364013240573));
#52168=CARTESIAN_POINT('Ctrl Pts',(6.99949624089758,-7.01952796744627,-13.942306371551));
#52169=CARTESIAN_POINT('Ctrl Pts',(6.99982980142646,-7.00546800291992,-13.9444036434113));
#52170=CARTESIAN_POINT('Ctrl Pts',(7.00000000252704,-6.99132316217677,-13.9465468520234));
#52171=CARTESIAN_POINT('Ctrl Pts',(7.00000000000032,-6.97709949620138,-13.9487329104922));
#52172=CARTESIAN_POINT('Ctrl Pts',(6.99990204209712,-6.87914456964441,-13.8881650018953));
#52173=CARTESIAN_POINT('Ctrl Pts',(6.99990204209712,-7.13651843302261,-14.0922367193011));
#52174=CARTESIAN_POINT('Ctrl Pts',(6.99990204209712,-7.80837710098112,-14.676030897134));
#52175=CARTESIAN_POINT('Ctrl Pts',(6.99990204209712,-8.78348255721519,-15.7555643069836));
#52176=CARTESIAN_POINT('Ctrl Pts',(6.99990204209712,-9.70999001325044,-17.1681336842782));
#52177=CARTESIAN_POINT('Ctrl Pts',(6.99990204209712,-10.4111885651775,-18.7078378782952));
#52178=CARTESIAN_POINT('Ctrl Pts',(6.99990204209712,-10.8675485943344,-20.3372599925577));
#52179=CARTESIAN_POINT('Ctrl Pts',(6.99990204209712,-11.0696762981163,-22.0150948612855));
#52180=CARTESIAN_POINT('Ctrl Pts',(6.99990204209712,-11.0250216793473,-23.3220419082231));
#52181=CARTESIAN_POINT('Ctrl Pts',(6.99990204209712,-10.9251645215214,-24.0577229990154));
#52182=CARTESIAN_POINT('Ctrl Pts',(6.99990204209712,-10.8963439108589,-24.2367456800396));
#52183=CARTESIAN_POINT('Ctrl Pts',(7.00657867940667,-7.1754747309625,-13.5144113065886));
#52184=CARTESIAN_POINT('Ctrl Pts',(7.00657867940667,-7.44407566709084,-13.7273830362199));
#52185=CARTESIAN_POINT('Ctrl Pts',(7.00657867940667,-8.14504949431156,-14.3364946131352));
#52186=CARTESIAN_POINT('Ctrl Pts',(7.00657867940667,-9.16238026129488,-15.4627618448717));
#52187=CARTESIAN_POINT('Ctrl Pts',(7.00657867940667,-10.1293833823756,-16.9370083185477));
#52188=CARTESIAN_POINT('Ctrl Pts',(7.00657867940667,-10.8609672539439,-18.5435648618307));
#52189=CARTESIAN_POINT('Ctrl Pts',(7.00657867940667,-11.3371716152691,-20.2436461281815));
#52190=CARTESIAN_POINT('Ctrl Pts',(7.00657867940667,-11.5480935350588,-21.9947648368347));
#52191=CARTESIAN_POINT('Ctrl Pts',(7.00657867940667,-11.5014977799429,-23.3582205168238));
#52192=CARTESIAN_POINT('Ctrl Pts',(7.00657867940667,-11.3973240256672,-24.1257634459938));
#52193=CARTESIAN_POINT('Ctrl Pts',(7.00657867940667,-11.3672534070212,-24.3125554713659));
#52194=CARTESIAN_POINT('Ctrl Pts',(6.71861277733521,-7.41191640291053,-13.2161934396482));
#52195=CARTESIAN_POINT('Ctrl Pts',(6.71861277733521,-7.68947541419458,-13.43626648412));
#52196=CARTESIAN_POINT('Ctrl Pts',(6.71861277733521,-8.41368021089695,-14.0655787997737));
#52197=CARTESIAN_POINT('Ctrl Pts',(6.71861277733521,-9.4647025299881,-15.2291349221608));
#52198=CARTESIAN_POINT('Ctrl Pts',(6.71861277733521,-10.4640171198348,-16.7525935169619));
#52199=CARTESIAN_POINT('Ctrl Pts',(6.71861277733521,-11.2198454211492,-18.4124915127807));
#52200=CARTESIAN_POINT('Ctrl Pts',(6.71861277733521,-11.7118835641508,-20.1689516775356));
#52201=CARTESIAN_POINT('Ctrl Pts',(6.71861277733521,-11.9298223840338,-21.978543521564));
#52202=CARTESIAN_POINT('Ctrl Pts',(6.71861277733521,-11.8816777972994,-23.3870874086374));
#52203=CARTESIAN_POINT('Ctrl Pts',(6.71861277733521,-11.7740598330902,-24.1800528810343));
#52204=CARTESIAN_POINT('Ctrl Pts',(6.71861277733521,-11.7429918337667,-24.3730440619698));
#52205=CARTESIAN_POINT('Ctrl Pts',(6.25720741184697,-7.48821447986154,-13.1199606158348));
#52206=CARTESIAN_POINT('Ctrl Pts',(6.25720741184697,-7.76866419946435,-13.3423252050321));
#52207=CARTESIAN_POINT('Ctrl Pts',(6.25720741184697,-8.50036546784203,-13.9781561580555));
#52208=CARTESIAN_POINT('Ctrl Pts',(6.25720741184697,-9.56225981559318,-15.1537451451436));
#52209=CARTESIAN_POINT('Ctrl Pts',(6.25720741184697,-10.5720010908474,-16.6930841478832));
#52210=CARTESIAN_POINT('Ctrl Pts',(6.25720741184697,-11.3356529003941,-18.3701950580588));
#52211=CARTESIAN_POINT('Ctrl Pts',(6.25720741184697,-11.8328004942073,-20.1448482997505));
#52212=CARTESIAN_POINT('Ctrl Pts',(6.25720741184697,-12.0530036187637,-21.973309016367));
#52213=CARTESIAN_POINT('Ctrl Pts',(6.25720741184697,-12.0043592348795,-23.3964025531034));
#52214=CARTESIAN_POINT('Ctrl Pts',(6.25720741184697,-11.8956298481708,-24.1975717027368));
#52215=CARTESIAN_POINT('Ctrl Pts',(6.25720741184697,-11.8642400010606,-24.392563307896));
#52216=CARTESIAN_POINT('Ctrl Pts',(7.00000000000032,-6.9770994962013,-13.9487329104922));
#52217=CARTESIAN_POINT('Ctrl Pts',(7.00000000000032,-7.10629915106168,-14.0533893975594));
#52218=CARTESIAN_POINT('Ctrl Pts',(6.99999999999072,-7.23274383645403,-14.1606500554492));
#52219=CARTESIAN_POINT('Ctrl Pts',(6.99999999940502,-7.35653276712002,-14.2705333166525));
#52220=CARTESIAN_POINT('Ctrl Pts',(6.99999999896232,-7.45009804601583,-14.353588060927));
#52221=CARTESIAN_POINT('Ctrl Pts',(6.99999999822524,-7.54214550930935,-14.4381420517995));
#52222=CARTESIAN_POINT('Ctrl Pts',(6.99999999797672,-7.63270518127864,-14.5242182514032));
#52223=CARTESIAN_POINT('Ctrl Pts',(6.99999999764697,-7.75286173493317,-14.6384260358524));
#52224=CARTESIAN_POINT('Ctrl Pts',(6.99999999919547,-7.8704006665934,-14.7553125453204));
#52225=CARTESIAN_POINT('Ctrl Pts',(6.99999999987686,-7.98538150041516,-14.874987097388));
#52226=CARTESIAN_POINT('Ctrl Pts',(6.99999999995253,-7.99815034808622,-14.8882771916991));
#52227=CARTESIAN_POINT('Ctrl Pts',(7.00000000000035,-8.01088760691926,-14.9016017031286));
#52228=CARTESIAN_POINT('Ctrl Pts',(7.00000000000035,-8.02359332727153,-14.9149608060427));
#52229=CARTESIAN_POINT('Ctrl Pts',(7.00000000000035,-8.16375185897403,-15.0623268897741));
#52230=CARTESIAN_POINT('Ctrl Pts',(6.99999999555914,-8.30011589105752,-15.2138319381572));
#52231=CARTESIAN_POINT('Ctrl Pts',(6.99999999493194,-8.43226901989482,-15.3691238080779));
#52232=CARTESIAN_POINT('Ctrl Pts',(6.99999999439975,-8.54440376184542,-15.500892264215));
#52233=CARTESIAN_POINT('Ctrl Pts',(6.99999999610764,-8.65350711581379,-15.6353863891432));
#52234=CARTESIAN_POINT('Ctrl Pts',(6.99999999794456,-8.75934547301326,-15.7723701876197));
#52235=CARTESIAN_POINT('Ctrl Pts',(6.99999999900022,-8.82017040022465,-15.8510942890886));
#52236=CARTESIAN_POINT('Ctrl Pts',(7.00000000000035,-8.87991734635779,-15.9306403281046));
#52237=CARTESIAN_POINT('Ctrl Pts',(7.00000000000035,-8.93855257173526,-16.0109543539319));
#52238=CARTESIAN_POINT('Ctrl Pts',(7.00000000000035,-9.09298167451233,-16.222479471625));
#52239=CARTESIAN_POINT('Ctrl Pts',(6.99999999747293,-9.23963260823544,-16.4393930418639));
#52240=CARTESIAN_POINT('Ctrl Pts',(6.99999999839252,-9.37832622087594,-16.6612166909058));
#52241=CARTESIAN_POINT('Ctrl Pts',(6.99999999909985,-9.48500722655949,-16.8318400492108));
#52242=CARTESIAN_POINT('Ctrl Pts',(6.99999999994394,-9.586979807279,-17.0053694008068));
#52243=CARTESIAN_POINT('Ctrl Pts',(6.9999999999955,-9.68414867194944,-17.1816028684607));
#52244=CARTESIAN_POINT('Ctrl Pts',(6.99999999999884,-9.69044102029951,-17.1930151904342));
#52245=CARTESIAN_POINT('Ctrl Pts',(7.00000000000035,-9.69671321993812,-17.2044388563421));
#52246=CARTESIAN_POINT('Ctrl Pts',(7.00000000000035,-9.70296524696087,-17.2158738099789));
#52247=CARTESIAN_POINT('Ctrl Pts',(7.00000000000035,-9.87477532000824,-17.5301143294911));
#52248=CARTESIAN_POINT('Ctrl Pts',(7.00000000000863,-10.0313678420663,-17.8528586248414));
#52249=CARTESIAN_POINT('Ctrl Pts',(6.99999999997898,-10.1718235720896,-18.1825334426912));
#52250=CARTESIAN_POINT('Ctrl Pts',(6.99999999996923,-10.2180173474565,-18.2909585277864));
#52251=CARTESIAN_POINT('Ctrl Pts',(7.00000000000035,-10.2624658168571,-18.4001328570506));
#52252=CARTESIAN_POINT('Ctrl Pts',(7.00000000000035,-10.3051367476958,-18.5099993257218));
#52253=CARTESIAN_POINT('Ctrl Pts',(7.00000000000035,-10.3319482521631,-18.5790319260819));
#52254=CARTESIAN_POINT('Ctrl Pts',(6.99999999997254,-10.3580605209726,-18.6483371267314));
#52255=CARTESIAN_POINT('Ctrl Pts',(6.99999999993318,-10.3834664693262,-18.717900541163));
#52256=CARTESIAN_POINT('Ctrl Pts',(6.99999999971942,-10.5214370739838,-19.0956745261202));
#52257=CARTESIAN_POINT('Ctrl Pts',(7.00000000000035,-10.6385722836543,-19.481064067169));
#52258=CARTESIAN_POINT('Ctrl Pts',(7.00000000000035,-10.7343171771693,-19.8715547121628));
#52259=CARTESIAN_POINT('Ctrl Pts',(7.00000000000035,-10.7726966551624,-20.0280834477003));
#52260=CARTESIAN_POINT('Ctrl Pts',(6.999999999624,-10.8076376867947,-20.1854325756873));
#52261=CARTESIAN_POINT('Ctrl Pts',(6.99999999912793,-10.8391038800975,-20.3434795187503));
#52262=CARTESIAN_POINT('Ctrl Pts',(6.99999999825573,-10.8944274489208,-20.621356186185));
#52263=CARTESIAN_POINT('Ctrl Pts',(6.99999999886898,-10.9390123595612,-20.901390595644));
#52264=CARTESIAN_POINT('Ctrl Pts',(6.99999999982073,-10.9726762049677,-21.1829159345384));
#52265=CARTESIAN_POINT('Ctrl Pts',(6.99999999992676,-10.9764265412553,-21.2142793952952));
#52266=CARTESIAN_POINT('Ctrl Pts',(7.00000000000035,-10.9800412819873,-21.2456613499309));
#52267=CARTESIAN_POINT('Ctrl Pts',(7.00000000000035,-10.9835201357179,-21.2770608676747));
#52268=CARTESIAN_POINT('Ctrl Pts',(7.00000000000035,-11.0078795682481,-21.4969247921714));
#52269=CARTESIAN_POINT('Ctrl Pts',(6.99999999634688,-11.0256228522879,-21.7176517758152));
#52270=CARTESIAN_POINT('Ctrl Pts',(6.99999999542235,-11.0366757131641,-21.9386334390376));
#52271=CARTESIAN_POINT('Ctrl Pts',(6.99999999531207,-11.0379941427253,-21.9649930178432));
#52272=CARTESIAN_POINT('Ctrl Pts',(6.99999999523666,-11.0392174373876,-21.991356219691));
#52273=CARTESIAN_POINT('Ctrl Pts',(6.99999999520114,-11.0403455207274,-22.0177220124615));
#52274=CARTESIAN_POINT('Ctrl Pts',(6.99999999489308,-11.050129574066,-22.2463968928441));
#52275=CARTESIAN_POINT('Ctrl Pts',(7.00000000000035,-11.0527466392745,-22.4752660514269));
#52276=CARTESIAN_POINT('Ctrl Pts',(7.00000000000035,-11.0482983184102,-22.7036608217722));
#52277=CARTESIAN_POINT('Ctrl Pts',(7.00000000000035,-11.044983466985,-22.8738586903776));
#52278=CARTESIAN_POINT('Ctrl Pts',(6.99999999741464,-11.0376888388909,-23.0437848171676));
#52279=CARTESIAN_POINT('Ctrl Pts',(6.99999999745767,-11.0264497943418,-23.2135396730414));
#52280=CARTESIAN_POINT('Ctrl Pts',(6.99999999749874,-11.0157217260455,-23.3755767287237));
#52281=CARTESIAN_POINT('Ctrl Pts',(6.99999999865165,-11.0013993941378,-23.5374580702059));
#52282=CARTESIAN_POINT('Ctrl Pts',(6.99999999924098,-10.9834692586181,-23.699270698839));
#52283=CARTESIAN_POINT('Ctrl Pts',(6.9999999997591,-10.9677053432543,-23.8415340174717));
#52284=CARTESIAN_POINT('Ctrl Pts',(6.99999999990897,-10.9491520894197,-23.9837444084844));
#52285=CARTESIAN_POINT('Ctrl Pts',(6.99999999989431,-10.9277733094969,-24.1259362010628));
#52286=CARTESIAN_POINT('Ctrl Pts',(6.26386085547009,-8.4207418582818,-13.9442726607693));
#52287=CARTESIAN_POINT('Ctrl Pts',(6.264607194611,-8.60590534760794,-14.1256751686954));
#52288=CARTESIAN_POINT('Ctrl Pts',(6.26531572513606,-8.78359556684554,-14.3114975773241));
#52289=CARTESIAN_POINT('Ctrl Pts',(6.26598642940395,-8.95375584024701,-14.5010992765559));
#52290=CARTESIAN_POINT('Ctrl Pts',(6.26666478024275,-9.12585607834021,-14.6928625884524));
#52291=CARTESIAN_POINT('Ctrl Pts',(6.26730443743229,-9.29025374785374,-14.8884918847937));
#52292=CARTESIAN_POINT('Ctrl Pts',(6.26790538606772,-9.44692290708507,-15.0873663300705));
#52293=CARTESIAN_POINT('Ctrl Pts',(6.26800179595848,-9.4720572623971,-15.1192716584363));
#52294=CARTESIAN_POINT('Ctrl Pts',(6.26809720958945,-9.49699277082847,-15.1512605953605));
#52295=CARTESIAN_POINT('Ctrl Pts',(6.26819162690635,-9.52172940099684,-15.1833306754945));
#52296=CARTESIAN_POINT('Ctrl Pts',(6.26876871801906,-9.67292295210862,-15.37934724149));
#52297=CARTESIAN_POINT('Ctrl Pts',(6.2693085884704,-9.81668511809778,-15.5783911664421));
#52298=CARTESIAN_POINT('Ctrl Pts',(6.26981122734859,-9.95309248242574,-15.7798081313912));
#52299=CARTESIAN_POINT('Ctrl Pts',(6.27017912980239,-10.0529347473803,-15.9272336467207));
#52300=CARTESIAN_POINT('Ctrl Pts',(6.27052708590838,-10.1488372020054,-16.0759315329076));
#52301=CARTESIAN_POINT('Ctrl Pts',(6.27085509217591,-10.2408366896114,-16.2256615039805));
#52302=CARTESIAN_POINT('Ctrl Pts',(6.27121137691842,-10.3407677488555,-16.3883001772955));
#52303=CARTESIAN_POINT('Ctrl Pts',(6.27154412300116,-10.4360937721226,-16.5521563516628));
#52304=CARTESIAN_POINT('Ctrl Pts',(6.27185332634397,-10.5268692976001,-16.7169398447424));
#52305=CARTESIAN_POINT('Ctrl Pts',(6.27227096778314,-10.6494799419672,-16.9395131668055));
#52306=CARTESIAN_POINT('Ctrl Pts',(6.2726456578957,-10.7637883511822,-17.1637762381474));
#52307=CARTESIAN_POINT('Ctrl Pts',(6.27297738874874,-10.869998798733,-17.3890720441409));
#52308=CARTESIAN_POINT('Ctrl Pts',(6.27330911960178,-10.9762092462838,-17.6143678501343));
#52309=CARTESIAN_POINT('Ctrl Pts',(6.27359789121449,-11.0743218171509,-17.8406965676868));
#52310=CARTESIAN_POINT('Ctrl Pts',(6.27384369779657,-11.1645575170758,-18.0674572453059));
#52311=CARTESIAN_POINT('Ctrl Pts',(6.27395596405333,-11.2057705072685,-18.171024742323));
#52312=CARTESIAN_POINT('Ctrl Pts',(6.27405926792789,-11.2453406153195,-18.2746831003251));
#52313=CARTESIAN_POINT('Ctrl Pts',(6.27415361604604,-11.2832899881317,-18.3783788192582));
#52314=CARTESIAN_POINT('Ctrl Pts',(6.27415652027611,-11.2844581482576,-18.381570787797));
#52315=CARTESIAN_POINT('Ctrl Pts',(6.27415941595948,-11.2856247726996,-18.384762791782));
#52316=CARTESIAN_POINT('Ctrl Pts',(6.27416230310198,-11.2867898621169,-18.3879548296995));
#52317=CARTESIAN_POINT('Ctrl Pts',(6.27420631246129,-11.3045495808973,-18.4366117781816));
#52318=CARTESIAN_POINT('Ctrl Pts',(6.27424833729733,-11.3219526271923,-18.4852766012743));
#52319=CARTESIAN_POINT('Ctrl Pts',(6.27428839822284,-11.3390022188445,-18.533943700428));
#52320=CARTESIAN_POINT('Ctrl Pts',(6.2743178500858,-11.3515366830508,-18.5697226225751));
#52321=CARTESIAN_POINT('Ctrl Pts',(6.27434670121203,-11.3640964164529,-18.6061334871817));
#52322=CARTESIAN_POINT('Ctrl Pts',(6.27437398744428,-11.3762332615428,-18.6418692456922));
#52323=CARTESIAN_POINT('Ctrl Pts',(6.27438625127513,-11.3816881815887,-18.6579307265802));
#52324=CARTESIAN_POINT('Ctrl Pts',(6.27439819898716,-11.387058352707,-18.673855597911));
#52325=CARTESIAN_POINT('Ctrl Pts',(6.27440974304166,-11.3923063239685,-18.6895241035388));
#52326=CARTESIAN_POINT('Ctrl Pts',(6.27456064715992,-11.4609079124125,-18.8943431318955));
#52327=CARTESIAN_POINT('Ctrl Pts',(6.27467736520998,-11.5248693955755,-19.1037511979344));
#52328=CARTESIAN_POINT('Ctrl Pts',(6.27475989545213,-11.5836609481629,-19.3175727645897));
#52329=CARTESIAN_POINT('Ctrl Pts',(6.27484107220331,-11.6414883228561,-19.5278876705287));
#52330=CARTESIAN_POINT('Ctrl Pts',(6.27488917331302,-11.6943139378734,-19.7424725854378));
#52331=CARTESIAN_POINT('Ctrl Pts',(6.27490419809794,-11.741610311925,-19.9611156276329));
#52332=CARTESIAN_POINT('Ctrl Pts',(6.27490863211128,-11.7555680993114,-20.025640089765));
#52333=CARTESIAN_POINT('Ctrl Pts',(6.2749101854529,-11.769044178975,-20.0905176757685));
#52334=CARTESIAN_POINT('Ctrl Pts',(6.2749088581209,-11.7820245987158,-20.155742159142));
#52335=CARTESIAN_POINT('Ctrl Pts',(6.27490450942711,-11.8245519171822,-20.369434969669));
#52336=CARTESIAN_POINT('Ctrl Pts',(6.27486923973871,-11.8617601976141,-20.5868549744431));
#52337=CARTESIAN_POINT('Ctrl Pts',(6.2748030495234,-11.8931694348145,-20.8077262448279));
#52338=CARTESIAN_POINT('Ctrl Pts',(6.27475277095458,-11.9170281197666,-20.9755016677541));
#52339=CARTESIAN_POINT('Ctrl Pts',(6.27468465115883,-11.9375403794305,-21.1452675639377));
#52340=CARTESIAN_POINT('Ctrl Pts',(6.27459869066247,-11.9544887837,-21.3168841110458));
#52341=CARTESIAN_POINT('Ctrl Pts',(6.27448994645919,-11.9759293383426,-21.5339873791369));
#52342=CARTESIAN_POINT('Ctrl Pts',(6.27435264982169,-11.9916670083741,-21.7540538870482));
#52343=CARTESIAN_POINT('Ctrl Pts',(6.27418680323014,-12.0012473071029,-21.9767610896342));
#52344=CARTESIAN_POINT('Ctrl Pts',(6.27401315364896,-12.0112783535429,-22.2099465418742));
#52345=CARTESIAN_POINT('Ctrl Pts',(6.27380820438329,-12.0145579268997,-22.4460271421446));
#52346=CARTESIAN_POINT('Ctrl Pts',(6.27357195921121,-12.0106606948055,-22.6846229983359));
#52347=CARTESIAN_POINT('Ctrl Pts',(6.2733393070839,-12.0068227355811,-22.9195900582934));
#52348=CARTESIAN_POINT('Ctrl Pts',(6.27307630376345,-11.9960245832477,-23.1569965027566));
#52349=CARTESIAN_POINT('Ctrl Pts',(6.27278295384919,-11.9778555569011,-23.3964293197048));
#52350=CARTESIAN_POINT('Ctrl Pts',(6.27261682316355,-11.9675660266934,-23.5320255346988));
#52351=CARTESIAN_POINT('Ctrl Pts',(6.2724409596977,-11.9549124215193,-23.6682707312012));
#52352=CARTESIAN_POINT('Ctrl Pts',(6.27225536444075,-11.9398195551922,-23.8050824682305));
#52353=CARTESIAN_POINT('Ctrl Pts',(6.27204648914279,-11.9228335233136,-23.9590551117422));
#52354=CARTESIAN_POINT('Ctrl Pts',(6.27182528752745,-11.9027579548588,-24.1137456145766));
#52355=CARTESIAN_POINT('Ctrl Pts',(6.27159176118789,-11.8794807211417,-24.2690119676562));
#52356=CARTESIAN_POINT('Ctrl Pts',(-6.390310997295,-8.1390337018704,-13.724647000479));
#52357=CARTESIAN_POINT('Ctrl Pts',(-4.26020733153,-9.11395737648274,-13.8218516500125));
#52358=CARTESIAN_POINT('Ctrl Pts',(0.0001535201484502,-10.0899905443268,
-13.9179732725499));
#52359=CARTESIAN_POINT('Ctrl Pts',(4.260514371827,-9.11388703213361,-13.8218447223658));
#52360=CARTESIAN_POINT('Ctrl Pts',(6.39077155774,-8.13882290112087,-13.7246259826053));
#52361=CARTESIAN_POINT('Ctrl Pts',(-6.390310997295,-8.71288713243719,-14.2540934475748));
#52362=CARTESIAN_POINT('Ctrl Pts',(-4.26020733153,-9.62694691866724,-14.3565346513067));
#52363=CARTESIAN_POINT('Ctrl Pts',(0.0001535201484502,-10.5423893454478,
-14.457603967021));
#52364=CARTESIAN_POINT('Ctrl Pts',(4.260514371827,-9.62688094118782,-14.3565273670688));
#52365=CARTESIAN_POINT('Ctrl Pts',(6.39077155774,-8.71268949185425,-14.2540712974373));
#52366=CARTESIAN_POINT('Ctrl Pts',(-6.390310997295,-9.96965830570771,-15.6639820761747));
#52367=CARTESIAN_POINT('Ctrl Pts',(-4.26020733153,-10.7489237306763,-15.7525575365657));
#52368=CARTESIAN_POINT('Ctrl Pts',(0.0001535201484502,-11.5272448903699,
-15.8420463049841));
#52369=CARTESIAN_POINT('Ctrl Pts',(4.260514371827,-10.7488676357646,-15.7525510869549));
#52370=CARTESIAN_POINT('Ctrl Pts',(6.39077155774,-9.96948981072532,-15.663962924145));
#52371=CARTESIAN_POINT('Ctrl Pts',(-6.390310997295,-11.3879809584937,-18.3168609125011));
#52372=CARTESIAN_POINT('Ctrl Pts',(-4.26020733153,-12.0191857141868,-18.3050659003902));
#52373=CARTESIAN_POINT('Ctrl Pts',(0.0001535201484502,-12.6510838649568,
-18.2929947853426));
#52374=CARTESIAN_POINT('Ctrl Pts',(4.260514371827,-12.019140172221,-18.3050667703783));
#52375=CARTESIAN_POINT('Ctrl Pts',(6.39077155774,-11.3878444776174,-18.3168634628551));
#52376=CARTESIAN_POINT('Ctrl Pts',(-6.390310997295,-12.0713625046932,-21.4528944523568));
#52377=CARTESIAN_POINT('Ctrl Pts',(-4.26020733153,-12.6592431520397,-21.2792418550437));
#52378=CARTESIAN_POINT('Ctrl Pts',(0.0001535201484502,-13.2456895514566,
-21.1056367718251));
#52379=CARTESIAN_POINT('Ctrl Pts',(4.260514371827,-12.6592008858621,-21.2792543670473));
#52380=CARTESIAN_POINT('Ctrl Pts',(6.39077155774,-12.0712353914676,-21.4529320000167));
#52381=CARTESIAN_POINT('Ctrl Pts',(-6.390310997295,-11.972049918498,-23.5459013792421));
#52382=CARTESIAN_POINT('Ctrl Pts',(-4.26020733153,-12.6077624045725,-23.2652611808828));
#52383=CARTESIAN_POINT('Ctrl Pts',(0.0001535201484502,-13.2461450674405,
-22.9846436057981));
#52384=CARTESIAN_POINT('Ctrl Pts',(4.260514371827,-12.6077163952593,-23.2652814054656));
#52385=CARTESIAN_POINT('Ctrl Pts',(6.39077155774,-11.9719124629745,-23.545962060063));
#52386=CARTESIAN_POINT('Ctrl Pts',(-6.390310997295,-11.8061921255752,-24.5118553802274));
#52387=CARTESIAN_POINT('Ctrl Pts',(-4.26020733153,-12.4817967099141,-24.1870632940561));
#52388=CARTESIAN_POINT('Ctrl Pts',(0.0001535201484502,-13.1582598604799,
-23.8622686316189));
#52389=CARTESIAN_POINT('Ctrl Pts',(4.260514371827,-12.4817479560743,-24.1870867025552));
#52390=CARTESIAN_POINT('Ctrl Pts',(6.39077155774,-11.8060460444555,-24.5119256076905));
#52391=CARTESIAN_POINT('Ctrl Pts',(-6.26383832463082,-8.42072097704164,
-13.9442592301454));
#52392=CARTESIAN_POINT('Ctrl Pts',(-5.97538166530715,-8.54511327803086,
-13.9555611456819));
#52393=CARTESIAN_POINT('Ctrl Pts',(-5.68507720580592,-8.66086372588226,
-13.9652304145446));
#52394=CARTESIAN_POINT('Ctrl Pts',(-5.39341281594673,-8.76784094219661,
-13.9735236289449));
#52395=CARTESIAN_POINT('Ctrl Pts',(-5.11950005635845,-8.86830718200011,
-13.9813120917165));
#52396=CARTESIAN_POINT('Ctrl Pts',(-4.8443878682284,-8.96103497709053,-13.9878870849323));
#52397=CARTESIAN_POINT('Ctrl Pts',(-4.56848035310862,-9.04595730735802,
-13.9934724196174));
#52398=CARTESIAN_POINT('Ctrl Pts',(-4.31195848006228,-9.12491287772086,
-13.9986653209937));
#52399=CARTESIAN_POINT('Ctrl Pts',(-4.05474911530607,-9.19712104882665,
-14.00300287132));
#52400=CARTESIAN_POINT('Ctrl Pts',(-3.79717702676898,-9.26257108423024,
-14.0066729478108));
#52401=CARTESIAN_POINT('Ctrl Pts',(-3.5773823659106,-9.3184217333297,-14.0098047437371));
#52402=CARTESIAN_POINT('Ctrl Pts',(-3.35732357810741,-9.36935171683099,
-14.0124506324332));
#52403=CARTESIAN_POINT('Ctrl Pts',(-3.13720246660799,-9.41538425106597,
-14.0147316531077));
#52404=CARTESIAN_POINT('Ctrl Pts',(-2.89762459074644,-9.46548565523124,
-14.0172142958869));
#52405=CARTESIAN_POINT('Ctrl Pts',(-2.65797161578867,-9.50979849671482,
-14.019280061851));
#52406=CARTESIAN_POINT('Ctrl Pts',(-2.41848996164712,-9.54830494866256,
-14.0209850915276));
#52407=CARTESIAN_POINT('Ctrl Pts',(-2.18234700883573,-9.58627456808007,
-14.0226663507619));
#52408=CARTESIAN_POINT('Ctrl Pts',(-1.94637063324644,-9.61859853128913,
-14.0239968819857));
#52409=CARTESIAN_POINT('Ctrl Pts',(-1.71079709151736,-9.64531020662259,
-14.0250352679962));
#52410=CARTESIAN_POINT('Ctrl Pts',(-1.47670514184955,-9.67185388428608,
-14.0260671232884));
#52411=CARTESIAN_POINT('Ctrl Pts',(-1.24301097489225,-9.69285557808708,
-14.0268105104645));
#52412=CARTESIAN_POINT('Ctrl Pts',(-1.0099464175956,-9.70839908468116,-14.0273274013437));
#52413=CARTESIAN_POINT('Ctrl Pts',(-0.778428527975858,-9.72383944114588,
-14.0278408620214));
#52414=CARTESIAN_POINT('Ctrl Pts',(-0.54753191928796,-9.73389378123307,
-14.0281308355323));
#52415=CARTESIAN_POINT('Ctrl Pts',(-0.317483833678931,-9.73869552910469,
-14.0282623090293));
#52416=CARTESIAN_POINT('Ctrl Pts',(-0.211730793665827,-9.74090289124577,
-14.0283227473587));
#52417=CARTESIAN_POINT('Ctrl Pts',(-0.106157066799982,-9.74200097364583,
-14.0283497487973));
#52418=CARTESIAN_POINT('Ctrl Pts',(-0.000784728634572568,-9.74200642998883,
-14.0283499195312));
#52419=CARTESIAN_POINT('Ctrl Pts',(-0.000523153662346578,-9.74200644353359,
-14.028349919955));
#52420=CARTESIAN_POINT('Ctrl Pts',(-0.000261577451239455,-9.74200645034681,
-14.0283499202138));
#52421=CARTESIAN_POINT('Ctrl Pts',(-1.58450436742064E-12,-9.74200645042823,
-14.0283499203075));
#52422=CARTESIAN_POINT('Ctrl Pts',(0.229838637557164,-9.74200652196735,
-14.0283500025861));
#52423=CARTESIAN_POINT('Ctrl Pts',(0.460633496507224,-9.73680495785485,
-14.0282222464573));
#52424=CARTESIAN_POINT('Ctrl Pts',(0.692159238285023,-9.72624319253679,
-14.0278992860365));
#52425=CARTESIAN_POINT('Ctrl Pts',(0.925512241714882,-9.71559807100703,
-14.0275737767278));
#52426=CARTESIAN_POINT('Ctrl Pts',(1.15960771013407,-9.69950781444332,-14.0270499565804));
#52427=CARTESIAN_POINT('Ctrl Pts',(1.39421492746824,-9.67786301061442,-14.0262631113473));
#52428=CARTESIAN_POINT('Ctrl Pts',(1.63029378402774,-9.65608243371467,-14.0254713304079));
#52429=CARTESIAN_POINT('Ctrl Pts',(1.86689082981409,-9.6286774638351,-14.0244132003187));
#52430=CARTESIAN_POINT('Ctrl Pts',(2.10377097976868,-9.59558948956167,-14.0230272818018));
#52431=CARTESIAN_POINT('Ctrl Pts',(2.34348947075129,-9.56210504916419,-14.0216247569571));
#52432=CARTESIAN_POINT('Ctrl Pts',(2.58349789095941,-9.52280064216678,-14.0198865221185));
#52433=CARTESIAN_POINT('Ctrl Pts',(2.82355260317888,-9.47766881045565,-14.017753756889));
#52434=CARTESIAN_POINT('Ctrl Pts',(2.92765742358338,-9.45809643384462,-14.0168288379857));
#52435=CARTESIAN_POINT('Ctrl Pts',(3.03177095016019,-9.43742875781944,-14.0158297824754));
#52436=CARTESIAN_POINT('Ctrl Pts',(3.13587331164792,-9.41566819115963,-14.0147520852401));
#52437=CARTESIAN_POINT('Ctrl Pts',(3.39867956582585,-9.36073367352787,-14.0120314401991));
#52438=CARTESIAN_POINT('Ctrl Pts',(3.66140879823393,-9.29881450311919,-14.0087907922733));
#52439=CARTESIAN_POINT('Ctrl Pts',(3.92371691757782,-9.2298741376027,-14.004824436216));
#52440=CARTESIAN_POINT('Ctrl Pts',(4.19327232811746,-9.15902902394007,-14.0007484940071));
#52441=CARTESIAN_POINT('Ctrl Pts',(4.4623830343311,-9.08076995842586,-13.9959061304099));
#52442=CARTESIAN_POINT('Ctrl Pts',(4.73067562905621,-8.99511737496303,-13.9900830109841));
#52443=CARTESIAN_POINT('Ctrl Pts',(5.02417182687565,-8.90141852499846,-13.9837128634492));
#52444=CARTESIAN_POINT('Ctrl Pts',(5.31668898549974,-8.79887209713146,-13.9761688159281));
#52445=CARTESIAN_POINT('Ctrl Pts',(5.60773826797885,-8.68756970498058,-13.9671831253586));
#52446=CARTESIAN_POINT('Ctrl Pts',(5.82734099413855,-8.60358973933271,-13.9604032352703));
#52447=CARTESIAN_POINT('Ctrl Pts',(6.04610805609104,-8.51462651729644,-13.9528028757534));
#52448=CARTESIAN_POINT('Ctrl Pts',(6.26382947399266,-8.42073790614957,-13.9442724045435));
#52449=CARTESIAN_POINT('Ctrl Pts',(-6.38263471220914,-8.36841944701316,
-13.9389824198947));
#52450=CARTESIAN_POINT('Ctrl Pts',(-6.32602239780459,-8.394139193293,-13.9420683564949));
#52451=CARTESIAN_POINT('Ctrl Pts',(-5.68511490691572,-8.68097899639166,
-13.976093651889));
#52452=CARTESIAN_POINT('Ctrl Pts',(-4.3452434520593,-9.18098161005785,-14.0268456230749));
#52453=CARTESIAN_POINT('Ctrl Pts',(-2.26201825060707,-9.6636131923873,-14.0637937745164));
#52454=CARTESIAN_POINT('Ctrl Pts',(-0.00125756887690166,-9.84171456782906,
-14.0745454197917));
#52455=CARTESIAN_POINT('Ctrl Pts',(2.25978796677181,-9.66398535327025,-14.0638181801999));
#52456=CARTESIAN_POINT('Ctrl Pts',(4.34366867832048,-9.18148899332632,-14.026891442955));
#52457=CARTESIAN_POINT('Ctrl Pts',(5.68433680181859,-8.68130836760525,-13.9761309988622));
#52458=CARTESIAN_POINT('Ctrl Pts',(6.32575507084932,-8.39426070532174,-13.942082936579));
#52459=CARTESIAN_POINT('Ctrl Pts',(6.38264695375981,-8.36841389164203,-13.938981748398));
#52460=CARTESIAN_POINT('Ctrl Pts',(-6.17942050080956,-7.96893940221161,
-13.4711461915673));
#52461=CARTESIAN_POINT('Ctrl Pts',(-6.12458159000237,-7.99369183810001,
-13.4742878091345));
#52462=CARTESIAN_POINT('Ctrl Pts',(-5.50375880491641,-8.2697463021422,-13.5089464493689));
#52463=CARTESIAN_POINT('Ctrl Pts',(-4.20607327283165,-8.75099127862432,
-13.5610724671584));
#52464=CARTESIAN_POINT('Ctrl Pts',(-2.18922025325704,-9.21546154338672,
-13.5997349748739));
#52465=CARTESIAN_POINT('Ctrl Pts',(-0.00121700010307547,-9.38682514547008,
-13.6112156728877));
#52466=CARTESIAN_POINT('Ctrl Pts',(2.18706140901595,-9.21581965563337,-13.5997608378893));
#52467=CARTESIAN_POINT('Ctrl Pts',(4.20454828183471,-8.75147962203571,-13.5611198620646));
#52468=CARTESIAN_POINT('Ctrl Pts',(5.5030051176246,-8.2700633023372,-13.5089845778398));
#52469=CARTESIAN_POINT('Ctrl Pts',(6.12432263701548,-7.99380877974493,-13.4743026523511));
#52470=CARTESIAN_POINT('Ctrl Pts',(6.17943235891975,-7.96893405529369,-13.4711455083109));
#52471=CARTESIAN_POINT('Ctrl Pts',(-6.17609323028145,-8.03335433234395,
-12.8276174364743));
#52472=CARTESIAN_POINT('Ctrl Pts',(-6.12140911242363,-8.05780395121941,
-12.8307280019944));
#52473=CARTESIAN_POINT('Ctrl Pts',(-5.50230415439753,-8.33050515234243,
-12.8650456140325));
#52474=CARTESIAN_POINT('Ctrl Pts',(-4.20735980031929,-8.80645453110351,
-12.916693548388));
#52475=CARTESIAN_POINT('Ctrl Pts',(-2.19139790985851,-9.26683779944148,
-12.955028315275));
#52476=CARTESIAN_POINT('Ctrl Pts',(-0.00121862788615356,-9.43699416114887,
-12.9664097316442));
#52477=CARTESIAN_POINT('Ctrl Pts',(2.18923837210851,-9.26719317059794,-12.9550539597772));
#52478=CARTESIAN_POINT('Ctrl Pts',(4.20583716474793,-8.80693793478961,-12.916740528662));
#52479=CARTESIAN_POINT('Ctrl Pts',(5.50155240772465,-8.33081840437701,-12.8650833759042));
#52480=CARTESIAN_POINT('Ctrl Pts',(6.12115089105302,-8.05791946224448,-12.8307426976662));
#52481=CARTESIAN_POINT('Ctrl Pts',(6.17610505478834,-8.03334905141697,-12.8276167590171));
#52482=CARTESIAN_POINT('Ctrl Pts',(-6.37328423761647,-8.51437156949978,
-12.4447843264679));
#52483=CARTESIAN_POINT('Ctrl Pts',(-6.31704477490063,-8.53938216381777,
-12.4477987971532));
#52484=CARTESIAN_POINT('Ctrl Pts',(-5.68027830641508,-8.81836853175587,
-12.4810393968647));
#52485=CARTESIAN_POINT('Ctrl Pts',(-4.34709680890174,-9.30595474822533,
-12.5306952467038));
#52486=CARTESIAN_POINT('Ctrl Pts',(-2.26647258115335,-9.7789738787803,-12.5668982241231));
#52487=CARTESIAN_POINT('Ctrl Pts',(-0.0012610105169752,-9.954224760735,
-12.5774258330699));
#52488=CARTESIAN_POINT('Ctrl Pts',(2.26424126928097,-9.7793395776048,-12.566922135523));
#52489=CARTESIAN_POINT('Ctrl Pts',(4.34552789319493,-9.30645053700893,-12.5307401190399));
#52490=CARTESIAN_POINT('Ctrl Pts',(5.67950489339072,-8.81868912212491,-12.4810759011191));
#52491=CARTESIAN_POINT('Ctrl Pts',(6.31677921013562,-8.53950032554409,-12.4478130376531));
#52492=CARTESIAN_POINT('Ctrl Pts',(6.37329639823823,-8.51436616865024,-12.4447836683068));
#52493=CARTESIAN_POINT('Ctrl Pts',(-6.24991282163701,-8.55170697043111,
-12.4626563115405));
#52494=CARTESIAN_POINT('Ctrl Pts',(-5.9951518486516,-8.66268534979844,-12.4758442934149));
#52495=CARTESIAN_POINT('Ctrl Pts',(-5.73646706502544,-8.76784866932984,
-12.4876291065261));
#52496=CARTESIAN_POINT('Ctrl Pts',(-5.47399786209961,-8.86673420580976,
-12.4981941489829));
#52497=CARTESIAN_POINT('Ctrl Pts',(-5.27446010051969,-8.94191025839756,
-12.5062260433892));
#52498=CARTESIAN_POINT('Ctrl Pts',(-5.07273572700998,-9.01345851273478,
-12.5135524815385));
#52499=CARTESIAN_POINT('Ctrl Pts',(-4.86889821251265,-9.0811859245181,-12.5202415502398));
#52500=CARTESIAN_POINT('Ctrl Pts',(-4.63291108368157,-9.1595954238162,-12.527985630721));
#52501=CARTESIAN_POINT('Ctrl Pts',(-4.3940912290919,-9.23288409034135,-12.5348755534569));
#52502=CARTESIAN_POINT('Ctrl Pts',(-4.15257087682656,-9.30077330239881,
-12.5409921785991));
#52503=CARTESIAN_POINT('Ctrl Pts',(-4.03181070069389,-9.33471790842754,
-12.5440504911702));
#52504=CARTESIAN_POINT('Ctrl Pts',(-3.91037570869951,-9.36731298118346,
-12.5469150648855));
#52505=CARTESIAN_POINT('Ctrl Pts',(-3.78828430791232,-9.39852576868662,
-12.5495933701623));
#52506=CARTESIAN_POINT('Ctrl Pts',(-3.72723860751873,-9.41413216243819,
-12.5509325228007));
#52507=CARTESIAN_POINT('Ctrl Pts',(-3.66602880391475,-9.42939298126246,
-12.5522251035111));
#52508=CARTESIAN_POINT('Ctrl Pts',(-3.60465734051059,-9.44430429742624,
-12.553471843025));
#52509=CARTESIAN_POINT('Ctrl Pts',(-3.57397160880851,-9.45175995550813,
-12.554095212782));
#52510=CARTESIAN_POINT('Ctrl Pts',(-3.54324546208646,-9.45912823768745,
-12.5547071219219));
#52511=CARTESIAN_POINT('Ctrl Pts',(-3.51247920955523,-9.46640865724988,
-12.5553076546463));
#52512=CARTESIAN_POINT('Ctrl Pts',(-3.49709608328961,-9.4700488670311,-12.5556079210085));
#52513=CARTESIAN_POINT('Ctrl Pts',(-3.48170293056752,-9.47366711114212,
-12.5559053432456));
#52514=CARTESIAN_POINT('Ctrl Pts',(-3.46629979054523,-9.47726332934056,
-12.5561999311267));
#52515=CARTESIAN_POINT('Ctrl Pts',(-3.45089665052293,-9.480859547539,-12.5564945190078));
#52516=CARTESIAN_POINT('Ctrl Pts',(-3.43752301160335,-9.4839640228018,-12.5567480657857));
#52517=CARTESIAN_POINT('Ctrl Pts',(-3.42006044787704,-9.48798584610345,
-12.557075201193));
#52518=CARTESIAN_POINT('Ctrl Pts',(-3.16496428844448,-9.54673733839557,
-12.5618540519572));
#52519=CARTESIAN_POINT('Ctrl Pts',(-2.9083995259039,-9.5990949307777,-12.5658854025021));
#52520=CARTESIAN_POINT('Ctrl Pts',(-2.65057545024978,-9.64488223466745,
-12.5693035076391));
#52521=CARTESIAN_POINT('Ctrl Pts',(-2.39508555341555,-9.69025500878651,
-12.5726906673782));
#52522=CARTESIAN_POINT('Ctrl Pts',(-2.13835912217894,-9.72917596851338,
-12.5754757356453));
#52523=CARTESIAN_POINT('Ctrl Pts',(-1.8806090149955,-9.76150571997245,-12.5777508730779));
#52524=CARTESIAN_POINT('Ctrl Pts',(-1.70382302984741,-9.78368009275444,
-12.5793113473558));
#52525=CARTESIAN_POINT('Ctrl Pts',(-1.5265556646053,-9.80275440615707,-12.5806311333328));
#52526=CARTESIAN_POINT('Ctrl Pts',(-1.34887783893452,-9.81869245723344,
-12.5817290231167));
#52527=CARTESIAN_POINT('Ctrl Pts',(-1.09250470695069,-9.84168963235498,
-12.5833131793917));
#52528=CARTESIAN_POINT('Ctrl Pts',(-0.835276744086408,-9.85815719512418,
-12.5844360222734));
#52529=CARTESIAN_POINT('Ctrl Pts',(-0.577412891913281,-9.86802180172397,
-12.5851131549729));
#52530=CARTESIAN_POINT('Ctrl Pts',(-0.385525226552946,-9.87536248291747,
-12.5856170387541));
#52531=CARTESIAN_POINT('Ctrl Pts',(-0.193285590508025,-9.87904741916114,
-12.5858732856714));
#52532=CARTESIAN_POINT('Ctrl Pts',(-0.00078636143307452,-9.87905785432159,
-12.5858736475182));
#52533=CARTESIAN_POINT('Ctrl Pts',(0.257720844642301,-9.8790718676981,-12.5858741334423));
#52534=CARTESIAN_POINT('Ctrl Pts',(0.515777038007509,-9.87245589781863,
-12.5854163540354));
#52535=CARTESIAN_POINT('Ctrl Pts',(0.773154488727125,-9.85925949667269,
-12.5845132529827));
#52536=CARTESIAN_POINT('Ctrl Pts',(1.03174709470167,-9.84600079140433,-12.5836058881221));
#52537=CARTESIAN_POINT('Ctrl Pts',(1.28965444445947,-9.82609939635818,-12.5822489670534));
#52538=CARTESIAN_POINT('Ctrl Pts',(1.54665177143313,-9.79963821643248,-12.5804148452328));
#52539=CARTESIAN_POINT('Ctrl Pts',(1.60560439865932,-9.79356828529937,-12.5799941159542));
#52540=CARTESIAN_POINT('Ctrl Pts',(1.66450916949929,-9.7871533139504,-12.579548108785));
#52541=CARTESIAN_POINT('Ctrl Pts',(1.72336342415286,-9.78039454216238,-12.5790761922448));
#52542=CARTESIAN_POINT('Ctrl Pts',(1.98197035651968,-9.75069634533781,-12.5770025802428));
#52543=CARTESIAN_POINT('Ctrl Pts',(2.23960128133811,-9.71435892567672,-12.574430876114));
#52544=CARTESIAN_POINT('Ctrl Pts',(2.49603560817474,-9.67151459029893,-12.5712774729064));
#52545=CARTESIAN_POINT('Ctrl Pts',(2.52259643111958,-9.66707688174331,-12.5709508513292));
#52546=CARTESIAN_POINT('Ctrl Pts',(2.54914442427194,-9.66256939409518,-12.5706179541918));
#52547=CARTESIAN_POINT('Ctrl Pts',(2.57567934791689,-9.65799229447821,-12.5702786645519));
#52548=CARTESIAN_POINT('Ctrl Pts',(2.71703894936703,-9.63360869397081,-12.56847116554));
#52549=CARTESIAN_POINT('Ctrl Pts',(2.85802756534812,-9.60724934697013,-12.5664824530093));
#52550=CARTESIAN_POINT('Ctrl Pts',(2.99860947845435,-9.57894193118977,-12.5642922890289));
#52551=CARTESIAN_POINT('Ctrl Pts',(3.06890043500747,-9.5647882232996,-12.5631972070388));
#52552=CARTESIAN_POINT('Ctrl Pts',(3.1390897140937,-9.55014749051982,-12.5620517520799));
#52553=CARTESIAN_POINT('Ctrl Pts',(3.20917295407369,-9.53502358563055,-12.5608529863025));
#52554=CARTESIAN_POINT('Ctrl Pts',(3.24421457406368,-9.52746163318592,-12.5602536034138));
#52555=CARTESIAN_POINT('Ctrl Pts',(3.27922968418995,-9.51977888728932,-12.559640892266));
#52556=CARTESIAN_POINT('Ctrl Pts',(3.31421774203385,-9.51197583874081,-12.5590144729994));
#52557=CARTESIAN_POINT('Ctrl Pts',(3.33171177095581,-9.50807431446657,-12.5587012633661));
#52558=CARTESIAN_POINT('Ctrl Pts',(3.34919903680103,-9.50414271450498,-12.558384626671));
#52559=CARTESIAN_POINT('Ctrl Pts',(3.36667947214295,-9.50018110159169,-12.5580645140084));
#52560=CARTESIAN_POINT('Ctrl Pts',(3.38415990748487,-9.49621948867839,-12.5577444013458));
#52561=CARTESIAN_POINT('Ctrl Pts',(3.40367174990795,-9.49175857405086,-12.5573826410032));
#52562=CARTESIAN_POINT('Ctrl Pts',(3.41910021933437,-9.48820628709549,-12.5570936987225));
#52563=CARTESIAN_POINT('Ctrl Pts',(3.68468645188544,-9.42705709054576,-12.5521198358181));
#52564=CARTESIAN_POINT('Ctrl Pts',(3.94732104507969,-9.35935398742538,-12.5463133571322));
#52565=CARTESIAN_POINT('Ctrl Pts',(4.20681520902679,-9.28542097652985,-12.5396050120407));
#52566=CARTESIAN_POINT('Ctrl Pts',(4.47313973337084,-9.20954191373872,-12.5327200910528));
#52567=CARTESIAN_POINT('Ctrl Pts',(4.7361562409857,-9.12710073431103,-12.5248850533555));
#52568=CARTESIAN_POINT('Ctrl Pts',(4.99568992142244,-9.03847547006321,-12.5159872135925));
#52569=CARTESIAN_POINT('Ctrl Pts',(5.13446019343343,-8.99108835635211,-12.5112296205042));
#52570=CARTESIAN_POINT('Ctrl Pts',(5.27223524686326,-8.9419337085792,-12.506167554481));
#52571=CARTESIAN_POINT('Ctrl Pts',(5.40899176766102,-8.89107233748081,-12.5007797956799));
#52572=CARTESIAN_POINT('Ctrl Pts',(5.67488604643662,-8.79218310348412,-12.4903044323681));
#52573=CARTESIAN_POINT('Ctrl Pts',(5.93692802123922,-8.68684255488974,-12.478598163806));
#52574=CARTESIAN_POINT('Ctrl Pts',(6.194971318514,-8.57552812461383,-12.4654727479179));
#52575=CARTESIAN_POINT('Ctrl Pts',(6.21329458554215,-8.56762385408414,-12.4645407318465));
#52576=CARTESIAN_POINT('Ctrl Pts',(6.23159770394303,-8.55968947309391,-12.4636015474238));
#52577=CARTESIAN_POINT('Ctrl Pts',(6.24988062747952,-8.55172515761025,-12.4626551215893));
#52578=CARTESIAN_POINT('Ctrl Pts',(7.10864015812303,-14.3702857527608,-7.14961345992433));
#52579=CARTESIAN_POINT('Ctrl Pts',(7.10873195145162,-14.3685405421865,-7.15305333563911));
#52580=CARTESIAN_POINT('Ctrl Pts',(7.11056295294098,-14.3266947300623,-7.23573122197125));
#52581=CARTESIAN_POINT('Ctrl Pts',(7.09575328823177,-14.2427614361485,-7.41145149599964));
#52582=CARTESIAN_POINT('Ctrl Pts',(7.015653292201,-14.1296722279313,-7.67994912051664));
#52583=CARTESIAN_POINT('Ctrl Pts',(6.86753480235506,-14.0345787862568,-7.94877408540477));
#52584=CARTESIAN_POINT('Ctrl Pts',(6.65756610531993,-13.97131600051,-8.18823799362193));
#52585=CARTESIAN_POINT('Ctrl Pts',(6.43827730135439,-13.9506144748102,-8.34979252916423));
#52586=CARTESIAN_POINT('Ctrl Pts',(6.29372111382291,-13.954903661422,-8.42179428876983));
#52587=CARTESIAN_POINT('Ctrl Pts',(6.24006895947315,-13.9586807624534,-8.44434194376808));
#52588=CARTESIAN_POINT('Ctrl Pts',(6.8141141961259,-13.8514991507047,-6.8948240391595));
#52589=CARTESIAN_POINT('Ctrl Pts',(6.81419627684994,-13.8499675766328,-6.89784015081079));
#52590=CARTESIAN_POINT('Ctrl Pts',(6.81583363961584,-13.8132441297087,-6.97034394335527));
#52591=CARTESIAN_POINT('Ctrl Pts',(6.80258372349459,-13.7395910455641,-7.12497917479021));
#52592=CARTESIAN_POINT('Ctrl Pts',(6.73069216203656,-13.6408694233877,-7.36194197355014));
#52593=CARTESIAN_POINT('Ctrl Pts',(6.59792593852943,-13.5588146206345,-7.59913721838558));
#52594=CARTESIAN_POINT('Ctrl Pts',(6.41046234837585,-13.5054525382864,-7.80983934257711));
#52595=CARTESIAN_POINT('Ctrl Pts',(6.21582986261128,-13.4892779790566,-7.95132463382177));
#52596=CARTESIAN_POINT('Ctrl Pts',(6.08830244526732,-13.4939767162925,-8.01411538505492));
#52597=CARTESIAN_POINT('Ctrl Pts',(6.04108479443307,-13.4975659796289,-8.03375561024937));
#52598=CARTESIAN_POINT('Ctrl Pts',(7.05418145102173,-13.3159705186763,-6.61710193690136));
#52599=CARTESIAN_POINT('Ctrl Pts',(7.0542892633488,-13.3139898936888,-6.62100630655558));
#52600=CARTESIAN_POINT('Ctrl Pts',(7.05643951679178,-13.2665094508432,-6.71482650170777));
#52601=CARTESIAN_POINT('Ctrl Pts',(7.03906592225061,-13.1717458506828,-6.91317869534412));
#52602=CARTESIAN_POINT('Ctrl Pts',(6.94574282526344,-13.0442863141664,-7.21546230643042));
#52603=CARTESIAN_POINT('Ctrl Pts',(6.77268167770971,-12.9366350636699,-7.51934219641006));
#52604=CARTESIAN_POINT('Ctrl Pts',(6.52525483088428,-12.8644440066539,-7.79272044859093));
#52605=CARTESIAN_POINT('Ctrl Pts',(6.26358458306018,-12.8408370822447,-7.97995451406243));
#52606=CARTESIAN_POINT('Ctrl Pts',(6.08889668952107,-12.8463947505128,-8.06469804500965));
#52607=CARTESIAN_POINT('Ctrl Pts',(6.02373779604539,-12.8510945065208,-8.09140233501099));
#52608=CARTESIAN_POINT('Ctrl Pts',(7.66687013380095,-13.1298707134944,-6.50628245672557));
#52609=CARTESIAN_POINT('Ctrl Pts',(7.66702167078277,-13.1270827140161,-6.5117850556935));
#52610=CARTESIAN_POINT('Ctrl Pts',(7.67004350237204,-13.0602569178355,-6.64396416362557));
#52611=CARTESIAN_POINT('Ctrl Pts',(7.64565946499919,-12.9272996711648,-6.92120542958822));
#52612=CARTESIAN_POINT('Ctrl Pts',(7.51579922451643,-12.7474722240711,-7.34139335357857));
#52613=CARTESIAN_POINT('Ctrl Pts',(7.27412336431642,-12.5929349937385,-7.76507343272806));
#52614=CARTESIAN_POINT('Ctrl Pts',(6.92493246816672,-12.4859435512758,-8.15007988493282));
#52615=CARTESIAN_POINT('Ctrl Pts',(6.54999801644743,-12.4479784492041,-8.4178655165686));
#52616=CARTESIAN_POINT('Ctrl Pts',(6.29594779154568,-12.4542588737833,-8.54084107185101));
#52617=CARTESIAN_POINT('Ctrl Pts',(6.20064104132926,-12.4606133626168,-8.57979107217853));
#52618=CARTESIAN_POINT('',(6.26385988969939,-13.9442649557967,-8.42071839556295));
#52619=CARTESIAN_POINT('',(6.24994527954487,-12.4626513729877,-8.55169284846167));
#52620=CARTESIAN_POINT('Ctrl Pts',(6.26385592204643,-13.9442753243737,-8.42070825250184));
#52621=CARTESIAN_POINT('Ctrl Pts',(6.25433094938681,-13.9218720248115,-8.4015324156922));
#52622=CARTESIAN_POINT('Ctrl Pts',(6.24498622483379,-13.8980075092444,-8.38293048695047));
#52623=CARTESIAN_POINT('Ctrl Pts',(6.23592366206991,-13.8726980683743,-8.36513067103791));
#52624=CARTESIAN_POINT('Ctrl Pts',(6.22708766500422,-13.8480213680756,-8.34777585372286));
#52625=CARTESIAN_POINT('Ctrl Pts',(6.21852019074842,-13.8219708232343,-8.3311842415144));
#52626=CARTESIAN_POINT('Ctrl Pts',(6.21032173905935,-13.7946096914538,-8.31557592497331));
#52627=CARTESIAN_POINT('Ctrl Pts',(6.20224970289332,-13.7676704529668,-8.30020827991192));
#52628=CARTESIAN_POINT('Ctrl Pts',(6.19453572189864,-13.7394606139546,-8.28579459549095));
#52629=CARTESIAN_POINT('Ctrl Pts',(6.18727710741677,-13.7100907636814,-8.27254267655098));
#52630=CARTESIAN_POINT('Ctrl Pts',(6.18014608857456,-13.6812371916651,-8.25952370662328));
#52631=CARTESIAN_POINT('Ctrl Pts',(6.1734549049804,-13.6512641756783,-8.24762677146337));
#52632=CARTESIAN_POINT('Ctrl Pts',(6.16729227922977,-13.6203252002813,-8.23703555362394));
#52633=CARTESIAN_POINT('Ctrl Pts',(6.16649544171368,-13.6163247405255,-8.23566609195988));
#52634=CARTESIAN_POINT('Ctrl Pts',(6.16570743204194,-13.612308196355,-8.23431843270015));
#52635=CARTESIAN_POINT('Ctrl Pts',(6.16492843297263,-13.608275957326,-8.23299294604334));
#52636=CARTESIAN_POINT('Ctrl Pts',(6.15899612350256,-13.5775692585389,-8.22289897115123));
#52637=CARTESIAN_POINT('Ctrl Pts',(6.15358731359049,-13.5459490871413,-8.21409328094374));
#52638=CARTESIAN_POINT('Ctrl Pts',(6.14877659384877,-13.5136112831753,-8.20672369077255));
#52639=CARTESIAN_POINT('Ctrl Pts',(6.14402750491138,-13.4816877633448,-8.19944851345313));
#52640=CARTESIAN_POINT('Ctrl Pts',(6.13986155259341,-13.4490654654329,-8.19357343054227));
#52641=CARTESIAN_POINT('Ctrl Pts',(6.13633723326726,-13.4159680839301,-8.1892066760389));
#52642=CARTESIAN_POINT('Ctrl Pts',(6.13283360983156,-13.383065060463,-8.18486556446525));
#52643=CARTESIAN_POINT('Ctrl Pts',(6.1299643255585,-13.3496932358894,-8.18201553851788));
#52644=CARTESIAN_POINT('Ctrl Pts',(6.12776995560997,-13.316097801226,-8.18072180153648));
#52645=CARTESIAN_POINT('Ctrl Pts',(6.1255830317919,-13.282616365567,-8.179432454578));
#52646=CARTESIAN_POINT('Ctrl Pts',(6.12406658849042,-13.2489136651176,-8.17968907655454));
#52647=CARTESIAN_POINT('Ctrl Pts',(6.12324125283879,-13.2152460979091,-8.18151036836834));
#52648=CARTESIAN_POINT('Ctrl Pts',(6.12241666034082,-13.1816088458528,-8.18333002024368));
#52649=CARTESIAN_POINT('Ctrl Pts',(6.12228197612596,-13.1480075395908,-8.18671153080457));
#52650=CARTESIAN_POINT('Ctrl Pts',(6.122836841893,-13.1146987316703,-8.19162595594638));
#52651=CARTESIAN_POINT('Ctrl Pts',(6.1233944112646,-13.0812276253159,-8.19656432681168));
#52652=CARTESIAN_POINT('Ctrl Pts',(6.12464822342135,-13.0480527410839,-8.20305039378025));
#52653=CARTESIAN_POINT('Ctrl Pts',(6.12657672595882,-13.0154220523358,-8.21100805179854));
#52654=CARTESIAN_POINT('Ctrl Pts',(6.12851268953151,-12.9826651212245,-8.21899649658821));
#52655=CARTESIAN_POINT('Ctrl Pts',(6.13112842257139,-12.9504573700935,-8.22846751325802));
#52656=CARTESIAN_POINT('Ctrl Pts',(6.13438230274582,-12.9190248592522,-8.2393018492621));
#52657=CARTESIAN_POINT('Ctrl Pts',(6.13767357069664,-12.8872311821651,-8.25026067409498));
#52658=CARTESIAN_POINT('Ctrl Pts',(6.14161751179079,-12.8562313109216,-8.26261375045333));
#52659=CARTESIAN_POINT('Ctrl Pts',(6.1461536325471,-12.8262230153038,-8.27620209831034));
#52660=CARTESIAN_POINT('Ctrl Pts',(6.1494575947754,-12.8043659527202,-8.2860994071512));
#52661=CARTESIAN_POINT('Ctrl Pts',(6.15307533149207,-12.7830341718204,-8.29665125444258));
#52662=CARTESIAN_POINT('Ctrl Pts',(6.15697892940399,-12.7622897446298,-8.3077874826303));
#52663=CARTESIAN_POINT('Ctrl Pts',(6.16243382819168,-12.7333014232692,-8.32334927946783));
#52664=CARTESIAN_POINT('Ctrl Pts',(6.16844710131043,-12.7054621437925,-8.34005240550776));
#52665=CARTESIAN_POINT('Ctrl Pts',(6.17493397014691,-12.6788987311741,-8.35769073070605));
#52666=CARTESIAN_POINT('Ctrl Pts',(6.18156923382221,-12.6517276489029,-8.37573255356872));
#52667=CARTESIAN_POINT('Ctrl Pts',(6.18869965656706,-12.625891567721,-8.39475204203223));
#52668=CARTESIAN_POINT('Ctrl Pts',(6.19622899598039,-12.6014723181196,-8.41452203315139));
#52669=CARTESIAN_POINT('Ctrl Pts',(6.20386985882546,-12.5766913743021,-8.43458485437609));
#52670=CARTESIAN_POINT('Ctrl Pts',(6.21192118959142,-12.5533693081249,-8.45541979900906));
#52671=CARTESIAN_POINT('Ctrl Pts',(6.22028225574658,-12.5315379646513,-8.47679504363041));
#52672=CARTESIAN_POINT('Ctrl Pts',(6.22884384657957,-12.5091830368603,-8.49868293388352));
#52673=CARTESIAN_POINT('Ctrl Pts',(6.23772988080328,-12.4883907997429,-8.52113665235221));
#52674=CARTESIAN_POINT('Ctrl Pts',(6.2468373203672,-12.4691443274329,-8.54392454922704));
#52675=CARTESIAN_POINT('Ctrl Pts',(6.24787065114139,-12.4669606212449,-8.54651006571107));
#52676=CARTESIAN_POINT('Ctrl Pts',(6.24890684035735,-12.4647967651974,-8.5490999082433));
#52677=CARTESIAN_POINT('Ctrl Pts',(6.24994574427476,-12.4626526982907,-8.55169375781615));
#52678=CARTESIAN_POINT('',(7.00000122821582,-12.5220660378628,-8.0444743030066));
#52679=CARTESIAN_POINT('Ctrl Pts',(7.00000132931107,-12.5220647920326,-8.04447409604749));
#52680=CARTESIAN_POINT('Ctrl Pts',(6.96887878389782,-12.5144347474821,-8.07520189714783));
#52681=CARTESIAN_POINT('Ctrl Pts',(6.93707075291002,-12.5075043810512,-8.10494973687714));
#52682=CARTESIAN_POINT('Ctrl Pts',(6.90460107002341,-12.5012608134835,-8.13374300551672));
#52683=CARTESIAN_POINT('Ctrl Pts',(6.86312146827392,-12.4932847363192,-8.17052603540976));
#52684=CARTESIAN_POINT('Ctrl Pts',(6.8205633372368,-12.4864286234133,-8.20575222368633));
#52685=CARTESIAN_POINT('Ctrl Pts',(6.77697281918209,-12.4806721578446,-8.23946237925169));
#52686=CARTESIAN_POINT('Ctrl Pts',(6.7350679148999,-12.4751382906317,-8.27186898750836));
#52687=CARTESIAN_POINT('Ctrl Pts',(6.69220821568608,-12.4706207026436,-8.30287475268951));
#52688=CARTESIAN_POINT('Ctrl Pts',(6.64840148631274,-12.4671221440221,-8.33249307237288));
#52689=CARTESIAN_POINT('Ctrl Pts',(6.60341126484273,-12.4635290675826,-8.36291156700114));
#52690=CARTESIAN_POINT('Ctrl Pts',(6.55744030090632,-12.4610077121262,-8.39186122162719));
#52691=CARTESIAN_POINT('Ctrl Pts',(6.51046156859088,-12.4595840347784,-8.41933237390026));
#52692=CARTESIAN_POINT('Ctrl Pts',(6.49869811470617,-12.4592275465974,-8.42621113833253));
#52693=CARTESIAN_POINT('Ctrl Pts',(6.48687134569449,-12.4589400147176,-8.43299702468925));
#52694=CARTESIAN_POINT('Ctrl Pts',(6.47498059517163,-12.4587221158036,-8.43968951496237));
#52695=CARTESIAN_POINT('Ctrl Pts',(6.42823118731504,-12.4578654293242,-8.46600155950091));
#52696=CARTESIAN_POINT('Ctrl Pts',(6.38049401611387,-12.4580829756919,-8.49087309509549));
#52697=CARTESIAN_POINT('Ctrl Pts',(6.33175355644512,-12.4594129782019,-8.51426069387726));
#52698=CARTESIAN_POINT('Ctrl Pts',(6.30479295496598,-12.4601486640753,-8.5271974559553));
#52699=CARTESIAN_POINT('Ctrl Pts',(6.27752508279713,-12.4612252038702,-8.53967947586593));
#52700=CARTESIAN_POINT('Ctrl Pts',(6.2499457442928,-12.4626526982629,-8.55169375784748));
#52701=CARTESIAN_POINT('',(6.99999966028467,-13.9486981671726,-6.97711506156621));
#52702=CARTESIAN_POINT('Ctrl Pts',(6.999999755579,-13.9486981671724,-6.97711506157905));
#52703=CARTESIAN_POINT('Ctrl Pts',(7.,-13.8626463334129,-7.01419856109545));
#52704=CARTESIAN_POINT('Ctrl Pts',(7.,-13.7400684821722,-7.07011204123475));
#52705=CARTESIAN_POINT('Ctrl Pts',(7.,-13.6272404800293,-7.12645786767111));
#52706=CARTESIAN_POINT('Ctrl Pts',(7.,-13.5541884450668,-7.1641178289169));
#52707=CARTESIAN_POINT('Ctrl Pts',(7.,-13.520579782048,-7.1819856114406));
#52708=CARTESIAN_POINT('Ctrl Pts',(7.,-13.339612670826,-7.28166708221286));
#52709=CARTESIAN_POINT('Ctrl Pts',(7.,-13.2055611610638,-7.36745032586629));
#52710=CARTESIAN_POINT('Ctrl Pts',(7.,-12.8482255802639,-7.63349426885588));
#52711=CARTESIAN_POINT('Ctrl Pts',(7.,-12.6600978814924,-7.8296083475282));
#52712=CARTESIAN_POINT('Ctrl Pts',(7.000002769617,-12.5220662044828,-8.04447387621312));
#52713=CARTESIAN_POINT('Ctrl Pts',(6.99999922604724,-13.9486981671804,-6.97711506153452));
#52714=CARTESIAN_POINT('Ctrl Pts',(6.99999541671456,-13.9418949807255,-7.02119365462051));
#52715=CARTESIAN_POINT('Ctrl Pts',(6.99835381561817,-13.9356151148029,-7.06425756057063));
#52716=CARTESIAN_POINT('Ctrl Pts',(6.9953485697528,-13.9298432802271,-7.10615136253393));
#52717=CARTESIAN_POINT('Ctrl Pts',(6.99234332388744,-13.9240714456514,-7.14804516449724));
#52718=CARTESIAN_POINT('Ctrl Pts',(6.98797379154531,-13.9188076897555,-7.18876918020147));
#52719=CARTESIAN_POINT('Ctrl Pts',(6.98248007277824,-13.9140314092665,-7.22820843471191));
#52720=CARTESIAN_POINT('Ctrl Pts',(6.97660699910893,-13.9089253147672,-7.27037106753371));
#52721=CARTESIAN_POINT('Ctrl Pts',(6.96944999946155,-13.9043759886361,-7.31106590392677));
#52722=CARTESIAN_POINT('Ctrl Pts',(6.96130496881929,-13.900335688588,-7.35021802520771));
#52723=CARTESIAN_POINT('Ctrl Pts',(6.9554290548961,-13.8974209720756,-7.3784627924359));
#52724=CARTESIAN_POINT('Ctrl Pts',(6.94903794299284,-13.8947711282211,-7.4059054976004));
#52725=CARTESIAN_POINT('Ctrl Pts',(6.94223029680783,-13.8923674055314,-7.43252906388036));
#52726=CARTESIAN_POINT('Ctrl Pts',(6.93362366105249,-13.8893284747345,-7.46618817765514));
#52727=CARTESIAN_POINT('Ctrl Pts',(6.92435173757794,-13.8866830002541,-7.49853750694693));
#52728=CARTESIAN_POINT('Ctrl Pts',(6.91459419318944,-13.8843912896279,-7.52956122924081));
#52729=CARTESIAN_POINT('Ctrl Pts',(6.90281862571623,-13.8816256149834,-7.56700117525552));
#52730=CARTESIAN_POINT('Ctrl Pts',(6.89033747519103,-13.8793747431416,-7.60251052333689));
#52731=CARTESIAN_POINT('Ctrl Pts',(6.87745399509062,-13.87755326155,-7.63611118024047));
#52732=CARTESIAN_POINT('Ctrl Pts',(6.86947771174407,-13.8764255652154,-7.65691366202369));
#52733=CARTESIAN_POINT('Ctrl Pts',(6.86134622163443,-13.8754624935046,-7.67698512013817));
#52734=CARTESIAN_POINT('Ctrl Pts',(6.8531229005019,-13.8746441171068,-7.69633557749649));
#52735=CARTESIAN_POINT('Ctrl Pts',(6.84770422519965,-13.8741048561557,-7.70908636804509));
#52736=CARTESIAN_POINT('Ctrl Pts',(6.84224554756976,-13.8736284270604,-7.72152417125158));
#52737=CARTESIAN_POINT('Ctrl Pts',(6.8367636178037,-13.8732091805885,-7.7336526079316));
#52738=CARTESIAN_POINT('Ctrl Pts',(6.83402265292067,-13.8729995573526,-7.73971682627161));
#52739=CARTESIAN_POINT('Ctrl Pts',(6.83127586601031,-13.8728042342134,-7.74570369902245));
#52740=CARTESIAN_POINT('Ctrl Pts',(6.82852524644297,-13.872622504644,-7.75161374361826));
#52741=CARTESIAN_POINT('Ctrl Pts',(6.82714993665931,-13.8725316398593,-7.75456876591616));
#52742=CARTESIAN_POINT('Ctrl Pts',(6.82577366815407,-13.8724441737331,-7.75750458093883));
#52743=CARTESIAN_POINT('Ctrl Pts',(6.82439668502147,-13.8723600188195,-7.76042125420104));
#52744=CARTESIAN_POINT('Ctrl Pts',(6.82331719844689,-13.8722940455355,-7.76270778157706));
#52745=CARTESIAN_POINT('Ctrl Pts',(6.82270593100578,-13.8722577027424,-7.76399798722328));
#52746=CARTESIAN_POINT('Ctrl Pts',(6.82146136860573,-13.8721857550262,-7.76660776827813));
#52747=CARTESIAN_POINT('Ctrl Pts',(6.82111837867054,-13.8721659268982,-7.76732699990109));
#52748=CARTESIAN_POINT('Ctrl Pts',(6.82072709486732,-13.8721434920848,-7.7681463433998));
#52749=CARTESIAN_POINT('Ctrl Pts',(6.82026383294919,-13.8721174008885,-7.76911391468128));
#52750=CARTESIAN_POINT('Ctrl Pts',(6.80986980584361,-13.8715320028847,-7.79082293442298));
#52751=CARTESIAN_POINT('Ctrl Pts',(6.79910043570059,-13.8711237960025,-7.81218975557005));
#52752=CARTESIAN_POINT('Ctrl Pts',(6.78797479033902,-13.8708967998656,-7.83319651415722));
#52753=CARTESIAN_POINT('Ctrl Pts',(6.75802589931483,-13.8702857537334,-7.88974416629362));
#52754=CARTESIAN_POINT('Ctrl Pts',(6.7254993938176,-13.8709862004088,-7.9436820906596));
#52755=CARTESIAN_POINT('Ctrl Pts',(6.69085594874757,-13.8730137832032,-7.99475942931483));
#52756=CARTESIAN_POINT('Ctrl Pts',(6.66371766412754,-13.8746021101971,-8.03477136667432));
#52757=CARTESIAN_POINT('Ctrl Pts',(6.63527897360461,-13.8770054109227,-8.07302800792033));
#52758=CARTESIAN_POINT('Ctrl Pts',(6.6057412909821,-13.8802385643642,-8.10941412831148));
#52759=CARTESIAN_POINT('Ctrl Pts',(6.56617721821083,-13.8845691924528,-8.1581513001952));
#52760=CARTESIAN_POINT('Ctrl Pts',(6.5246436408946,-13.8903876497457,-8.20353270811691));
#52761=CARTESIAN_POINT('Ctrl Pts',(6.4816917663355,-13.8976560231946,-8.24539866607507));
#52762=CARTESIAN_POINT('Ctrl Pts',(6.44899683080048,-13.9031887037539,-8.2772670026868));
#52763=CARTESIAN_POINT('Ctrl Pts',(6.41547887539951,-13.9095620771806,-8.30709844682416));
#52764=CARTESIAN_POINT('Ctrl Pts',(6.3813625868749,-13.9167654813743,-8.33482743069761));
#52765=CARTESIAN_POINT('Ctrl Pts',(6.34283815341129,-13.924899633053,-8.36613925975182));
#52766=CARTESIAN_POINT('Ctrl Pts',(6.30355145233289,-13.9340917614948,-8.39477063371972));
#52767=CARTESIAN_POINT('Ctrl Pts',(6.26385592205553,-13.9442753243951,-8.42070825252017));
#52768=CARTESIAN_POINT('Ctrl Pts',(6.99933866941448,-24.2330493766941,-10.874321862056));
#52769=CARTESIAN_POINT('Ctrl Pts',(6.99933866941448,-24.1955798273609,-10.8803485970913));
#52770=CARTESIAN_POINT('Ctrl Pts',(6.99933866941448,-23.5851351123061,-10.9752955968351));
#52771=CARTESIAN_POINT('Ctrl Pts',(6.99933866941448,-22.3847684638752,-11.0599204357608));
#52772=CARTESIAN_POINT('Ctrl Pts',(6.99933866941448,-20.6450473295107,-10.9047318327807));
#52773=CARTESIAN_POINT('Ctrl Pts',(6.99933866941448,-18.9490871085038,-10.4757466588859));
#52774=CARTESIAN_POINT('Ctrl Pts',(6.99933866941448,-17.342462236957,-9.7823271357614));
#52775=CARTESIAN_POINT('Ctrl Pts',(6.99933866941448,-15.8669670639865,-8.8443674600905));
#52776=CARTESIAN_POINT('Ctrl Pts',(6.99933866941448,-14.734489189311,-7.83889823066968));
#52777=CARTESIAN_POINT('Ctrl Pts',(6.99933866941448,-14.1224323389474,-7.13859596735225));
#52778=CARTESIAN_POINT('Ctrl Pts',(6.99933866941448,-13.9057057528166,-6.86526372147669));
#52779=CARTESIAN_POINT('Ctrl Pts',(7.01704755924886,-24.310389917853,-11.3548276333142));
#52780=CARTESIAN_POINT('Ctrl Pts',(7.01704755924886,-24.2712580736605,-11.3611213667568));
#52781=CARTESIAN_POINT('Ctrl Pts',(7.01704755924886,-23.6337446446486,-11.4602748689665));
#52782=CARTESIAN_POINT('Ctrl Pts',(7.01704755924886,-22.3805064854811,-11.5486515701702));
#52783=CARTESIAN_POINT('Ctrl Pts',(7.01704755924886,-20.5629013815418,-11.3865346008396));
#52784=CARTESIAN_POINT('Ctrl Pts',(7.01704755924886,-18.7919623591938,-10.9385361771176));
#52785=CARTESIAN_POINT('Ctrl Pts',(7.01704755924886,-17.1138140330456,-10.2143156875747));
#52786=CARTESIAN_POINT('Ctrl Pts',(7.01704755924886,-15.5725993502725,-9.23452321255108));
#52787=CARTESIAN_POINT('Ctrl Pts',(7.01704755924886,-14.3899029550477,-8.18446712170575));
#52788=CARTESIAN_POINT('Ctrl Pts',(7.01704755924886,-13.7507244922113,-7.45315527481836));
#52789=CARTESIAN_POINT('Ctrl Pts',(7.01704755924886,-13.5243359009936,-7.1676330973788));
#52790=CARTESIAN_POINT('Ctrl Pts',(6.72711815520593,-24.3727491957856,-11.7422569490181));
#52791=CARTESIAN_POINT('Ctrl Pts',(6.72711815520593,-24.3322770518609,-11.7487659618967));
#52792=CARTESIAN_POINT('Ctrl Pts',(6.72711815520593,-23.6729382589067,-11.8513111452604));
#52793=CARTESIAN_POINT('Ctrl Pts',(6.72711815520593,-22.3770700743642,-11.9427129535966));
#52794=CARTESIAN_POINT('Ctrl Pts',(6.72711815520593,-20.4966675289803,-11.7750096783504));
#52795=CARTESIAN_POINT('Ctrl Pts',(6.72711815520593,-18.6652734872849,-11.3116809697256));
#52796=CARTESIAN_POINT('Ctrl Pts',(6.72711815520593,-16.9294561699855,-10.562625820423));
#52797=CARTESIAN_POINT('Ctrl Pts',(6.72711815520593,-15.335252186698,-9.54910377585614));
#52798=CARTESIAN_POINT('Ctrl Pts',(6.72711815520593,-14.1120648583422,-8.46309752947625));
#52799=CARTESIAN_POINT('Ctrl Pts',(6.72711815520593,-13.451018379787,-7.70678281590056));
#52800=CARTESIAN_POINT('Ctrl Pts',(6.72711815520593,-13.216839363892,-7.41143195975148));
#52801=CARTESIAN_POINT('Ctrl Pts',(6.25441317313844,-24.3925105190614,-11.865031237121));
#52802=CARTESIAN_POINT('Ctrl Pts',(6.25441317313844,-24.3516136412845,-11.8716084709059));
#52803=CARTESIAN_POINT('Ctrl Pts',(6.25441317313844,-23.6853585066674,-11.975228459979));
#52804=CARTESIAN_POINT('Ctrl Pts',(6.25441317313844,-22.3759810939704,-12.0675889086622));
#52805=CARTESIAN_POINT('Ctrl Pts',(6.25441317313844,-20.4756783736281,-11.8981153628051));
#52806=CARTESIAN_POINT('Ctrl Pts',(6.25441317313844,-18.6251264580638,-11.4299285684873));
#52807=CARTESIAN_POINT('Ctrl Pts',(6.25441317313844,-16.8710341444066,-10.6730034476867));
#52808=CARTESIAN_POINT('Ctrl Pts',(6.25441317313844,-15.2600381338117,-9.64879268205177));
#52809=CARTESIAN_POINT('Ctrl Pts',(6.25441317313844,-14.0240194442555,-8.55139402272411));
#52810=CARTESIAN_POINT('Ctrl Pts',(6.25441317313844,-13.3560431079106,-7.78715603376997));
#52811=CARTESIAN_POINT('Ctrl Pts',(6.25441317313844,-13.1193953478972,-7.48869052164871));
#52812=CARTESIAN_POINT('',(7.00000000000001,-24.1259420764689,-10.9277801898196));
#52813=CARTESIAN_POINT('Ctrl Pts',(7.00000000000006,-24.1259420781412,-10.9277802009505));
#52814=CARTESIAN_POINT('Ctrl Pts',(7.00000000000006,-23.9636071725167,-10.9521697295806));
#52815=CARTESIAN_POINT('Ctrl Pts',(7.00000000006077,-23.8012468908441,-10.9728907817485));
#52816=CARTESIAN_POINT('Ctrl Pts',(6.99999999867347,-23.6387646052866,-10.9899916559832));
#52817=CARTESIAN_POINT('Ctrl Pts',(6.99999999728333,-23.4759487464894,-11.0071276380083));
#52818=CARTESIAN_POINT('Ctrl Pts',(6.99999999422996,-23.3130099247608,-11.0206285810807));
#52819=CARTESIAN_POINT('Ctrl Pts',(6.99999999314807,-23.1498445645076,-11.0304911277965));
#52820=CARTESIAN_POINT('Ctrl Pts',(6.99999999206999,-22.9872534292042,-11.0403189654271));
#52821=CARTESIAN_POINT('Ctrl Pts',(6.9999999947222,-22.8244368951336,-11.0465339705941));
#52822=CARTESIAN_POINT('Ctrl Pts',(6.99999999803545,-22.66129298247,-11.0490812192144));
#52823=CARTESIAN_POINT('Ctrl Pts',(6.99999999907237,-22.6102350557993,-11.0498784125092));
#52824=CARTESIAN_POINT('Ctrl Pts',(7.00000000000006,-22.5591450946315,-11.0503159841132));
#52825=CARTESIAN_POINT('Ctrl Pts',(7.00000000000006,-22.508020091487,-11.0503912041561));
#52826=CARTESIAN_POINT('Ctrl Pts',(7.00000000000006,-22.4670935981955,-11.0504514191662));
#52827=CARTESIAN_POINT('Ctrl Pts',(6.99999999938403,-22.4261442171024,-11.050284473563));
#52828=CARTESIAN_POINT('Ctrl Pts',(6.99999999847206,-22.3851771719375,-11.0498891036845));
#52829=CARTESIAN_POINT('Ctrl Pts',(6.99999999416113,-22.1915245001741,-11.0480201762823));
#52830=CARTESIAN_POINT('Ctrl Pts',(6.99999998574668,-21.9974766397739,-11.0410429983301));
#52831=CARTESIAN_POINT('Ctrl Pts',(6.99999998500523,-21.8035275617183,-11.0289287826417));
#52832=CARTESIAN_POINT('Ctrl Pts',(6.99999998426222,-21.6091684925747,-11.0167889585797));
#52833=CARTESIAN_POINT('Ctrl Pts',(6.99999998984227,-21.4149090420865,-10.9994903474823));
#52834=CARTESIAN_POINT('Ctrl Pts',(6.99999999473006,-21.2212489723544,-10.9770562251537));
#52835=CARTESIAN_POINT('Ctrl Pts',(6.99999999759815,-21.1076118068151,-10.9638921791203));
#52836=CARTESIAN_POINT('Ctrl Pts',(7.00000000000006,-20.9941810379534,-10.948960864708));
#52837=CARTESIAN_POINT('Ctrl Pts',(7.00000000000006,-20.8810571711621,-10.9322753272691));
#52838=CARTESIAN_POINT('Ctrl Pts',(7.00000000000006,-20.803036582786,-10.9207674511217));
#52839=CARTESIAN_POINT('Ctrl Pts',(6.99999999890224,-20.7251635517596,-10.908419020453));
#52840=CARTESIAN_POINT('Ctrl Pts',(6.99999999758216,-20.6474486195687,-10.8952326698618));
#52841=CARTESIAN_POINT('Ctrl Pts',(6.9999999934628,-20.4049366467525,-10.8540842340856));
#52842=CARTESIAN_POINT('Ctrl Pts',(6.99999998925875,-20.1639637186277,-10.8047802508425));
#52843=CARTESIAN_POINT('Ctrl Pts',(6.99999999152164,-19.9248987558909,-10.7474287548476));
#52844=CARTESIAN_POINT('Ctrl Pts',(6.99999999354319,-19.7113312431013,-10.6961940769836));
#52845=CARTESIAN_POINT('Ctrl Pts',(7.00000000000006,-19.4992861507214,-10.6385361910376));
#52846=CARTESIAN_POINT('Ctrl Pts',(7.00000000000006,-19.2890339655977,-10.5744977405065));
#52847=CARTESIAN_POINT('Ctrl Pts',(7.00000000000006,-19.17655249537,-10.5402382199093));
#52848=CARTESIAN_POINT('Ctrl Pts',(6.99999999803034,-19.0645775028502,-10.504167106816));
#52849=CARTESIAN_POINT('Ctrl Pts',(6.99999999636317,-18.9531879180019,-10.4662992290709));
#52850=CARTESIAN_POINT('Ctrl Pts',(6.99999999271532,-18.7094607695301,-10.3834420223219));
#52851=CARTESIAN_POINT('Ctrl Pts',(6.99999999204987,-18.4685373676012,-10.2919792986757));
#52852=CARTESIAN_POINT('Ctrl Pts',(6.99999999506641,-18.2311614386956,-10.1922299012747));
#52853=CARTESIAN_POINT('Ctrl Pts',(6.99999999705723,-18.0745004696608,-10.1263983010382));
#52854=CARTESIAN_POINT('Ctrl Pts',(7.00000000000006,-17.9193843979218,-10.0569584114509));
#52855=CARTESIAN_POINT('Ctrl Pts',(7.00000000000006,-17.766022595808,-9.98401350658058));
#52856=CARTESIAN_POINT('Ctrl Pts',(7.00000000000006,-17.6246293972524,-9.91676134029285));
#52857=CARTESIAN_POINT('Ctrl Pts',(6.99999999722481,-17.4847350708803,-9.84651938455048));
#52858=CARTESIAN_POINT('Ctrl Pts',(6.9999999944647,-17.3464252545365,-9.77332652209554));
#52859=CARTESIAN_POINT('Ctrl Pts',(6.99999999008274,-17.1268437480598,-9.65712508805378));
#52860=CARTESIAN_POINT('Ctrl Pts',(6.99999998784249,-16.9112542265341,-9.53348786405889));
#52861=CARTESIAN_POINT('Ctrl Pts',(6.99999999262698,-16.7000150345023,-9.4025775854068));
#52862=CARTESIAN_POINT('Ctrl Pts',(6.99999999531406,-16.5813783940284,-9.32905545386764));
#52863=CARTESIAN_POINT('Ctrl Pts',(7.00000000000006,-16.4641144961371,-9.25323851298255));
#52864=CARTESIAN_POINT('Ctrl Pts',(7.00000000000006,-16.3482917008713,-9.17515026984984));
#52865=CARTESIAN_POINT('Ctrl Pts',(7.00000000000006,-16.1866110203611,-9.06614443675301));
#52866=CARTESIAN_POINT('Ctrl Pts',(6.99999999014838,-16.0276937644611,-8.95275813318587));
#52867=CARTESIAN_POINT('Ctrl Pts',(6.99999998525279,-15.8719395759788,-8.83523425985909));
#52868=CARTESIAN_POINT('Ctrl Pts',(6.99999998003402,-15.705902863785,-8.70995173794678));
#52869=CARTESIAN_POINT('Ctrl Pts',(6.99999998145005,-15.5434613041719,-8.57996719362684));
#52870=CARTESIAN_POINT('Ctrl Pts',(6.99999998835937,-15.3850002943582,-8.4456794914934));
#52871=CARTESIAN_POINT('Ctrl Pts',(6.99999999308637,-15.2765894902534,-8.35380681071988));
#52872=CARTESIAN_POINT('Ctrl Pts',(7.00000000000006,-15.170041121258,-8.25992084727754));
#52873=CARTESIAN_POINT('Ctrl Pts',(7.00000000000006,-15.0654684222749,-8.16415901392044));
#52874=CARTESIAN_POINT('Ctrl Pts',(7.00000000000006,-14.942478127508,-8.05153137566937));
#52875=CARTESIAN_POINT('Ctrl Pts',(6.99999999283358,-14.8222826731093,-7.93626853663342));
#52876=CARTESIAN_POINT('Ctrl Pts',(6.99999999157264,-14.704766055738,-7.81832398014723));
#52877=CARTESIAN_POINT('Ctrl Pts',(6.99999999107903,-14.6587635315272,-7.77215393682353));
#52878=CARTESIAN_POINT('Ctrl Pts',(6.99999999110877,-14.6131718473932,-7.72557250510986));
#52879=CARTESIAN_POINT('Ctrl Pts',(6.99999999149981,-14.567985422531,-7.67857521349894));
#52880=CARTESIAN_POINT('Ctrl Pts',(6.99999999249449,-14.4530460284897,-7.55902957040342));
#52881=CARTESIAN_POINT('Ctrl Pts',(6.99999999551018,-14.3407261040585,-7.43679567026283));
#52882=CARTESIAN_POINT('Ctrl Pts',(6.9999999971704,-14.2309835397531,-7.31180056414431));
#52883=CARTESIAN_POINT('Ctrl Pts',(6.99999999862377,-14.1349138626647,-7.20237866792347));
#52884=CARTESIAN_POINT('Ctrl Pts',(6.99999999923222,-14.0408196901903,-7.09084007133104));
#52885=CARTESIAN_POINT('Ctrl Pts',(6.99999999922778,-13.948698167165,-6.97711506158508));
#52886=CARTESIAN_POINT('',(6.27159471697238,-24.269013917935,-11.8794981306075));
#52887=CARTESIAN_POINT('Origin',(5.999999877384,-24.1259420367214,-10.9277801432445));
#52888=CARTESIAN_POINT('Ctrl Pts',(6.27159470456973,-24.2690136413581,-11.8794980693512));
#52889=CARTESIAN_POINT('Ctrl Pts',(6.27193966908722,-24.0395180543602,-11.9138782815514));
#52890=CARTESIAN_POINT('Ctrl Pts',(6.27225782582989,-23.8113318046113,-11.9412742082228));
#52891=CARTESIAN_POINT('Ctrl Pts',(6.27254917050926,-23.5849162071069,-11.962037041859));
#52892=CARTESIAN_POINT('Ctrl Pts',(6.27284515847502,-23.3548921261236,-11.983130781771));
#52893=CARTESIAN_POINT('Ctrl Pts',(6.27311347294071,-23.1266955387491,-11.9973783462536));
#52894=CARTESIAN_POINT('Ctrl Pts',(6.27335411034387,-22.9007559497552,-12.005146606458));
#52895=CARTESIAN_POINT('Ctrl Pts',(6.27354178947188,-22.7245400145422,-12.0112052668415));
#52896=CARTESIAN_POINT('Ctrl Pts',(6.27371263313229,-22.5496958596412,-12.0133226529662));
#52897=CARTESIAN_POINT('Ctrl Pts',(6.27386663999438,-22.3764053057352,-12.0116720606327));
#52898=CARTESIAN_POINT('Ctrl Pts',(6.27406869011557,-22.1490558425905,-12.0095065572487));
#52899=CARTESIAN_POINT('Ctrl Pts',(6.27424176026293,-21.9243820277569,-12.0008567702672));
#52900=CARTESIAN_POINT('Ctrl Pts',(6.27438584818351,-21.7027300644865,-11.9862080166945));
#52901=CARTESIAN_POINT('Ctrl Pts',(6.27447252049793,-21.5694011318745,-11.9773964426885));
#52902=CARTESIAN_POINT('Ctrl Pts',(6.27454870616355,-21.4371646133612,-11.9664139402272));
#52903=CARTESIAN_POINT('Ctrl Pts',(6.27461440482897,-21.3060872704049,-11.9533633073105));
#52904=CARTESIAN_POINT('Ctrl Pts',(6.27472591390497,-21.0836122276783,-11.9312127201056));
#52905=CARTESIAN_POINT('Ctrl Pts',(6.27480721239585,-20.8644791517284,-11.9031052711444));
#52906=CARTESIAN_POINT('Ctrl Pts',(6.27485829924009,-20.6489740686427,-11.8695298232301));
#52907=CARTESIAN_POINT('Ctrl Pts',(6.27487121344989,-20.594496680279,-11.8610423078113));
#52908=CARTESIAN_POINT('Ctrl Pts',(6.27488219706538,-20.5402508831747,-11.8522052883625));
#52909=CARTESIAN_POINT('Ctrl Pts',(6.27489125007749,-20.4862408043715,-11.8430264891903));
#52910=CARTESIAN_POINT('Ctrl Pts',(6.27492812753947,-20.2662306459103,-11.8056366333501));
#52911=CARTESIAN_POINT('Ctrl Pts',(6.27493296962422,-20.0501355961709,-11.76257741312));
#52912=CARTESIAN_POINT('Ctrl Pts',(6.27490577626535,-19.8381798151852,-11.7143926828644));
#52913=CARTESIAN_POINT('Ctrl Pts',(6.27488257692671,-19.6573550055141,-11.6732850771318));
#52914=CARTESIAN_POINT('Ctrl Pts',(6.27483606148424,-19.4795419596773,-11.6284465854906));
#52915=CARTESIAN_POINT('Ctrl Pts',(6.27476623040389,-19.3048532627893,-11.5802011728913));
#52916=CARTESIAN_POINT('Ctrl Pts',(6.27472435242991,-19.2000917631089,-11.5512682089009));
#52917=CARTESIAN_POINT('Ctrl Pts',(6.2746740891859,-19.0964534576399,-11.5211097231509));
#52918=CARTESIAN_POINT('Ctrl Pts',(6.27461544218523,-18.9939586105461,-11.4897934549333));
#52919=CARTESIAN_POINT('Ctrl Pts',(6.27458611868489,-18.9427111869992,-11.4741353208245));
#52920=CARTESIAN_POINT('Ctrl Pts',(6.27455469661342,-18.8917496307821,-11.4581877322973));
#52921=CARTESIAN_POINT('Ctrl Pts',(6.27452117941578,-18.8410761475086,-11.4419589915794));
#52922=CARTESIAN_POINT('Ctrl Pts',(6.27450442081696,-18.8157394058718,-11.4338446212205));
#52923=CARTESIAN_POINT('Ctrl Pts',(6.27448713825884,-18.7904746826481,-11.4256599622173));
#52924=CARTESIAN_POINT('Ctrl Pts',(6.27446933174197,-18.7652822447661,-11.417406045708));
#52925=CARTESIAN_POINT('Ctrl Pts',(6.27445391981117,-18.7434776373593,-11.4102620999773));
#52926=CARTESIAN_POINT('Ctrl Pts',(6.27443873004181,-18.7225443122958,-11.4033384872226));
#52927=CARTESIAN_POINT('Ctrl Pts',(6.27442216619727,-18.7003606182323,-11.3959293058135));
#52928=CARTESIAN_POINT('Ctrl Pts',(6.27441959263581,-18.6969138882179,-11.3947781247761));
#52929=CARTESIAN_POINT('Ctrl Pts',(6.27441698590347,-18.6934370056222,-11.3936151253547));
#52930=CARTESIAN_POINT('Ctrl Pts',(6.27441434001319,-18.6899220490416,-11.3924375508251));
#52931=CARTESIAN_POINT('Ctrl Pts',(6.27440279689551,-18.6745874912887,-11.3873001944403));
#52932=CARTESIAN_POINT('Ctrl Pts',(6.2743910639149,-18.659253820605,-11.3821284442931));
#52933=CARTESIAN_POINT('Ctrl Pts',(6.27437914107232,-18.6439212023062,-11.376922213299));
#52934=CARTESIAN_POINT('Ctrl Pts',(6.2742001082632,-18.4136873710926,-11.2987457085033));
#52935=CARTESIAN_POINT('Ctrl Pts',(6.27397826546618,-18.1836867138033,-11.2127933414718));
#52936=CARTESIAN_POINT('Ctrl Pts',(6.27371361695892,-17.9544888171664,-11.1188672514994));
#52937=CARTESIAN_POINT('Ctrl Pts',(6.27345239043039,-17.7282545130149,-11.0261556519674));
#52938=CARTESIAN_POINT('Ctrl Pts',(6.27314945800378,-17.5028023070296,-10.9256751677364));
#52939=CARTESIAN_POINT('Ctrl Pts',(6.27280482563134,-17.2787286637382,-10.8172494411368));
#52940=CARTESIAN_POINT('Ctrl Pts',(6.27260798186139,-17.1507444573198,-10.7553198881097));
#52941=CARTESIAN_POINT('Ctrl Pts',(6.27239753412351,-17.0232108844582,-10.6907985735669));
#52942=CARTESIAN_POINT('Ctrl Pts',(6.27217348382512,-16.8962464406854,-10.6236547826323));
#52943=CARTESIAN_POINT('Ctrl Pts',(6.2717701365263,-16.6676782762649,-10.5027789485001));
#52944=CARTESIAN_POINT('Ctrl Pts',(6.27132270436512,-16.4409512945987,-10.3734023863807));
#52945=CARTESIAN_POINT('Ctrl Pts',(6.27083119754382,-16.2167888769591,-10.2354143091808));
#52946=CARTESIAN_POINT('Ctrl Pts',(6.2703673283612,-16.0052312078906,-10.1051853605504));
#52947=CARTESIAN_POINT('Ctrl Pts',(6.26986420337956,-15.7959581779868,-9.96728626862293));
#52948=CARTESIAN_POINT('Ctrl Pts',(6.2693218323302,-15.5896259522535,-9.82164365060285));
#52949=CARTESIAN_POINT('Ctrl Pts',(6.26905885839949,-15.4895837459165,-9.75102739668692));
#52950=CARTESIAN_POINT('Ctrl Pts',(6.26878665818488,-15.3902336026562,-9.67859101895923));
#52951=CARTESIAN_POINT('Ctrl Pts',(6.26850523301692,-15.2916544059507,-9.60432785433404));
#52952=CARTESIAN_POINT('Ctrl Pts',(6.26791731255527,-15.0857143073545,-9.44918595872037));
#52953=CARTESIAN_POINT('Ctrl Pts',(6.26728913172618,-14.8831364031573,-9.28606925080027));
#52954=CARTESIAN_POINT('Ctrl Pts',(6.26662070494602,-14.684553681111,-9.11503058970898));
#52955=CARTESIAN_POINT('Ctrl Pts',(6.26595959126037,-14.4881436042373,-8.94586322093109));
#52956=CARTESIAN_POINT('Ctrl Pts',(6.26525910742267,-14.2956417419887,-8.76894625204622));
#52957=CARTESIAN_POINT('Ctrl Pts',(6.26451927074089,-14.1077007982857,-8.58436221949173));
#52958=CARTESIAN_POINT('Ctrl Pts',(6.26430325540102,-14.0528263539262,-8.53046791618305));
#52959=CARTESIAN_POINT('Ctrl Pts',(6.26408388523087,-13.9983409961619,-8.4759201993414));
#52960=CARTESIAN_POINT('Ctrl Pts',(6.26386116072122,-13.9442616342258,-8.4207216444605));
#52961=CARTESIAN_POINT('Ctrl Pts',(6.99999999998952,-24.7867299440625,-9.33248386897489));
#52962=CARTESIAN_POINT('Ctrl Pts',(6.99999999998952,-24.7867268022291,-9.33249195735394));
#52963=CARTESIAN_POINT('Ctrl Pts',(6.99999999998952,-24.6819075264287,-9.6023398658611));
#52964=CARTESIAN_POINT('Ctrl Pts',(6.99999999998952,-24.467486837193,-10.1365881548782));
#52965=CARTESIAN_POINT('Ctrl Pts',(6.99999999998952,-24.2412740854125,-10.6659288230027));
#52966=CARTESIAN_POINT('Ctrl Pts',(6.99999999998952,-24.1259369152881,-10.9277807259463));
#52967=CARTESIAN_POINT('Ctrl Pts',(7.00000270572501,-25.3377021368351,-9.5465023705352));
#52968=CARTESIAN_POINT('Ctrl Pts',(7.00000270572501,-25.3376989472236,-9.54651058191452));
#52969=CARTESIAN_POINT('Ctrl Pts',(7.00000270572501,-25.2312856813305,-9.82046207694803));
#52970=CARTESIAN_POINT('Ctrl Pts',(7.00000270572501,-25.0136075533826,-10.362826432265));
#52971=CARTESIAN_POINT('Ctrl Pts',(7.00000270572501,-24.7839582727123,-10.9002087469914));
#52972=CARTESIAN_POINT('Ctrl Pts',(7.00000270572501,-24.6668671666083,-11.1660426394912));
#52973=CARTESIAN_POINT('Ctrl Pts',(6.57967197783315,-25.7251433388993,-9.69699923153138));
#52974=CARTESIAN_POINT('Ctrl Pts',(6.57967197783315,-25.7251401156906,-9.69700752940395));
#52975=CARTESIAN_POINT('Ctrl Pts',(6.57967197783315,-25.6176059630351,-9.97384464828113));
#52976=CARTESIAN_POINT('Ctrl Pts',(6.57967197783315,-25.397637218632,-10.5219161854199));
#52977=CARTESIAN_POINT('Ctrl Pts',(6.57967197783315,-25.1655713860881,-11.0649533503668));
#52978=CARTESIAN_POINT('Ctrl Pts',(6.57967197783315,-25.0472469199922,-11.3335873602638));
#52979=CARTESIAN_POINT('Ctrl Pts',(5.98852435812724,-25.7188194279219,-9.69454278460152));
#52980=CARTESIAN_POINT('Ctrl Pts',(5.98852435812724,-25.7188162052615,-9.69455108106231));
#52981=CARTESIAN_POINT('Ctrl Pts',(5.98852435812724,-25.6113003479907,-9.97134110007211));
#52982=CARTESIAN_POINT('Ctrl Pts',(5.98852435812724,-25.3913689915969,-10.5193194831806));
#52983=CARTESIAN_POINT('Ctrl Pts',(5.98852435812724,-25.1593426026096,-11.0622643482657));
#52984=CARTESIAN_POINT('Ctrl Pts',(5.98852435812724,-25.0410382677198,-11.330852653955));
#52985=CARTESIAN_POINT('',(6.99999999994035,-24.7867180660544,-9.33250873275177));
#52986=CARTESIAN_POINT('',(5.98852583803482,-25.7188097331028,-9.69456766152955));
#52987=CARTESIAN_POINT('Origin',(5.999999999061,-24.7867247845918,-9.33250979146072));
#52988=CARTESIAN_POINT('',(5.98852581355281,-25.041038964337,-11.3308503205395));
#52989=CARTESIAN_POINT('Origin',(5.98846855882151,11.4751154998608,4.75314843379863));
#52990=CARTESIAN_POINT('Origin',(6.,-24.1259421517584,-10.9277801936246));
#52991=CARTESIAN_POINT('Origin',(6.99999997874242,11.4664777701405,4.74946019467707));
#52992=CARTESIAN_POINT('Origin',(5.999999877384,-24.1259420367214,-10.9277801432445));
#52993=CARTESIAN_POINT('Origin',(5.99999764418935,-24.1259401205898,-10.92777920691));
#52994=CARTESIAN_POINT('Ctrl Pts',(-6.09469640286227,-25.067939639332,-11.2720340325188));
#52995=CARTESIAN_POINT('Ctrl Pts',(-6.05660168672299,-25.0620362475116,
-11.2843010058053));
#52996=CARTESIAN_POINT('Ctrl Pts',(-5.71257762289918,-25.0092998243332,
-11.394110688857));
#52997=CARTESIAN_POINT('Ctrl Pts',(-5.02644182487932,-24.9143124203008,
-11.5957010011836));
#52998=CARTESIAN_POINT('Ctrl Pts',(-3.98600488126534,-24.7973050957913,
-11.8498309399477));
#52999=CARTESIAN_POINT('Ctrl Pts',(-2.81238881479937,-24.6981603854715,
-12.0695365650579));
#53000=CARTESIAN_POINT('Ctrl Pts',(-1.52056314267948,-24.6290900858772,
-12.2259244827651));
#53001=CARTESIAN_POINT('Ctrl Pts',(-0.189421525832001,-24.6021758282813,
-12.2891015458096));
#53002=CARTESIAN_POINT('Ctrl Pts',(1.08612112074885,-24.6169125737592,-12.2542343899029));
#53003=CARTESIAN_POINT('Ctrl Pts',(2.24134091410634,-24.6645165608675,-12.14542388015));
#53004=CARTESIAN_POINT('Ctrl Pts',(3.27311180230409,-24.7349519813417,-11.987723359583));
#53005=CARTESIAN_POINT('Ctrl Pts',(4.20014655760399,-24.8207557066891,-11.7987497778676));
#53006=CARTESIAN_POINT('Ctrl Pts',(5.05723014150755,-24.9193545614888,-11.5851573172023));
#53007=CARTESIAN_POINT('Ctrl Pts',(5.68071122101956,-25.0048784218136,-11.4035074456581));
#53008=CARTESIAN_POINT('Ctrl Pts',(6.0226216716602,-25.0567655494879,-11.2952493912532));
#53009=CARTESIAN_POINT('Ctrl Pts',(6.09456166898787,-25.0679141839452,-11.2720852989104));
#53010=CARTESIAN_POINT('Ctrl Pts',(-6.21867431468926,-24.9346968833895,
-11.6029424921361));
#53011=CARTESIAN_POINT('Ctrl Pts',(-6.17985088684529,-24.9285688314149,
-11.6153919480189));
#53012=CARTESIAN_POINT('Ctrl Pts',(-5.82924224889114,-24.8737915981942,
-11.726821457879));
#53013=CARTESIAN_POINT('Ctrl Pts',(-5.12989137209224,-24.7745387685011,
-11.9311466147024));
#53014=CARTESIAN_POINT('Ctrl Pts',(-4.06887094871852,-24.6510530267549,
-12.1882783777638));
#53015=CARTESIAN_POINT('Ctrl Pts',(-2.87132776031619,-24.5453674748488,
-12.410182967047));
#53016=CARTESIAN_POINT('Ctrl Pts',(-1.5524869166459,-24.4708982597995,-12.5677689267365));
#53017=CARTESIAN_POINT('Ctrl Pts',(-0.193358844396399,-24.4413460965294,
-12.6311563952282));
#53018=CARTESIAN_POINT('Ctrl Pts',(1.10887434912825,-24.4575903644852,-12.5962055595565));
#53019=CARTESIAN_POINT('Ctrl Pts',(2.28838573686662,-24.5091665685093,-12.4866859321996));
#53020=CARTESIAN_POINT('Ctrl Pts',(3.34148469913762,-24.5846570400626,-12.3275787096358));
#53021=CARTESIAN_POINT('Ctrl Pts',(4.2872641910569,-24.6758354477742,-12.1366054642574));
#53022=CARTESIAN_POINT('Ctrl Pts',(5.16125575332339,-24.7797709394588,-11.9204468212989));
#53023=CARTESIAN_POINT('Ctrl Pts',(5.7967639608332,-24.8691764112112,-11.7363471153343));
#53024=CARTESIAN_POINT('Ctrl Pts',(6.14522058488246,-24.9230952791029,-11.6265024693038));
#53025=CARTESIAN_POINT('Ctrl Pts',(6.21853693433094,-24.9346678113508,-11.6029935132844));
#53026=CARTESIAN_POINT('Ctrl Pts',(-6.3291976151697,-24.6411127990943,-11.8134744744563));
#53027=CARTESIAN_POINT('Ctrl Pts',(-6.28967065041395,-24.6348054639139,
-11.8260431665115));
#53028=CARTESIAN_POINT('Ctrl Pts',(-5.93271715869416,-24.5784070111057,
-11.9385075897552));
#53029=CARTESIAN_POINT('Ctrl Pts',(-5.22084676033754,-24.4758901456533,
-12.1441734830564));
#53030=CARTESIAN_POINT('Ctrl Pts',(-4.14083391228667,-24.3476616660051,
-12.4019308785022));
#53031=CARTESIAN_POINT('Ctrl Pts',(-2.92182478818763,-24.2373538322188,
-12.6234624893178));
#53032=CARTESIAN_POINT('Ctrl Pts',(-1.57942699565776,-24.1591923694902,
-12.7800117355765));
#53033=CARTESIAN_POINT('Ctrl Pts',(-0.196627641794983,-24.127897596587,
-12.8424645128103));
#53034=CARTESIAN_POINT('Ctrl Pts',(1.12798366959883,-24.1451325507698,-12.8080890569226));
#53035=CARTESIAN_POINT('Ctrl Pts',(2.32846860310748,-24.1993949614146,-12.6995305381204));
#53036=CARTESIAN_POINT('Ctrl Pts',(3.40040463563438,-24.2783987537493,-12.5410590148184));
#53037=CARTESIAN_POINT('Ctrl Pts',(4.36313923304952,-24.3734142612292,-12.3501602884885));
#53038=CARTESIAN_POINT('Ctrl Pts',(5.25277086485876,-24.4812739291955,-12.1333723566152));
#53039=CARTESIAN_POINT('Ctrl Pts',(5.89966040938067,-24.5736432781445,-11.9480989079523));
#53040=CARTESIAN_POINT('Ctrl Pts',(6.25441184400203,-24.6291702577748,-11.8372584494335));
#53041=CARTESIAN_POINT('Ctrl Pts',(6.32905697483992,-24.6410811304521,-11.8135238830363));
#53042=CARTESIAN_POINT('Ctrl Pts',(-6.39488356493844,-24.2701531239778,
-11.8436584886566));
#53043=CARTESIAN_POINT('Ctrl Pts',(-6.35487788284077,-24.2637628370598,
-11.8562492151803));
#53044=CARTESIAN_POINT('Ctrl Pts',(-5.99361978154214,-24.2066235446642,
-11.9688688499429));
#53045=CARTESIAN_POINT('Ctrl Pts',(-5.27347862166588,-24.1027720674649,
-12.1740981846543));
#53046=CARTESIAN_POINT('Ctrl Pts',(-4.18145578449957,-23.9728855570156,
-12.4299227229637));
#53047=CARTESIAN_POINT('Ctrl Pts',(-2.9495367877123,-23.8611892252005,-12.6486100257343));
#53048=CARTESIAN_POINT('Ctrl Pts',(-1.59373038381807,-23.7820931269272,
-12.8021774001287));
#53049=CARTESIAN_POINT('Ctrl Pts',(-0.198299206200222,-23.7504472304135,
-12.8628132462037));
#53050=CARTESIAN_POINT('Ctrl Pts',(1.13802038684705,-23.7678739310925,-12.8295103268418));
#53051=CARTESIAN_POINT('Ctrl Pts',(2.35020389927267,-23.8227718588654,-12.7233138532897));
#53052=CARTESIAN_POINT('Ctrl Pts',(3.43313687196658,-23.9027473925422,-12.5673442125066));
#53053=CARTESIAN_POINT('Ctrl Pts',(4.40622315044349,-23.9989707201674,-12.3785772414031));
#53054=CARTESIAN_POINT('Ctrl Pts',(5.30578728126644,-24.1082259561267,-12.1632793605793));
#53055=CARTESIAN_POINT('Ctrl Pts',(5.96018217331522,-24.2017987382936,-11.9784438330912));
#53056=CARTESIAN_POINT('Ctrl Pts',(6.31919070559268,-24.2580531221787,-11.8674820485747));
#53057=CARTESIAN_POINT('Ctrl Pts',(6.39473997476331,-24.2701206174988,-11.8437053720656));
#53058=CARTESIAN_POINT('',(-5.98852245733355,-25.0410395152723,-11.3308498383555));
#53059=CARTESIAN_POINT('Ctrl Pts',(-5.98852261948751,-25.0410393033441,
-11.3308502493374));
#53060=CARTESIAN_POINT('Ctrl Pts',(-5.87205076796215,-25.0233544613059,
-11.367685096755));
#53061=CARTESIAN_POINT('Ctrl Pts',(-5.74888355754614,-25.005242019761,-11.4056286998378));
#53062=CARTESIAN_POINT('Ctrl Pts',(-5.61901871664054,-24.9868831667565,
-11.444317480895));
#53063=CARTESIAN_POINT('Ctrl Pts',(-5.51146429395196,-24.9716783136003,
-11.4763596370485));
#53064=CARTESIAN_POINT('Ctrl Pts',(-5.39931579719988,-24.9563046811778,
-11.5089121550632));
#53065=CARTESIAN_POINT('Ctrl Pts',(-5.28257497430164,-24.9408702526267,
-11.5417420021001));
#53066=CARTESIAN_POINT('Ctrl Pts',(-5.21037293125216,-24.9313243436034,
-11.5620466562067));
#53067=CARTESIAN_POINT('Ctrl Pts',(-5.13641382817025,-24.921756434098,-11.5824542767675));
#53068=CARTESIAN_POINT('Ctrl Pts',(-5.0606977888326,-24.9121959426248,-11.6028979719004));
#53069=CARTESIAN_POINT('Ctrl Pts',(-5.00129388439626,-24.9046951471949,
-11.6189373120801));
#53070=CARTESIAN_POINT('Ctrl Pts',(-4.940808549391,-24.8971989135736,-11.6349987771992));
#53071=CARTESIAN_POINT('Ctrl Pts',(-4.87924165182869,-24.8897228456719,
-11.6510488119178));
#53072=CARTESIAN_POINT('Ctrl Pts',(-4.80922171108662,-24.8812203248014,
-11.6693024924573));
#53073=CARTESIAN_POINT('Ctrl Pts',(-4.73780290838212,-24.8727440062738,
-11.6875411426127));
#53074=CARTESIAN_POINT('Ctrl Pts',(-4.66498524290714,-24.8643182000375,
-11.7057116411845));
#53075=CARTESIAN_POINT('Ctrl Pts',(-4.62857641016964,-24.8601052969194,
-11.7147968904705));
#53076=CARTESIAN_POINT('Ctrl Pts',(-4.59181786178269,-24.8559050168986,
-11.723865099662));
#53077=CARTESIAN_POINT('Ctrl Pts',(-4.55470959781019,-24.8517205219723,
-11.7329092764268));
#53078=CARTESIAN_POINT('Ctrl Pts',(-4.53615546582394,-24.8496282745091,
-11.7374313648091));
#53079=CARTESIAN_POINT('Ctrl Pts',(-4.51751390494272,-24.8475399729966,
-11.7419474449398));
#53080=CARTESIAN_POINT('Ctrl Pts',(-4.49878491518002,-24.8454560142994,
-11.7464566339608));
#53081=CARTESIAN_POINT('Ctrl Pts',(-4.48942042029867,-24.8444140349508,
-11.7487112284712));
#53082=CARTESIAN_POINT('Ctrl Pts',(-4.480034068197,-24.8433731412847,-11.7509641001946));
#53083=CARTESIAN_POINT('Ctrl Pts',(-4.47062585887677,-24.8423333832995,
-11.7532151375777));
#53084=CARTESIAN_POINT('Ctrl Pts',(-4.46121764955655,-24.8412936253143,
-11.7554661749609));
#53085=CARTESIAN_POINT('Ctrl Pts',(-4.45054315234059,-24.8401184151216,
-11.7580112496464));
#53086=CARTESIAN_POINT('Ctrl Pts',(-4.4423356592623,-24.8392175664482,-11.7599626347848));
#53087=CARTESIAN_POINT('Ctrl Pts',(-4.30838925350436,-24.8245157030693,
-11.7918092684698));
#53088=CARTESIAN_POINT('Ctrl Pts',(-4.17012435782523,-24.8100104719952,
-11.8233568462962));
#53089=CARTESIAN_POINT('Ctrl Pts',(-4.02753309951211,-24.7958400284994,
-11.8542867658105));
#53090=CARTESIAN_POINT('Ctrl Pts',(-3.89053390305902,-24.7822253132968,
-11.8840036935517));
#53091=CARTESIAN_POINT('Ctrl Pts',(-3.74954081408819,-24.7689196049158,
-11.9131501841802));
#53092=CARTESIAN_POINT('Ctrl Pts',(-3.60456156835002,-24.756055028871,-11.941428033939));
#53093=CARTESIAN_POINT('Ctrl Pts',(-3.4566234260213,-24.7429278983482,-11.9702830092913));
#53094=CARTESIAN_POINT('Ctrl Pts',(-3.30453072099736,-24.730260574804,-11.9982326013014));
#53095=CARTESIAN_POINT('Ctrl Pts',(-3.14828345340735,-24.7181990088325,
-12.024941127055));
#53096=CARTESIAN_POINT('Ctrl Pts',(-3.07015981961235,-24.7121682258468,
-12.0382953899319));
#53097=CARTESIAN_POINT('Ctrl Pts',(-2.99099754506532,-24.7062889446006,
-12.0513391359894));
#53098=CARTESIAN_POINT('Ctrl Pts',(-2.91079662890743,-24.7005796605404,
-12.0640290816424));
#53099=CARTESIAN_POINT('Ctrl Pts',(-2.89466050069938,-24.6994309736676,
-12.0665822518532));
#53100=CARTESIAN_POINT('Ctrl Pts',(-2.87848233128174,-24.6982891659728,
-12.0691211031326));
#53101=CARTESIAN_POINT('Ctrl Pts',(-2.86226211536665,-24.6971543919734,
-12.0716452719487));
#53102=CARTESIAN_POINT('Ctrl Pts',(-2.83817290389319,-24.6954690993121,
-12.0753940035764));
#53103=CARTESIAN_POINT('Ctrl Pts',(-2.81399095318337,-24.6937993201618,
-12.0791103517112));
#53104=CARTESIAN_POINT('Ctrl Pts',(-2.7897162732971,-24.6921455557091,-12.0827931595367));
#53105=CARTESIAN_POINT('Ctrl Pts',(-2.76940638379877,-24.690761901076,-12.0858744533099));
#53106=CARTESIAN_POINT('Ctrl Pts',(-2.74903157918974,-24.6893894585293,
-12.0889322650775));
#53107=CARTESIAN_POINT('Ctrl Pts',(-2.7285918594789,-24.6880285241487,-12.0919659100489));
#53108=CARTESIAN_POINT('Ctrl Pts',(-2.71837199962347,-24.6873480569584,
-12.0934827325346));
#53109=CARTESIAN_POINT('Ctrl Pts',(-2.70813591099257,-24.6866704667983,
-12.0949935133159));
#53110=CARTESIAN_POINT('Ctrl Pts',(-2.69788359358737,-24.6859957907078,
-12.0964981665553));
#53111=CARTESIAN_POINT('Ctrl Pts',(-2.68763127618217,-24.6853211146172,
-12.0980028197947));
#53112=CARTESIAN_POINT('Ctrl Pts',(-2.67595577372556,-24.6845578593136,
-12.0997054936876));
#53113=CARTESIAN_POINT('Ctrl Pts',(-2.66707795505005,-24.6839805416632,
-12.1009936577339));
#53114=CARTESIAN_POINT('Ctrl Pts',(-2.48139215791761,-24.6719055385544,
-12.1279365112102));
#53115=CARTESIAN_POINT('Ctrl Pts',(-2.29080876534563,-24.6607939753664,
-12.1528481905792));
#53116=CARTESIAN_POINT('Ctrl Pts',(-2.09532194002464,-24.6508433076934,
-12.1752575839113));
#53117=CARTESIAN_POINT('Ctrl Pts',(-1.99172347344666,-24.6455699399835,
-12.1871334675281));
#53118=CARTESIAN_POINT('Ctrl Pts',(-1.88674823654334,-24.6406228500151,
-12.1983058558354));
#53119=CARTESIAN_POINT('Ctrl Pts',(-1.78039790893332,-24.6360331099419,
-12.2086994875532));
#53120=CARTESIAN_POINT('Ctrl Pts',(-1.69972470639523,-24.6325515124814,
-12.2165836904091));
#53121=CARTESIAN_POINT('Ctrl Pts',(-1.61826034679528,-24.6292749693734,
-12.2240209290589));
#53122=CARTESIAN_POINT('Ctrl Pts',(-1.53600337413355,-24.6262160050007,
-12.2309799669966));
#53123=CARTESIAN_POINT('Ctrl Pts',(-1.46173164272138,-24.6234539950101,
-12.2372634440061));
#53124=CARTESIAN_POINT('Ctrl Pts',(-1.38681370628058,-24.6208693844213,
-12.2431570369601));
#53125=CARTESIAN_POINT('Ctrl Pts',(-1.31125082907904,-24.6184705634025,
-12.2486374451097));
#53126=CARTESIAN_POINT('Ctrl Pts',(-1.23162592321267,-24.6159427891185,
-12.254412463203));
#53127=CARTESIAN_POINT('Ctrl Pts',(-1.15128415257726,-24.6136213373792,
-12.2597286510634));
#53128=CARTESIAN_POINT('Ctrl Pts',(-1.07022551562338,-24.611515578708,-12.2645590549739));
#53129=CARTESIAN_POINT('Ctrl Pts',(-1.02969619714645,-24.6104626993724,
-12.2669742569292));
#53130=CARTESIAN_POINT('Ctrl Pts',(-0.988987662088587,-24.6094637393483,
-12.2692680108946));
#53131=CARTESIAN_POINT('Ctrl Pts',(-0.948099910353172,-24.6085198307991,
-12.2714369651261));
#53132=CARTESIAN_POINT('Ctrl Pts',(-0.927656034485465,-24.6080478765245,
-12.2725214422418));
#53133=CARTESIAN_POINT('Ctrl Pts',(-0.907167354448814,-24.6075896848596,
-12.2735747192932));
#53134=CARTESIAN_POINT('Ctrl Pts',(-0.886633870240808,-24.6071453945875,
-12.2745963788644));
#53135=CARTESIAN_POINT('Ctrl Pts',(-0.876367128136804,-24.6069232494515,
-12.2751072086499));
#53136=CARTESIAN_POINT('Ctrl Pts',(-0.866089184989999,-24.6067045796472,
-12.2756101340571));
#53137=CARTESIAN_POINT('Ctrl Pts',(-0.855800040800765,-24.6064894023357,
-12.276105103034));
#53138=CARTESIAN_POINT('Ctrl Pts',(-0.845510896611531,-24.6062742250242,
-12.2766000720109));
#53139=CARTESIAN_POINT('Ctrl Pts',(-0.833523570709159,-24.6060284825045,
-12.2771654501541));
#53140=CARTESIAN_POINT('Ctrl Pts',(-0.824899005106446,-24.6058543649454,
-12.2775660886454));
#53141=CARTESIAN_POINT('Ctrl Pts',(-0.603175520772098,-24.6013780871043,
-12.287865849392));
#53142=CARTESIAN_POINT('Ctrl Pts',(-0.379356108691484,-24.5986972392275,
-12.294099179569));
#53143=CARTESIAN_POINT('Ctrl Pts',(-0.153436083501442,-24.5978636227735,
-12.2960197642684));
#53144=CARTESIAN_POINT('Ctrl Pts',(-0.0981464448159366,-24.5976596109667,
-12.296489790925));
#53145=CARTESIAN_POINT('Ctrl Pts',(-0.0427310282098727,-24.5975662928513,
-12.2967012973707));
#53146=CARTESIAN_POINT('Ctrl Pts',(0.0128096103566303,-24.5975847248816,
-12.2966530210514));
#53147=CARTESIAN_POINT('Ctrl Pts',(0.154052749885538,-24.5976315986283,
-12.2965302515068));
#53148=CARTESIAN_POINT('Ctrl Pts',(0.29610840766086,-24.5984033807796,-12.2947229752056));
#53149=CARTESIAN_POINT('Ctrl Pts',(0.438976597831794,-24.5999235338914,
-12.2911986428102));
#53150=CARTESIAN_POINT('Ctrl Pts',(0.510410692917262,-24.6006836104473,
-12.2894364766125));
#53151=CARTESIAN_POINT('Ctrl Pts',(0.582047920626159,-24.6016307834336,
-12.2872450479625));
#53152=CARTESIAN_POINT('Ctrl Pts',(0.653888280922487,-24.6027673887545,
-12.2846215674522));
#53153=CARTESIAN_POINT('Ctrl Pts',(0.689808461070652,-24.603335691415,-12.2833098271971));
#53154=CARTESIAN_POINT('Ctrl Pts',(0.725779424351655,-24.6039513526094,
-12.2818900742089));
#53155=CARTESIAN_POINT('Ctrl Pts',(0.761801170691137,-24.6046146482615,
-12.2803620000399));
#53156=CARTESIAN_POINT('Ctrl Pts',(0.779812043860877,-24.6049462960875,
-12.2795979629554));
#53157=CARTESIAN_POINT('Ctrl Pts',(0.797835612794589,-24.6052898525645,
-12.2788068455948));
#53158=CARTESIAN_POINT('Ctrl Pts',(0.815871877480789,-24.6056453501107,
-12.2779886141642));
#53159=CARTESIAN_POINT('Ctrl Pts',(0.833908142166988,-24.6060008476568,
-12.2771703827336));
#53160=CARTESIAN_POINT('Ctrl Pts',(0.853574764290539,-24.6064022678434,
-12.2762468935398));
#53161=CARTESIAN_POINT('Ctrl Pts',(0.870018758783986,-24.6067476978381,
-12.2754525453828));
#53162=CARTESIAN_POINT('Ctrl Pts',(0.954872427152908,-24.6085301724204,
-12.2713535805536));
#53163=CARTESIAN_POINT('Ctrl Pts',(1.03910591013512,-24.6105606431458,-12.2666936617127));
#53164=CARTESIAN_POINT('Ctrl Pts',(1.12271338003206,-24.6128292922613,-12.2614998270138));
#53165=CARTESIAN_POINT('Ctrl Pts',(1.34022823043383,-24.6187314547544,-12.2479874437431));
#53166=CARTESIAN_POINT('Ctrl Pts',(1.55350464283,-24.6262446722061,-12.2308647797843));
#53167=CARTESIAN_POINT('Ctrl Pts',(1.76254241975356,-24.6351856038298,-12.2106161409963));
#53168=CARTESIAN_POINT('Ctrl Pts',(1.93919399330944,-24.6427413177473,-12.1935046219354));
#53169=CARTESIAN_POINT('Ctrl Pts',(2.11281902534721,-24.6513168882403,-12.1741597888555));
#53170=CARTESIAN_POINT('Ctrl Pts',(2.28342873010899,-24.6608091507357,-12.1528483689007));
#53171=CARTESIAN_POINT('Ctrl Pts',(2.31456109991636,-24.6625412715827,-12.1489595220846));
#53172=CARTESIAN_POINT('Ctrl Pts',(2.34559309142697,-24.6643039339464,-12.1450051321266));
#53173=CARTESIAN_POINT('Ctrl Pts',(2.37652480039739,-24.6660964943325,-12.140986795155));
#53174=CARTESIAN_POINT('Ctrl Pts',(2.47723059042409,-24.6719326157711,-12.1279041103377));
#53175=CARTESIAN_POINT('Ctrl Pts',(2.57774645010243,-24.6781345523141,-12.1140335534561));
#53176=CARTESIAN_POINT('Ctrl Pts',(2.67730193212354,-24.6846447806991,-12.0995100861891));
#53177=CARTESIAN_POINT('Ctrl Pts',(2.77899779962591,-24.6912949752419,-12.084674372747));
#53178=CARTESIAN_POINT('Ctrl Pts',(2.8796914022943,-24.6982668480994,-12.0691574773542));
#53179=CARTESIAN_POINT('Ctrl Pts',(2.97857178221497,-24.7054759893512,-12.0531516948572));
#53180=CARTESIAN_POINT('Ctrl Pts',(3.01268321914448,-24.7079629758224,-12.047630071249));
#53181=CARTESIAN_POINT('Ctrl Pts',(3.04657896440391,-24.7104780025605,-12.0420506729313));
#53182=CARTESIAN_POINT('Ctrl Pts',(3.0802260433282,-24.7130169985012,-12.036422638873));
#53183=CARTESIAN_POINT('Ctrl Pts',(3.15883688464465,-24.7189489430674,-12.0232736670624));
#53184=CARTESIAN_POINT('Ctrl Pts',(3.23630489540883,-24.7250268680016,-12.0098255651543));
#53185=CARTESIAN_POINT('Ctrl Pts',(3.31262859491132,-24.7312313779075,-11.9961225004861));
#53186=CARTESIAN_POINT('Ctrl Pts',(3.45637318405417,-24.7429166700654,-11.9703147708611));
#53187=CARTESIAN_POINT('Ctrl Pts',(3.59605850742905,-24.7550505065092,-11.9436041773303));
#53188=CARTESIAN_POINT('Ctrl Pts',(3.73168881449518,-24.7675089492556,-11.9162751283198));
#53189=CARTESIAN_POINT('Ctrl Pts',(3.8355116079042,-24.7770456844841,-11.8953551859349));
#53190=CARTESIAN_POINT('Ctrl Pts',(3.93695723414212,-24.7867726890048,-11.8740725457157));
#53191=CARTESIAN_POINT('Ctrl Pts',(4.03602569255836,-24.7966365496557,-11.8525471646707));
#53192=CARTESIAN_POINT('Ctrl Pts',(4.06079280716241,-24.7991025148184,-11.8471658194094));
#53193=CARTESIAN_POINT('Ctrl Pts',(4.08642489230921,-24.8016767052159,-11.8415516114812));
#53194=CARTESIAN_POINT('Ctrl Pts',(4.11438437314248,-24.8045167746375,-11.8353623819252));
#53195=CARTESIAN_POINT('Ctrl Pts',(4.14234385397576,-24.807356844059,-11.8291731523692));
#53196=CARTESIAN_POINT('Ctrl Pts',(4.17012474470698,-24.8102092676449,-11.822961572623));
#53197=CARTESIAN_POINT('Ctrl Pts',(4.19772704535576,-24.813072857578,-11.8167302722123));
#53198=CARTESIAN_POINT('Ctrl Pts',(4.20554193314355,-24.8138836100685,-11.81496603835));
#53199=CARTESIAN_POINT('Ctrl Pts',(4.21334250585392,-24.8146952579057,-11.8132002230615));
#53200=CARTESIAN_POINT('Ctrl Pts',(4.2211287629001,-24.8155077747819,-11.8114328844504));
#53201=CARTESIAN_POINT('Ctrl Pts',(4.26834485873559,-24.8204349014448,-11.8007156902017));
#53202=CARTESIAN_POINT('Ctrl Pts',(4.31503452256417,-24.8253939764717,-11.7899425107744));
#53203=CARTESIAN_POINT('Ctrl Pts',(4.36119776853383,-24.8303793321254,-11.7791263095482));
#53204=CARTESIAN_POINT('Ctrl Pts',(4.51915676200642,-24.8474379627442,-11.7421159948919));
#53205=CARTESIAN_POINT('Ctrl Pts',(4.67095309053977,-24.8648025159746,-11.7046073810182));
#53206=CARTESIAN_POINT('Ctrl Pts',(4.81658449887707,-24.8822581001067,-11.6670799571238));
#53207=CARTESIAN_POINT('Ctrl Pts',(4.86926930145242,-24.8885729741736,-11.6535037310774));
#53208=CARTESIAN_POINT('Ctrl Pts',(4.92114738769541,-24.8948998902692,-11.6399245763458));
#53209=CARTESIAN_POINT('Ctrl Pts',(4.97221904055577,-24.901229111514,-11.6263636369502));
#53210=CARTESIAN_POINT('Ctrl Pts',(5.00451866410746,-24.9052319477673,-11.6177871916434));
#53211=CARTESIAN_POINT('Ctrl Pts',(5.0364956863611,-24.9092353290269,-11.6092188631595));
#53212=CARTESIAN_POINT('Ctrl Pts',(5.0681500716503,-24.9132371031204,-11.6006632531542));
#53213=CARTESIAN_POINT('Ctrl Pts',(5.21038871655004,-24.9312190326083,-11.5622187102472));
#53214=CARTESIAN_POINT('Ctrl Pts',(5.34611257555511,-24.9491678527347,-11.5240350807026));
#53215=CARTESIAN_POINT('Ctrl Pts',(5.47532119490194,-24.9669053701192,-11.4865038210347));
#53216=CARTESIAN_POINT('Ctrl Pts',(5.60704624394362,-24.9849883382614,-11.44824161341));
#53217=CARTESIAN_POINT('Ctrl Pts',(5.73199999775446,-25.0028515439196,-11.4106573120967));
#53218=CARTESIAN_POINT('Ctrl Pts',(5.85018400307863,-25.0203164124304,-11.374112915196));
#53219=CARTESIAN_POINT('Ctrl Pts',(5.86232336329831,-25.022110329716,-11.370359229604));
#53220=CARTESIAN_POINT('Ctrl Pts',(5.87439129930192,-25.0239000542431,-11.366616471453));
#53221=CARTESIAN_POINT('Ctrl Pts',(5.88638781265971,-25.0256853994385,-11.3628850030951));
#53222=CARTESIAN_POINT('Ctrl Pts',(5.92102951903959,-25.0308408477093,-11.3521098363977));
#53223=CARTESIAN_POINT('Ctrl Pts',(5.95507566020921,-25.0359597807444,-11.3414288309808));
#53224=CARTESIAN_POINT('Ctrl Pts',(5.98852582161071,-25.041038287801,-11.3308501130812));
#53225=CARTESIAN_POINT('',(-6.27159361731003,-24.2690120888649,-11.8794975616074));
#53226=CARTESIAN_POINT('Origin',(-5.9999949808,-24.1259380084106,-10.9277770011797));
#53227=CARTESIAN_POINT('Ctrl Pts',(-6.27159386307111,-24.2690123724984,
-11.8794985003173));
#53228=CARTESIAN_POINT('Ctrl Pts',(-6.19708065351306,-24.2574475543624,
-11.9025009389632));
#53229=CARTESIAN_POINT('Ctrl Pts',(-6.11543895257566,-24.2450493566266,
-11.9272858537852));
#53230=CARTESIAN_POINT('Ctrl Pts',(-6.02658472781102,-24.2319368753586,
-11.9536191373682));
#53231=CARTESIAN_POINT('Ctrl Pts',(-5.93855997637016,-24.2189468019272,
-11.9797065940779));
#53232=CARTESIAN_POINT('Ctrl Pts',(-5.843456579914,-24.2052557378526,-12.0073137787139));
#53233=CARTESIAN_POINT('Ctrl Pts',(-5.74118385812537,-24.190999674031,-12.036167269489));
#53234=CARTESIAN_POINT('Ctrl Pts',(-5.64049537709834,-24.1769644416982,
-12.0645738094507));
#53235=CARTESIAN_POINT('Ctrl Pts',(-5.53285779290229,-24.1623816149949,
-12.0941884455386));
#53236=CARTESIAN_POINT('Ctrl Pts',(-5.41817822128907,-24.1474001878375,
-12.1247039897279));
#53237=CARTESIAN_POINT('Ctrl Pts',(-5.37925192931951,-24.1423149629849,
-12.1350620418729));
#53238=CARTESIAN_POINT('Ctrl Pts',(-5.33951424232753,-24.1371839758268,
-12.145523488055));
#53239=CARTESIAN_POINT('Ctrl Pts',(-5.29896141200715,-24.1320135572971,
-12.1560750390864));
#53240=CARTESIAN_POINT('Ctrl Pts',(-5.21821295353835,-24.1217182629216,
-12.1770851997462));
#53241=CARTESIAN_POINT('Ctrl Pts',(-5.13423258229018,-24.1112662697748,
-12.1984532839905));
#53242=CARTESIAN_POINT('Ctrl Pts',(-5.0469909527127,-24.1007138190865,-12.2200666252813));
#53243=CARTESIAN_POINT('Ctrl Pts',(-4.92201111320241,-24.0855966829228,
-12.2510292739491));
#53244=CARTESIAN_POINT('Ctrl Pts',(-4.79033819728022,-24.0702723180806,
-12.2824973998057));
#53245=CARTESIAN_POINT('Ctrl Pts',(-4.65188628790323,-24.0549258574929,
-12.3140999820478));
#53246=CARTESIAN_POINT('Ctrl Pts',(-4.51343437852624,-24.0395793969053,
-12.34570256429));
#53247=CARTESIAN_POINT('Ctrl Pts',(-4.36820327813878,-24.0242107182453,
-12.3774398645895));
#53248=CARTESIAN_POINT('Ctrl Pts',(-4.21611007767937,-24.0090298594609,
-12.4088906061113));
#53249=CARTESIAN_POINT('Ctrl Pts',(-4.07082690496949,-23.9945287290882,
-12.4389331293704));
#53250=CARTESIAN_POINT('Ctrl Pts',(-3.919281825186,-23.9801990076705,-12.4687138657733));
#53251=CARTESIAN_POINT('Ctrl Pts',(-3.76141964906482,-23.9662475292409,
-12.4978250150864));
#53252=CARTESIAN_POINT('Ctrl Pts',(-3.73054601994573,-23.9635189923533,
-12.503518379065));
#53253=CARTESIAN_POINT('Ctrl Pts',(-3.69943080463875,-23.960804995437,-12.5091859945926));
#53254=CARTESIAN_POINT('Ctrl Pts',(-3.66807364565266,-23.9581071929869,
-12.5148246080531));
#53255=CARTESIAN_POINT('Ctrl Pts',(-3.58017499593443,-23.9505448627174,
-12.5306304567171));
#53256=CARTESIAN_POINT('Ctrl Pts',(-3.490375146284,-23.9431096165281,-12.546208731638));
#53257=CARTESIAN_POINT('Ctrl Pts',(-3.39866712296084,-23.9358394501584,
-12.5614848710859));
#53258=CARTESIAN_POINT('Ctrl Pts',(-3.35281311129926,-23.9322043669735,
-12.5691229408098));
#53259=CARTESIAN_POINT('Ctrl Pts',(-3.30648204726695,-23.9286105470841,
-12.5766854190333));
#53260=CARTESIAN_POINT('Ctrl Pts',(-3.25967322938304,-23.9250630078039,
-12.5841625636959));
#53261=CARTESIAN_POINT('Ctrl Pts',(-3.23626882044109,-23.9232892381638,
-12.5879011360272));
#53262=CARTESIAN_POINT('Ctrl Pts',(-3.21274497244039,-23.9215270382459,
-12.5916183712853));
#53263=CARTESIAN_POINT('Ctrl Pts',(-3.1891016016632,-23.9197770417985,-12.5953130271372));
#53264=CARTESIAN_POINT('Ctrl Pts',(-3.17727991627461,-23.9189020435748,
-12.5971603550631));
#53265=CARTESIAN_POINT('Ctrl Pts',(-3.1654283501572,-23.9180300961918,-12.5990020379013));
#53266=CARTESIAN_POINT('Ctrl Pts',(-3.15354689347884,-23.9171612798269,
-12.6008379186848));
#53267=CARTESIAN_POINT('Ctrl Pts',(-3.14166543680048,-23.9162924634619,
-12.6026737994683));
#53268=CARTESIAN_POINT('Ctrl Pts',(-3.12814004811533,-23.9153102015369,
-12.6047504356254));
#53269=CARTESIAN_POINT('Ctrl Pts',(-3.11781284205288,-23.9145643041974,
-12.6063279968725));
#53270=CARTESIAN_POINT('Ctrl Pts',(-3.07662019693105,-23.9115891060443,
-12.6126204945932));
#53271=CARTESIAN_POINT('Ctrl Pts',(-3.03568681537497,-23.9086932554489,
-12.6187484873184));
#53272=CARTESIAN_POINT('Ctrl Pts',(-2.99501443262714,-23.9058746076504,
-12.6247163285268));
#53273=CARTESIAN_POINT('Ctrl Pts',(-2.79739858312814,-23.8921795782105,
-12.6537124170365));
#53274=CARTESIAN_POINT('Ctrl Pts',(-2.6059481172625,-23.8803065355462,-12.6789294120371));
#53275=CARTESIAN_POINT('Ctrl Pts',(-2.42085608552228,-23.8700051487675,
-12.700877549924));
#53276=CARTESIAN_POINT('Ctrl Pts',(-2.23092814035405,-23.859434616882,-12.7233991284594));
#53277=CARTESIAN_POINT('Ctrl Pts',(-2.04769490737325,-23.8505187444206,
-12.7424791212769));
#53278=CARTESIAN_POINT('Ctrl Pts',(-1.87131615446196,-23.8429959123325,
-12.7586449499604));
#53279=CARTESIAN_POINT('Ctrl Pts',(-1.78117031097362,-23.8391510498827,
-12.7669071824476));
#53280=CARTESIAN_POINT('Ctrl Pts',(-1.69281421885882,-23.8356702303762,
-12.7744077811853));
#53281=CARTESIAN_POINT('Ctrl Pts',(-1.60626489566071,-23.8325196335033,
-12.7812144424466));
#53282=CARTESIAN_POINT('Ctrl Pts',(-1.43907112315413,-23.826433390915,-12.7943633768622));
#53283=CARTESIAN_POINT('Ctrl Pts',(-1.27862186952989,-23.8215784079356,
-12.804925193892));
#53284=CARTESIAN_POINT('Ctrl Pts',(-1.12501669320035,-23.8177150204011,
-12.8133804302271));
#53285=CARTESIAN_POINT('Ctrl Pts',(-0.969939790398224,-23.8138146168634,
-12.8219166781235));
#53286=CARTESIAN_POINT('Ctrl Pts',(-0.821838349560999,-23.8109247887991,
-12.8283059141215));
#53287=CARTESIAN_POINT('Ctrl Pts',(-0.680782441978169,-23.808815889581,
-12.8330036984709));
#53288=CARTESIAN_POINT('Ctrl Pts',(-0.538388175208224,-23.8066869808172,
-12.8377460560887));
#53289=CARTESIAN_POINT('Ctrl Pts',(-0.403173390274244,-23.8053537794222,
-12.8407648496665));
#53290=CARTESIAN_POINT('Ctrl Pts',(-0.275183236026138,-23.8045989488871,
-12.8424872290624));
#53291=CARTESIAN_POINT('Ctrl Pts',(-0.236228074657881,-23.8043692082052,
-12.8430114535053));
#53292=CARTESIAN_POINT('Ctrl Pts',(-0.197942004448109,-23.8041931828349,
-12.8434152878692));
#53293=CARTESIAN_POINT('Ctrl Pts',(-0.160325891526743,-23.804065111692,
-12.8437099928471));
#53294=CARTESIAN_POINT('Ctrl Pts',(-0.154008551789045,-23.8040436031187,
-12.8437594863041));
#53295=CARTESIAN_POINT('Ctrl Pts',(-0.147710107568991,-23.804023447473,
-12.8438059009661));
#53296=CARTESIAN_POINT('Ctrl Pts',(-0.141430562185521,-23.8040046167472,
-12.843849290145));
#53297=CARTESIAN_POINT('Ctrl Pts',(-0.103047991455955,-23.8038895173851,
-12.8441144985521));
#53298=CARTESIAN_POINT('Ctrl Pts',(-0.0662560608545565,-23.8038251207424,
-12.8442644001821));
#53299=CARTESIAN_POINT('Ctrl Pts',(-0.0289816147159557,-23.8038019492759,
-12.8443170148345));
#53300=CARTESIAN_POINT('Ctrl Pts',(-0.0185593893001033,-23.8037954703535,
-12.844331726301));
#53301=CARTESIAN_POINT('Ctrl Pts',(-0.00809943928968467,-23.8037923580938,
-12.8443385552721));
#53302=CARTESIAN_POINT('Ctrl Pts',(0.0024435548564048,-23.803792739344,
-12.8443372522127));
#53303=CARTESIAN_POINT('Ctrl Pts',(0.127127989417073,-23.8037972481167,
-12.8443218418633));
#53304=CARTESIAN_POINT('Ctrl Pts',(0.25898642404739,-23.8042924746921,-12.8431696762975));
#53305=CARTESIAN_POINT('Ctrl Pts',(0.397985640324334,-23.8054910550641,
-12.8404650160666));
#53306=CARTESIAN_POINT('Ctrl Pts',(0.535666720384046,-23.8066782692412,
-12.837786004258));
#53307=CARTESIAN_POINT('Ctrl Pts',(0.680354116090917,-23.8085556434041,
-12.8335836901914));
#53308=CARTESIAN_POINT('Ctrl Pts',(0.831993591445606,-23.8113495705492,
-12.8274126495319));
#53309=CARTESIAN_POINT('Ctrl Pts',(0.942261582564669,-23.8133812363334,
-12.8229252411242));
#53310=CARTESIAN_POINT('Ctrl Pts',(1.05620525936726,-23.815897968114,-12.8173959531631));
#53311=CARTESIAN_POINT('Ctrl Pts',(1.17379482851288,-23.818993100867,-12.8106400419382));
#53312=CARTESIAN_POINT('Ctrl Pts',(1.33435500185533,-23.8232192839796,-12.8014153268106));
#53313=CARTESIAN_POINT('Ctrl Pts',(1.50171435296593,-23.8285235621057,-12.7899045033718));
#53314=CARTESIAN_POINT('Ctrl Pts',(1.67576187127814,-23.8351487432857,-12.7756218976607));
#53315=CARTESIAN_POINT('Ctrl Pts',(1.84377414908803,-23.8415441908723,-12.7618345530215));
#53316=CARTESIAN_POINT('Ctrl Pts',(2.01801903026665,-23.8491706974574,-12.7454640321563));
#53317=CARTESIAN_POINT('Ctrl Pts',(2.19835996716835,-23.85825712127,-12.7260475830157));
#53318=CARTESIAN_POINT('Ctrl Pts',(2.26108100521229,-23.8614173018892,-12.7192947077887));
#53319=CARTESIAN_POINT('Ctrl Pts',(2.32453906546292,-23.8647541557383,-12.7121731843065));
#53320=CARTESIAN_POINT('Ctrl Pts',(2.38872722788395,-23.8682775611684,-12.7046628694941));
#53321=CARTESIAN_POINT('Ctrl Pts',(2.47499317115351,-23.8730128562988,-12.6945693512018));
#53322=CARTESIAN_POINT('Ctrl Pts',(2.56257789012541,-23.87808510115,-12.6837736012509));
#53323=CARTESIAN_POINT('Ctrl Pts',(2.65146471615966,-23.8835179367988,-12.6722277411706));
#53324=CARTESIAN_POINT('Ctrl Pts',(2.72897727448682,-23.8882555678843,-12.6621593295416));
#53325=CARTESIAN_POINT('Ctrl Pts',(2.80748002688193,-23.8932674685411,-12.651520474965));
#53326=CARTESIAN_POINT('Ctrl Pts',(2.88696068491028,-23.89856938809,-12.6402790265889));
#53327=CARTESIAN_POINT('Ctrl Pts',(2.92670101392446,-23.9012203478645,-12.6346583024009));
#53328=CARTESIAN_POINT('Ctrl Pts',(2.96668581815838,-23.9039438114799,-12.6288869221067));
#53329=CARTESIAN_POINT('Ctrl Pts',(3.00691344054863,-23.9067417736369,-12.6229608336922));
#53330=CARTESIAN_POINT('Ctrl Pts',(3.02702725174375,-23.9081407547155,-12.619997789485));
#53331=CARTESIAN_POINT('Ctrl Pts',(3.04720176742329,-23.9095583603789,-12.6169960677866));
#53332=CARTESIAN_POINT('Ctrl Pts',(3.06743677586502,-23.9109948393404,-12.6139551599589));
#53333=CARTESIAN_POINT('Ctrl Pts',(3.07755428008588,-23.9117130788211,-12.6124347060451));
#53334=CARTESIAN_POINT('Ctrl Pts',(3.08768690749317,-23.9124360366231,-12.6109044555701));
#53335=CARTESIAN_POINT('Ctrl Pts',(3.09783463114383,-23.9131637438721,-12.6093643448404));
#53336=CARTESIAN_POINT('Ctrl Pts',(3.1079823547945,-23.913891451121,-12.6078242341107));
#53337=CARTESIAN_POINT('Ctrl Pts',(3.11649244074334,-23.9145041917183,-12.6065275662883));
#53338=CARTESIAN_POINT('Ctrl Pts',(3.12832306372687,-23.9153611450882,-12.6047143680975));
#53339=CARTESIAN_POINT('Ctrl Pts',(3.24396685480677,-23.9237378245419,-12.5869904398604));
#53340=CARTESIAN_POINT('Ctrl Pts',(3.35681912039119,-23.9324154957705,-12.5687089038458));
#53341=CARTESIAN_POINT('Ctrl Pts',(3.4668879598054,-23.9413241010436,-12.5500064110851));
#53342=CARTESIAN_POINT('Ctrl Pts',(3.63912660786559,-23.9552645235693,-12.5207402528736));
#53343=CARTESIAN_POINT('Ctrl Pts',(3.80454906756701,-23.9697690124171,-12.4904460839916));
#53344=CARTESIAN_POINT('Ctrl Pts',(3.96321157890833,-23.9845899397826,-12.459612244304));
#53345=CARTESIAN_POINT('Ctrl Pts',(4.12187409024965,-23.9994108671481,-12.4287784046164));
#53346=CARTESIAN_POINT('Ctrl Pts',(4.27377692443362,-24.0145483743825,-12.3974046276365));
#53347=CARTESIAN_POINT('Ctrl Pts',(4.4189885867178,-24.0297823945403,-12.3659264725924));
#53348=CARTESIAN_POINT('Ctrl Pts',(4.56351829145772,-24.0449448711678,-12.3345961484111));
#53349=CARTESIAN_POINT('Ctrl Pts',(4.70142003690318,-24.0602031912136,-12.3031622817141));
#53350=CARTESIAN_POINT('Ctrl Pts',(4.8327746454666,-24.0753671449434,-12.2720086542693));
#53351=CARTESIAN_POINT('Ctrl Pts',(4.90532346446221,-24.0837423892264,-12.254802110066));
#53352=CARTESIAN_POINT('Ctrl Pts',(4.97587515091848,-24.0920892595714,-12.2376801962019));
#53353=CARTESIAN_POINT('Ctrl Pts',(5.04444362554569,-24.1003786527912,-12.2207014861673));
#53354=CARTESIAN_POINT('Ctrl Pts',(5.13538826924481,-24.1113731501452,-12.1981820595218));
#53355=CARTESIAN_POINT('Ctrl Pts',(5.22284414698212,-24.1222663281055,-12.1759149756777));
#53356=CARTESIAN_POINT('Ctrl Pts',(5.30684382899792,-24.1329956869054,-12.1540257892894));
#53357=CARTESIAN_POINT('Ctrl Pts',(5.42689862544594,-24.1483303995594,-12.1227411254289));
#53358=CARTESIAN_POINT('Ctrl Pts',(5.53989391654885,-24.1633297986691,-12.0922303547407));
#53359=CARTESIAN_POINT('Ctrl Pts',(5.64592674944952,-24.1778361923838,-12.0628174732137));
#53360=CARTESIAN_POINT('Ctrl Pts',(5.75378605730955,-24.1925924668584,-12.0328979383218));
#53361=CARTESIAN_POINT('Ctrl Pts',(5.85444112642878,-24.2068385834764,-12.0041143447075));
#53362=CARTESIAN_POINT('Ctrl Pts',(5.94798675722919,-24.2204298947769,-11.9767582307012));
#53363=CARTESIAN_POINT('Ctrl Pts',(6.02496392816279,-24.2316139627471,-11.9542473315183));
#53364=CARTESIAN_POINT('Ctrl Pts',(6.09712692397713,-24.2423550377847,-11.9327020733305));
#53365=CARTESIAN_POINT('Ctrl Pts',(6.16452391351239,-24.2525831812488,-11.9122611829523));
#53366=CARTESIAN_POINT('Ctrl Pts',(6.20165874427759,-24.258218750125,-11.9009985284907));
#53367=CARTESIAN_POINT('Ctrl Pts',(6.23734659769671,-24.2636988047476,-11.8900707716899));
#53368=CARTESIAN_POINT('Ctrl Pts',(6.27159479316353,-24.2690136880217,-11.879498379804));
#53369=CARTESIAN_POINT('Ctrl Pts',(-6.390311350267,-24.5118463360737,-11.8061935774203));
#53370=CARTESIAN_POINT('Ctrl Pts',(-4.260207566844,-24.1870546297901,-12.4817978606254));
#53371=CARTESIAN_POINT('Ctrl Pts',(0.00016633772734,-23.8622593703069,-13.1582627624527));
#53372=CARTESIAN_POINT('Ctrl Pts',(4.260540242299,-24.1870799927345,-12.4817450361405));
#53373=CARTESIAN_POINT('Ctrl Pts',(6.390810363449,-24.5119224270561,-11.8060352994126));
#53374=CARTESIAN_POINT('Ctrl Pts',(-6.390311350267,-23.545895230188,-11.9720501088178));
#53375=CARTESIAN_POINT('Ctrl Pts',(-4.260207566844,-23.2652553174244,-12.6077625233822));
#53376=CARTESIAN_POINT('Ctrl Pts',(0.00016633772734,-22.9846371837595,-13.2461470236444));
#53377=CARTESIAN_POINT('Ctrl Pts',(4.260540242299,-23.2652772306214,-12.6077126725587));
#53378=CARTESIAN_POINT('Ctrl Pts',(6.390810363449,-23.5459609774455,-11.9719011765393));
#53379=CARTESIAN_POINT('Ctrl Pts',(-6.390311350267,-21.4528914442104,-12.0713617472543));
#53380=CARTESIAN_POINT('Ctrl Pts',(-4.260207566844,-21.2792389843666,-12.659242501556));
#53381=CARTESIAN_POINT('Ctrl Pts',(0.0001663377273399,-21.1056335160082,
-13.2456907741115));
#53382=CARTESIAN_POINT('Ctrl Pts',(4.260540242299,-21.2792525410423,-12.65919670638));
#53383=CARTESIAN_POINT('Ctrl Pts',(6.390810363449,-21.4529321268594,-12.0712240207621));
#53384=CARTESIAN_POINT('Ctrl Pts',(-6.390311350267,-18.3168609136217,-11.3879808552382));
#53385=CARTESIAN_POINT('Ctrl Pts',(-4.260207566844,-18.3050659001792,-12.0191856806231));
#53386=CARTESIAN_POINT('Ctrl Pts',(0.0001663377273402,-18.2929947474288,
-12.6510858023083));
#53387=CARTESIAN_POINT('Ctrl Pts',(4.260540242299,-18.3050668428013,-12.0191363361582));
#53388=CARTESIAN_POINT('Ctrl Pts',(6.390810363449,-18.3168636769148,-11.3878329789646));
#53389=CARTESIAN_POINT('Ctrl Pts',(-6.390311350267,-15.6641217900945,-9.96973288195603));
#53390=CARTESIAN_POINT('Ctrl Pts',(-4.260207566844,-15.7526919735633,-10.7489905945888));
#53391=CARTESIAN_POINT('Ctrl Pts',(0.0001663377273394,-15.8421756717823,
-11.5273064696613));
#53392=CARTESIAN_POINT('Ctrl Pts',(4.260540242299,-15.7526849858726,-10.7489298166621));
#53393=CARTESIAN_POINT('Ctrl Pts',(6.390810363449,-15.6641010402186,-9.96955032039603));
#53394=CARTESIAN_POINT('Ctrl Pts',(-6.390311350267,-14.2543287641255,-8.71309675413792));
#53395=CARTESIAN_POINT('Ctrl Pts',(-4.260207566844,-14.3567676644292,-9.62713414228719));
#53396=CARTESIAN_POINT('Ctrl Pts',(0.0001663377273409,-14.4578353619718,
-10.5425565369485));
#53397=CARTESIAN_POINT('Ctrl Pts',(4.260540242299,-14.3567597721566,-9.62706265784722));
#53398=CARTESIAN_POINT('Ctrl Pts',(6.390810363449,-14.2543047651132,-8.71288261692475));
#53399=CARTESIAN_POINT('Ctrl Pts',(-6.390311350267,-13.7249660384067,-8.13937934281661));
#53400=CARTESIAN_POINT('Ctrl Pts',(-4.260207566844,-13.8221738529227,-9.11426644869758));
#53401=CARTESIAN_POINT('Ctrl Pts',(0.0001663377273409,-13.9182987555376,
-10.0902661487876));
#53402=CARTESIAN_POINT('Ctrl Pts',(4.260540242299,-13.8221663466254,-9.11419023383394));
#53403=CARTESIAN_POINT('Ctrl Pts',(6.390810363449,-13.7249432649203,-8.1391509499607));
#53404=CARTESIAN_POINT('',(-6.26385894390912,-13.9442626806115,-8.42070713435433));
#53405=CARTESIAN_POINT('Ctrl Pts',(-6.27159552384312,-24.269012166051,-11.8794980574164));
#53406=CARTESIAN_POINT('Ctrl Pts',(-6.27195777361259,-24.0278185145914,
-11.9156534425328));
#53407=CARTESIAN_POINT('Ctrl Pts',(-6.27229031331253,-23.7878332021302,
-11.9441024507922));
#53408=CARTESIAN_POINT('Ctrl Pts',(-6.27259314318901,-23.5495553100136,
-11.9652318875922));
#53409=CARTESIAN_POINT('Ctrl Pts',(-6.27289863590125,-23.309182198958,-11.9865471192041));
#53410=CARTESIAN_POINT('Ctrl Pts',(-6.27317389400559,-23.0705465785284,
-12.0004135122592));
#53411=CARTESIAN_POINT('Ctrl Pts',(-6.27341891775463,-22.8341072928724,
-12.0072245172161));
#53412=CARTESIAN_POINT('Ctrl Pts',(-6.27366754294784,-22.5941927404691,
-12.0141356326898));
#53413=CARTESIAN_POINT('Ctrl Pts',(-6.27388503846378,-22.3565395172541,
-12.0137824595501));
#53414=CARTESIAN_POINT('Ctrl Pts',(-6.27407140456636,-22.1215730806342,
-12.0065719106687));
#53415=CARTESIAN_POINT('Ctrl Pts',(-6.27421804504213,-21.9366918732854,
-12.0008983557473));
#53416=CARTESIAN_POINT('Ctrl Pts',(-6.274345412718,-21.7534730092084,-11.9909791927894));
#53417=CARTESIAN_POINT('Ctrl Pts',(-6.27445350772255,-21.5721011929363,
-11.9770107164412));
#53418=CARTESIAN_POINT('Ctrl Pts',(-6.27450263019869,-21.4896789500694,
-11.9706629101849));
#53419=CARTESIAN_POINT('Ctrl Pts',(-6.27454777260064,-21.4076378813805,
-11.9634788610596));
#53420=CARTESIAN_POINT('Ctrl Pts',(-6.27458893494047,-21.3259936705028,
-11.9554821150223));
#53421=CARTESIAN_POINT('Ctrl Pts',(-6.27470712676182,-21.0915638974046,
-11.9325205928409));
#53422=CARTESIAN_POINT('Ctrl Pts',(-6.27479250379279,-20.8604098971047,
-11.9028602054795));
#53423=CARTESIAN_POINT('Ctrl Pts',(-6.27484506603337,-20.6328676324398,
-11.867043777871));
#53424=CARTESIAN_POINT('Ctrl Pts',(-6.27489762827396,-20.4053253677749,
-11.8312273502626));
#53425=CARTESIAN_POINT('Ctrl Pts',(-6.27491737572417,-20.1813946486095,
-11.7892548434866));
#53426=CARTESIAN_POINT('Ctrl Pts',(-6.274904308384,-19.9613613260337,-11.7416479058904));
#53427=CARTESIAN_POINT('Ctrl Pts',(-6.27489476877272,-19.8007293735071,
-11.7068931912392));
#53428=CARTESIAN_POINT('Ctrl Pts',(-6.27486754215411,-19.641886015768,-11.6690684550223));
#53429=CARTESIAN_POINT('Ctrl Pts',(-6.27482284572605,-19.4852449189779,
-11.6284287739379));
#53430=CARTESIAN_POINT('Ctrl Pts',(-6.27477793235585,-19.3278435365188,
-11.5875918408694));
#53431=CARTESIAN_POINT('Ctrl Pts',(-6.27471537917892,-19.1726661423447,
-11.5439127568876));
#53432=CARTESIAN_POINT('Ctrl Pts',(-6.27463540657113,-19.0201057129404,
-11.4976958184635));
#53433=CARTESIAN_POINT('Ctrl Pts',(-6.27457693113742,-18.9085545515761,
-11.4639023034869));
#53434=CARTESIAN_POINT('Ctrl Pts',(-6.27450914251616,-18.7984019852882,
-11.4287529048035));
#53435=CARTESIAN_POINT('Ctrl Pts',(-6.27443212685842,-18.6897913755697,
-11.3923809119521));
#53436=CARTESIAN_POINT('Ctrl Pts',(-6.2743563554567,-18.5829354662577,-11.3565965407962));
#53437=CARTESIAN_POINT('Ctrl Pts',(-6.27427024866111,-18.4758579337037,
-11.3190560601371));
#53438=CARTESIAN_POINT('Ctrl Pts',(-6.27417380647165,-18.3686262100889,
-11.2797074657311));
#53439=CARTESIAN_POINT('Ctrl Pts',(-6.27399075729118,-18.1650982806783,
-11.2050230563539));
#53440=CARTESIAN_POINT('Ctrl Pts',(-6.27377047507158,-17.9610120041854,
-11.123823840775));
#53441=CARTESIAN_POINT('Ctrl Pts',(-6.27351295981285,-17.7568367231181,
-11.035841741865));
#53442=CARTESIAN_POINT('Ctrl Pts',(-6.27325823671108,-17.554875250418,-10.9488136051864));
#53443=CARTESIAN_POINT('Ctrl Pts',(-6.2729670836052,-17.3528266037693,-10.8551488043137));
#53444=CARTESIAN_POINT('Ctrl Pts',(-6.27263950049519,-17.1511936567995,
-10.7546017230361));
#53445=CARTESIAN_POINT('Ctrl Pts',(-6.27231700457665,-16.9526919622582,
-10.655616084455));
#53446=CARTESIAN_POINT('Ctrl Pts',(-6.27195920134555,-16.7545931145514,
-10.5499602069169));
#53447=CARTESIAN_POINT('Ctrl Pts',(-6.27156609080189,-16.5574252175733,
-10.4374141472497));
#53448=CARTESIAN_POINT('Ctrl Pts',(-6.2713627573503,-16.4554416160609,-10.379200550225));
#53449=CARTESIAN_POINT('Ctrl Pts',(-6.27114997778991,-16.3537078788031,
-10.319143797673));
#53450=CARTESIAN_POINT('Ctrl Pts',(-6.27092775212072,-16.2523023418362,
-10.2572150776267));
#53451=CARTESIAN_POINT('Ctrl Pts',(-6.27050608517554,-16.0598881929588,
-10.1397070764348));
#53452=CARTESIAN_POINT('Ctrl Pts',(-6.27005040934441,-15.8686527392963,
-10.0154582935042));
#53453=CARTESIAN_POINT('Ctrl Pts',(-6.26956072399719,-15.6791680310297,
-9.88428363945258));
#53454=CARTESIAN_POINT('Ctrl Pts',(-6.2693850560598,-15.6111929771396,-9.83722652196934));
#53455=CARTESIAN_POINT('Ctrl Pts',(-6.26920501137747,-15.543443689627,-9.78927825014016));
#53456=CARTESIAN_POINT('Ctrl Pts',(-6.26902058992111,-15.4759481426865,
-9.74043078842283));
#53457=CARTESIAN_POINT('Ctrl Pts',(-6.26850854403676,-15.2885468624668,
-9.60480588757748));
#53458=CARTESIAN_POINT('Ctrl Pts',(-6.26796275784848,-15.1030987092309,
-9.46224688357658));
#53459=CARTESIAN_POINT('Ctrl Pts',(-6.2673832307336,-14.9201609309892,-9.31269380803585));
#53460=CARTESIAN_POINT('Ctrl Pts',(-6.2668123205751,-14.7399432443758,-9.16536442883974));
#53461=CARTESIAN_POINT('Ctrl Pts',(-6.26620866541429,-14.5621618196626,
-9.01124737044733));
#53462=CARTESIAN_POINT('Ctrl Pts',(-6.26557226465588,-14.387390153543,-8.85031461575968));
#53463=CARTESIAN_POINT('Ctrl Pts',(-6.26502584988123,-14.2373309034618,
-8.71213747859487));
#53464=CARTESIAN_POINT('Ctrl Pts',(-6.26445529515408,-14.0894910489303,
-8.56893625679463));
#53465=CARTESIAN_POINT('Ctrl Pts',(-6.26386060009764,-13.9442583528487,
-8.4207113681085));
#53466=CARTESIAN_POINT('Ctrl Pts',(6.26385988969939,-13.9442649557967,-8.42071839556296));
#53467=CARTESIAN_POINT('Ctrl Pts',(5.97383874386791,-13.9556277753621,-8.54578524258237));
#53468=CARTESIAN_POINT('Ctrl Pts',(5.68187737111666,-13.9653433861138,-8.66214789045299));
#53469=CARTESIAN_POINT('Ctrl Pts',(5.38846823418052,-13.9736716145702,-8.7696610247794));
#53470=CARTESIAN_POINT('Ctrl Pts',(5.11338258670262,-13.9814797426375,-8.87045993130766));
#53471=CARTESIAN_POINT('Ctrl Pts',(4.83702435532471,-13.988068547081,-8.96347945608504));
#53472=CARTESIAN_POINT('Ctrl Pts',(4.55979938137085,-13.9936635247548,-9.0486414964153));
#53473=CARTESIAN_POINT('Ctrl Pts',(4.30239065070984,-13.9988585693446,-9.12771609200192));
#53474=CARTESIAN_POINT('Ctrl Pts',(4.04423465963907,-14.0031969134852,-9.20001611936352));
#53475=CARTESIAN_POINT('Ctrl Pts',(3.78565629268788,-14.0068671085627,-9.26552212090106));
#53476=CARTESIAN_POINT('Ctrl Pts',(3.57067714236566,-14.009918467532,-9.31998307491506));
#53477=CARTESIAN_POINT('Ctrl Pts',(3.35540604275743,-14.0125081378356,-9.36974849325115));
#53478=CARTESIAN_POINT('Ctrl Pts',(3.14002969264849,-14.0147484168714,-9.41483453292874));
#53479=CARTESIAN_POINT('Ctrl Pts',(2.89780153371509,-14.0172680002243,-9.46554162485956));
#53480=CARTESIAN_POINT('Ctrl Pts',(2.65545132443959,-14.019360774289,-9.51033998830773));
#53481=CARTESIAN_POINT('Ctrl Pts',(2.41322275468519,-14.0210847790028,-9.54920642782744));
#53482=CARTESIAN_POINT('Ctrl Pts',(2.17467354086663,-14.0227825967686,-9.5874825015406));
#53483=CARTESIAN_POINT('Ctrl Pts',(1.93624229932215,-14.024122784021,-9.62000545081673));
#53484=CARTESIAN_POINT('Ctrl Pts',(1.69816178307905,-14.0251655159631,-9.64680346661629));
#53485=CARTESIAN_POINT('Ctrl Pts',(1.4617492566177,-14.0262009425354,-9.67341373577774));
#53486=CARTESIAN_POINT('Ctrl Pts',(1.22568255831659,-14.0269430813681,-9.69437893277111));
#53487=CARTESIAN_POINT('Ctrl Pts',(0.990189583399944,-14.0274553092097,
-9.70977763601441));
#53488=CARTESIAN_POINT('Ctrl Pts',(0.75648966765497,-14.0279636369144,-9.72505909250718));
#53489=CARTESIAN_POINT('Ctrl Pts',(0.523354771819489,-14.028245554676,-9.73485846362861));
#53490=CARTESIAN_POINT('Ctrl Pts',(0.291007625024935,-14.0283672016567,
-9.73930374711879));
#53491=CARTESIAN_POINT('Ctrl Pts',(0.193861948610386,-14.0284180629579,
-9.74116234567472));
#53492=CARTESIAN_POINT('Ctrl Pts',(0.0968539805059063,-14.0284409565461,
-9.74208560497615));
#53493=CARTESIAN_POINT('Ctrl Pts',(7.83699083554507E-14,-14.0284409287452,
-9.74208558080452));
#53494=CARTESIAN_POINT('Ctrl Pts',(-7.9714237465531E-7,-14.028440928745,
-9.74208558080432));
#53495=CARTESIAN_POINT('Ctrl Pts',(-1.59428481433331E-6,-14.0284409287448,
-9.74208558080406));
#53496=CARTESIAN_POINT('Ctrl Pts',(-2.39142724503642E-6,-14.0284409287445,
-9.74208558080373));
#53497=CARTESIAN_POINT('Ctrl Pts',(-0.230506176176072,-14.0284408616835,
-9.74208548711302));
#53498=CARTESIAN_POINT('Ctrl Pts',(-0.461891889173131,-14.0283107293459,
-9.73685239088828));
#53499=CARTESIAN_POINT('Ctrl Pts',(-0.693935715395254,-14.0279835403948,
-9.72623762050784));
#53500=CARTESIAN_POINT('Ctrl Pts',(-0.928010413572703,-14.0276534878517,
-9.71552994854139));
#53501=CARTESIAN_POINT('Ctrl Pts',(-1.16275479513849,-14.0271229008488,
-9.69934599832716));
#53502=CARTESIAN_POINT('Ctrl Pts',(-1.39793911692932,-14.0263272827681,
-9.67758619433263));
#53503=CARTESIAN_POINT('Ctrl Pts',(-1.63471589070468,-14.0255262774933,
-9.65567905295272));
#53504=CARTESIAN_POINT('Ctrl Pts',(-1.87193858261666,-14.0244566259444,
-9.62812035587519));
#53505=CARTESIAN_POINT('Ctrl Pts',(-2.10937275100279,-14.0230570272121,
-9.59486143413018));
#53506=CARTESIAN_POINT('Ctrl Pts',(-2.34982868667985,-14.0216396161249,
-9.56117923412431));
#53507=CARTESIAN_POINT('Ctrl Pts',(-2.59050151590398,-14.0198837865677,
-9.52165084198971));
#53508=CARTESIAN_POINT('Ctrl Pts',(-2.83114773156445,-14.0177307442246,
-9.47627906946699));
#53509=CARTESIAN_POINT('Ctrl Pts',(-2.93418571946641,-14.0168088716313,
-9.45685214378084));
#53510=CARTESIAN_POINT('Ctrl Pts',(-3.03721882826862,-14.0158142395614,
-9.43635459918357));
#53511=CARTESIAN_POINT('Ctrl Pts',(-3.14022794330804,-14.0147425141972,
-9.41478954778385));
#53512=CARTESIAN_POINT('Ctrl Pts',(-3.40298087450609,-14.012008785432,-9.3597819839916));
#53513=CARTESIAN_POINT('Ctrl Pts',(-3.66557292847633,-14.0087547923374,
-9.29780917364166));
#53514=CARTESIAN_POINT('Ctrl Pts',(-3.92766534880194,-14.0047774817881,
-9.22884775196303));
#53515=CARTESIAN_POINT('Ctrl Pts',(-4.19885783938051,-14.0006620756565,
-9.15749193146415));
#53516=CARTESIAN_POINT('Ctrl Pts',(-4.46951539858308,-13.9957721838197,
-9.07865430510139));
#53517=CARTESIAN_POINT('Ctrl Pts',(-4.7392627449362,-13.9898918314853,-8.99236905962181));
#53518=CARTESIAN_POINT('Ctrl Pts',(-5.03507315963629,-13.98344331777,-8.89774690821647));
#53519=CARTESIAN_POINT('Ctrl Pts',(-5.32978897414251,-13.9758034680593,
-8.79416873779773));
#53520=CARTESIAN_POINT('Ctrl Pts',(-5.62291527875815,-13.9667005606775,
-8.68174476322627));
#53521=CARTESIAN_POINT('Ctrl Pts',(-5.83748008953337,-13.9600373456432,
-8.59945181151676));
#53522=CARTESIAN_POINT('Ctrl Pts',(-6.05119323169097,-13.952590488428,-8.51242073270881));
#53523=CARTESIAN_POINT('Ctrl Pts',(-6.26386060007216,-13.9442583528048,
-8.42071136807365));
#53524=CARTESIAN_POINT('Ctrl Pts',(6.38247011518717,-13.9383842293975,-8.36786575295797));
#53525=CARTESIAN_POINT('Ctrl Pts',(5.83976911340181,-13.9679622540055,-8.61443012698678));
#53526=CARTESIAN_POINT('Ctrl Pts',(4.5258368467239,-14.0220349167051,-9.12803247901763));
#53527=CARTESIAN_POINT('Ctrl Pts',(2.38629932644282,-14.0625377999656,-9.65166978692595));
#53528=CARTESIAN_POINT('Ctrl Pts',(0.000145959755059722,-14.0741398126941,
-9.84427564872159));
#53529=CARTESIAN_POINT('Ctrl Pts',(-2.38600750188862,-14.0625408462426,
-9.65171698481383));
#53530=CARTESIAN_POINT('Ctrl Pts',(-4.52564624096925,-14.0220410567715,
-9.12809880319294));
#53531=CARTESIAN_POINT('Ctrl Pts',(-5.83967376427529,-13.9679673726684,
-8.6144731341098));
#53532=CARTESIAN_POINT('Ctrl Pts',(-6.38246545188257,-13.9383844561507,
-8.36786779269362));
#53533=CARTESIAN_POINT('Ctrl Pts',(6.177925724167,-13.466791063603,-7.96585293951407));
#53534=CARTESIAN_POINT('Ctrl Pts',(5.65233905480535,-13.4969066625404,-8.20307837018344));
#53535=CARTESIAN_POINT('Ctrl Pts',(4.37999194810445,-13.5523366915063,-8.69728215770289));
#53536=CARTESIAN_POINT('Ctrl Pts',(2.30900032384948,-13.5946978059676,-9.20108707500959));
#53537=CARTESIAN_POINT('Ctrl Pts',(0.000141220875385398,-13.6070941366454,
-9.38635631507042));
#53538=CARTESIAN_POINT('Ctrl Pts',(-2.30871791260755,-13.5947010396693,
-9.20113247851775));
#53539=CARTESIAN_POINT('Ctrl Pts',(-4.3798073931949,-13.5523430345878,-8.69734597758452));
#53540=CARTESIAN_POINT('Ctrl Pts',(-5.65224671339352,-13.496911875029,-8.2031197495587));
#53541=CARTESIAN_POINT('Ctrl Pts',(-6.1779212078179,-13.4667912943994,-7.96585490328432));
#53542=CARTESIAN_POINT('Ctrl Pts',(6.17628879660483,-12.8196117922142,-8.03444678682366));
#53543=CARTESIAN_POINT('Ctrl Pts',(5.65205474344145,-12.8494195568757,-8.26881665925291));
#53544=CARTESIAN_POINT('Ctrl Pts',(4.38232924763575,-12.9043202327645,-8.75753222014369));
#53545=CARTESIAN_POINT('Ctrl Pts',(2.31198089188489,-12.9463013545954,-9.25697094634347));
#53546=CARTESIAN_POINT('Ctrl Pts',(0.000141450441422552,-12.9585829054207,
-9.44098574409741));
#53547=CARTESIAN_POINT('Ctrl Pts',(-2.31169828944397,-12.9463045599124,
-9.25701601862634));
#53548=CARTESIAN_POINT('Ctrl Pts',(-4.38214499322134,-12.9043265148673,
-8.75759539236768));
#53549=CARTESIAN_POINT('Ctrl Pts',(-5.65196263603526,-12.8494247211796,
-8.26885754201286));
#53550=CARTESIAN_POINT('Ctrl Pts',(-6.17628429233524,-12.8196120244309,
-8.03444872628162));
#53551=CARTESIAN_POINT('Ctrl Pts',(6.376125622901,-12.4394717503676,-8.52105869970914));
#53552=CARTESIAN_POINT('Ctrl Pts',(5.83675988447364,-12.4683463754376,-8.76091826903374));
#53553=CARTESIAN_POINT('Ctrl Pts',(4.5293976034514,-12.5212149055004,-9.2616161521347));
#53554=CARTESIAN_POINT('Ctrl Pts',(2.39220470509012,-12.5608645076069,-9.7749319909605));
#53555=CARTESIAN_POINT('Ctrl Pts',(0.000146429844990828,-12.5722117056496,
-9.96455183631497));
#53556=CARTESIAN_POINT('Ctrl Pts',(-2.39191255764638,-12.5608674907541,
-9.77497840220907));
#53557=CARTESIAN_POINT('Ctrl Pts',(-4.52920776688929,-12.5212209074462,
-9.26168095077238));
#53558=CARTESIAN_POINT('Ctrl Pts',(-5.83666511294557,-12.4683513841291,
-8.7609601100695));
#53559=CARTESIAN_POINT('Ctrl Pts',(-6.37612098930916,-12.4394719804615,
-8.52106068240773));
#53560=CARTESIAN_POINT('',(-6.24994532672558,-12.462652132724,-8.55169075504561));
#53561=CARTESIAN_POINT('Origin',(-6.5277204968019,-13.2547548639173,-9.09521590379488));
#53562=CARTESIAN_POINT('Ctrl Pts',(6.24994435006576,-12.4626487224143,-8.5516910297148));
#53563=CARTESIAN_POINT('Ctrl Pts',(5.93520863610954,-12.478935053609,-8.68880231996198));
#53564=CARTESIAN_POINT('Ctrl Pts',(5.61561497397808,-12.4930288863896,-8.81654384237152));
#53565=CARTESIAN_POINT('Ctrl Pts',(5.29150042771701,-12.5052897567797,-8.93429441879265));
#53566=CARTESIAN_POINT('Ctrl Pts',(5.10416783972639,-12.5123763272767,-9.00235221031365));
#53567=CARTESIAN_POINT('Ctrl Pts',(4.9153250937991,-12.5188505341334,-9.06707147399993));
#53568=CARTESIAN_POINT('Ctrl Pts',(4.72503881885995,-12.5247817359611,-9.12832441192078));
#53569=CARTESIAN_POINT('Ctrl Pts',(4.72121098795688,-12.5249010490206,-9.12955658638399));
#53570=CARTESIAN_POINT('Ctrl Pts',(4.71738257406758,-12.5250201403348,-9.13078736032785));
#53571=CARTESIAN_POINT('Ctrl Pts',(4.71355357757958,-12.5251390103775,-9.13201673287128));
#53572=CARTESIAN_POINT('Ctrl Pts',(4.45754789802082,-12.5330866295876,-9.21421225182763));
#53573=CARTESIAN_POINT('Ctrl Pts',(4.19893806746814,-12.5400452191779,-9.29014571126507));
#53574=CARTESIAN_POINT('Ctrl Pts',(3.93791724033779,-12.5461419619073,-9.35956663918277));
#53575=CARTESIAN_POINT('Ctrl Pts',(3.80545482353562,-12.5492359268045,-9.39479625664174));
#53576=CARTESIAN_POINT('Ctrl Pts',(3.67237176886856,-12.5521072046937,-9.42834905312878));
#53577=CARTESIAN_POINT('Ctrl Pts',(3.53869508005236,-12.5547679555686,-9.46019456380016));
#53578=CARTESIAN_POINT('Ctrl Pts',(3.47185673564426,-12.556098331006,-9.47611731913585));
#53579=CARTESIAN_POINT('Ctrl Pts',(3.40486997931727,-12.5573760590713,-9.49161324128445));
#53580=CARTESIAN_POINT('Ctrl Pts',(3.33773832833752,-12.5586023421897,-9.50667870912308));
#53581=CARTESIAN_POINT('Ctrl Pts',(3.30417250284765,-12.5592154837489,-9.51421144304239));
#53582=CARTESIAN_POINT('Ctrl Pts',(3.27057045352523,-12.5598157631269,-9.52163656266291));
#53583=CARTESIAN_POINT('Ctrl Pts',(3.23693262388625,-12.5604033178904,-9.52895361921054));
#53584=CARTESIAN_POINT('Ctrl Pts',(3.20933465675268,-12.5608853738739,-9.53495685688323));
#53585=CARTESIAN_POINT('Ctrl Pts',(3.180755829783,-12.5613750545733,-9.54109103135349));
#53586=CARTESIAN_POINT('Ctrl Pts',(3.15355121784076,-12.5618325282578,-9.54685408039594));
#53587=CARTESIAN_POINT('Ctrl Pts',(3.14759744179454,-12.5619326471593,-9.54811533357665));
#53588=CARTESIAN_POINT('Ctrl Pts',(3.14170952969673,-12.5620312448056,-9.54935900566632));
#53589=CARTESIAN_POINT('Ctrl Pts',(3.13591223970834,-12.5621279382662,-9.55058015248305));
#53590=CARTESIAN_POINT('Ctrl Pts',(2.87755178205346,-12.5664371528765,-9.60500145123953));
#53591=CARTESIAN_POINT('Ctrl Pts',(2.61814577474157,-12.5700203191151,-9.652793457199));
#53592=CARTESIAN_POINT('Ctrl Pts',(2.3578840641493,-12.5730153521193,-9.69382346594162));
#53593=CARTESIAN_POINT('Ctrl Pts',(2.0559289187946,-12.5764901837573,-9.74142640463585));
#53594=CARTESIAN_POINT('Ctrl Pts',(1.75282198464787,-12.5791732609632,-9.77992868385661));
#53595=CARTESIAN_POINT('Ctrl Pts',(1.44895725672518,-12.5811590067854,-9.80926917466022));
#53596=CARTESIAN_POINT('Ctrl Pts',(1.14576931107835,-12.5831403298582,-9.83854431689812));
#53597=CARTESIAN_POINT('Ctrl Pts',(0.841826368189186,-12.5844273449745,
-9.85869852518057));
#53598=CARTESIAN_POINT('Ctrl Pts',(0.537511110199068,-12.5851093061151,
-9.86962038034393));
#53599=CARTESIAN_POINT('Ctrl Pts',(0.358491817075135,-12.5855104828492,
-9.87604537133472));
#53600=CARTESIAN_POINT('Ctrl Pts',(0.179343559716909,-12.5857021945379,
-9.8792744456513));
#53601=CARTESIAN_POINT('Ctrl Pts',(0.000144045323212458,-12.5857020417033,
-9.87927649693224));
#53602=CARTESIAN_POINT('Ctrl Pts',(9.53568818153291E-5,-12.5857020416617,
-9.87927649748958));
#53603=CARTESIAN_POINT('Ctrl Pts',(4.66684366375151E-5,-12.585702041606,
-9.87927649780865));
#53604=CARTESIAN_POINT('Ctrl Pts',(-2.02001232150136E-6,-12.5857020415362,
-9.87927649788946));
#53605=CARTESIAN_POINT('Ctrl Pts',(-0.298119005239199,-12.5857016138055,
-9.87927699270075));
#53606=CARTESIAN_POINT('Ctrl Pts',(-0.596080646488231,-12.5851365239961,
-9.87039237637331));
#53607=CARTESIAN_POINT('Ctrl Pts',(-0.89354275403253,-12.5839683223329,
-9.85270238622077));
#53608=CARTESIAN_POINT('Ctrl Pts',(-1.1210836629543,-12.5830747171929,-9.83917059062046));
#53609=CARTESIAN_POINT('Ctrl Pts',(-1.34833217344988,-12.5818281693976,
-9.82048537709595));
#53610=CARTESIAN_POINT('Ctrl Pts',(-1.57512820480823,-12.5802099836666,
-9.79666281776233));
#53611=CARTESIAN_POINT('Ctrl Pts',(-1.83662850139142,-12.5783441836081,
-9.76919493706882));
#53612=CARTESIAN_POINT('Ctrl Pts',(-2.09753059605828,-12.575973201931,-9.73491182923078));
#53613=CARTESIAN_POINT('Ctrl Pts',(-2.35759908107191,-12.5729990046887,
-9.69389384419149));
#53614=CARTESIAN_POINT('Ctrl Pts',(-2.35774019131026,-12.5729973909227,
-9.69387158829361));
#53615=CARTESIAN_POINT('Ctrl Pts',(-2.35788130130321,-12.572995776979,-9.69384933041219));
#53616=CARTESIAN_POINT('Ctrl Pts',(-2.35802241105073,-12.5729941628576,
-9.69382707054729));
#53617=CARTESIAN_POINT('Ctrl Pts',(-2.48812675613284,-12.5715059297154,
-9.67330329245208));
#53618=CARTESIAN_POINT('Ctrl Pts',(-2.61802246404346,-12.5698659514544,
-9.65109436515554));
#53619=CARTESIAN_POINT('Ctrl Pts',(-2.74768075918299,-12.5680600288683,
-9.6272147285293));
#53620=CARTESIAN_POINT('Ctrl Pts',(-2.81250990675276,-12.5671570675753,
-9.61527491021618));
#53621=CARTESIAN_POINT('Ctrl Pts',(-2.87727970070071,-12.5662126091452,
-9.6029174058796));
#53622=CARTESIAN_POINT('Ctrl Pts',(-2.9419865920507,-12.5652245964307,-9.59014423675178));
#53623=CARTESIAN_POINT('Ctrl Pts',(-2.97434003772569,-12.5647305900734,
-9.58375765218786));
#53624=CARTESIAN_POINT('Ctrl Pts',(-3.00667775770639,-12.564225694429,-9.57726715086189));
#53625=CARTESIAN_POINT('Ctrl Pts',(-3.03899930980661,-12.5637096414949,
-9.57067299017703));
#53626=CARTESIAN_POINT('Ctrl Pts',(-3.06566659180715,-12.5632838658676,
-9.56523239926745));
#53627=CARTESIAN_POINT('Ctrl Pts',(-3.09135655462812,-12.5628663941347,
-9.55992271288502));
#53628=CARTESIAN_POINT('Ctrl Pts',(-3.11846086046902,-12.562417769849,-9.55424587330949));
#53629=CARTESIAN_POINT('Ctrl Pts',(-3.12420779283676,-12.5623226479358,
-9.55304221167379));
#53630=CARTESIAN_POINT('Ctrl Pts',(-3.13001826947044,-12.5622261062038,
-9.55182186515024));
#53631=CARTESIAN_POINT('Ctrl Pts',(-3.13591502092693,-12.5621277362302,
-9.55057978976115));
#53632=CARTESIAN_POINT('Ctrl Pts',(-3.45257930704656,-12.5568451229652,
-9.48387850189209));
#53633=CARTESIAN_POINT('Ctrl Pts',(-3.76614685428018,-12.5505102571087,
-9.40752256927021));
#53634=CARTESIAN_POINT('Ctrl Pts',(-4.07624236026289,-12.5429015342422,
-9.32200266916992));
#53635=CARTESIAN_POINT('Ctrl Pts',(-4.29026496940007,-12.5376501239874,
-9.26297829829228));
#53636=CARTESIAN_POINT('Ctrl Pts',(-4.50263387066465,-12.5317919731508,
-9.19958748653664));
#53637=CARTESIAN_POINT('Ctrl Pts',(-4.71322682841913,-12.5252544390584,
-9.13197721008274));
#53638=CARTESIAN_POINT('Ctrl Pts',(-5.02876448392235,-12.5154590584232,
-9.03067473374325));
#53639=CARTESIAN_POINT('Ctrl Pts',(-5.34031574361354,-12.5041386185149,
-8.91990198233565));
#53640=CARTESIAN_POINT('Ctrl Pts',(-5.64761398272241,-12.4910219758922,
-8.80016008656025));
#53641=CARTESIAN_POINT('Ctrl Pts',(-5.85026677362467,-12.4823719938992,
-8.72119435790141));
#53642=CARTESIAN_POINT('Ctrl Pts',(-6.0510698467664,-12.4729408293642,-8.63832685047973));
#53643=CARTESIAN_POINT('Ctrl Pts',(-6.24994452572252,-12.4626498485398,
-8.55168918768589));
#53644=CARTESIAN_POINT('Ctrl Pts',(-6.24277095337913,-13.9570481133821,
-8.44169435429085));
#53645=CARTESIAN_POINT('Ctrl Pts',(-6.29815583077892,-13.9532401195528,
-8.41824340131205));
#53646=CARTESIAN_POINT('Ctrl Pts',(-6.4447418010428,-13.9493436454455,-8.34436057253389));
#53647=CARTESIAN_POINT('Ctrl Pts',(-6.66526187295068,-13.9714492594668,
-8.17939903115658));
#53648=CARTESIAN_POINT('Ctrl Pts',(-6.87369344496963,-14.036253579378,-7.93773816682672));
#53649=CARTESIAN_POINT('Ctrl Pts',(-7.019185666524,-14.1323671765394,-7.66828606903858));
#53650=CARTESIAN_POINT('Ctrl Pts',(-7.0965183656736,-14.2455227590742,-7.40111221773899));
#53651=CARTESIAN_POINT('Ctrl Pts',(-7.10969901122602,-14.3273043817824,
-7.23055752275661));
#53652=CARTESIAN_POINT('Ctrl Pts',(-7.10784879432356,-14.3669526800853,
-7.15228421614289));
#53653=CARTESIAN_POINT('Ctrl Pts',(-6.04395576815581,-13.495653564219,-8.0326875434042));
#53654=CARTESIAN_POINT('Ctrl Pts',(-6.09276946049994,-13.4920218131833,
-8.01223198182578));
#53655=CARTESIAN_POINT('Ctrl Pts',(-6.22228199799112,-13.4876402372165,
-7.94771003933163));
#53656=CARTESIAN_POINT('Ctrl Pts',(-6.41829649695095,-13.5050515638676,
-7.80303765417474));
#53657=CARTESIAN_POINT('Ctrl Pts',(-6.60464059843952,-13.5598578050206,
-7.59012754325846));
#53658=CARTESIAN_POINT('Ctrl Pts',(-6.73521158016175,-13.6429459389554,
-7.35210380136168));
#53659=CARTESIAN_POINT('Ctrl Pts',(-6.80469368075153,-13.7418688573599,
-7.1160681283494));
#53660=CARTESIAN_POINT('Ctrl Pts',(-6.81649571475142,-13.8137195396554,
-6.96583884061849));
#53661=CARTESIAN_POINT('Ctrl Pts',(-6.81483976643568,-13.8485536822665,
-6.89712306094761));
#53662=CARTESIAN_POINT('Ctrl Pts',(-6.02805601653886,-12.8501482256791,
-8.09057476185638));
#53663=CARTESIAN_POINT('Ctrl Pts',(-6.09538291160628,-12.8454029891221,
-8.06277674238425));
#53664=CARTESIAN_POINT('Ctrl Pts',(-6.27265850281004,-12.8403106482999,
-7.9757587629418));
#53665=CARTESIAN_POINT('Ctrl Pts',(-6.53595054453926,-12.8655837800627,
-7.7844790925534));
#53666=CARTESIAN_POINT('Ctrl Pts',(-6.78171371030984,-12.9396065336219,
-7.50843369672343));
#53667=CARTESIAN_POINT('Ctrl Pts',(-6.95183436866027,-13.0485085954569,
-7.20361737708373));
#53668=CARTESIAN_POINT('Ctrl Pts',(-7.04202608316068,-13.1761754239708,
-6.90252126095774));
#53669=CARTESIAN_POINT('Ctrl Pts',(-7.05751522705347,-13.2686270590318,
-6.7097519791209));
#53670=CARTESIAN_POINT('Ctrl Pts',(-7.05533880391617,-13.313666237071,-6.62082661348952));
#53671=CARTESIAN_POINT('Ctrl Pts',(-6.20650780120442,-12.4602299621517,
-8.57738035221049));
#53672=CARTESIAN_POINT('Ctrl Pts',(-6.30488566866451,-12.453836841744,-8.5368768391189));
#53673=CARTESIAN_POINT('Ctrl Pts',(-6.56239159754601,-12.4482921495602,
-8.41074728563732));
#53674=CARTESIAN_POINT('Ctrl Pts',(-6.9391515270053,-12.4886612913967,-8.13753809672886));
#53675=CARTESIAN_POINT('Ctrl Pts',(-7.28557450517007,-12.5981021554977,
-7.7492384229932));
#53676=CARTESIAN_POINT('Ctrl Pts',(-7.5229153234017,-12.7541756117298,-7.324649770896));
#53677=CARTESIAN_POINT('Ctrl Pts',(-7.64834332712291,-12.9340958564118,
-6.9063608319225));
#53678=CARTESIAN_POINT('Ctrl Pts',(-7.67008672986089,-13.0637272878827,
-6.63699912917934));
#53679=CARTESIAN_POINT('Ctrl Pts',(-7.66702778969363,-13.1270784697037,
-6.51178563799198));
#53680=CARTESIAN_POINT('',(-7.00001043113205,-13.9487143148388,-6.97711954537448));
#53681=CARTESIAN_POINT('',(-7.00000027445394,-12.5220632044943,-8.04447892907881));
#53682=CARTESIAN_POINT('Ctrl Pts',(-7.,-13.9487143149799,-6.97711954518352));
#53683=CARTESIAN_POINT('Ctrl Pts',(-7.,-13.845491146465,-7.02162187524465));
#53684=CARTESIAN_POINT('Ctrl Pts',(-7.,-13.754333549677,-7.0634883841343));
#53685=CARTESIAN_POINT('Ctrl Pts',(-7.,-13.6767079632962,-7.10164870932265));
#53686=CARTESIAN_POINT('Ctrl Pts',(-7.,-13.6378951701058,-7.12072887191683));
#53687=CARTESIAN_POINT('Ctrl Pts',(-7.,-13.6024393883131,-7.13883660024732));
#53688=CARTESIAN_POINT('Ctrl Pts',(-7.,-13.5703851007164,-7.15566494585842));
#53689=CARTESIAN_POINT('Ctrl Pts',(-7.,-13.5543579569181,-7.16407911866396));
#53690=CARTESIAN_POINT('Ctrl Pts',(-7.,-13.5391800633319,-7.17217227343122));
#53691=CARTESIAN_POINT('Ctrl Pts',(-7.,-13.5248512234156,-7.17990207217249));
#53692=CARTESIAN_POINT('Ctrl Pts',(-7.,-13.5176868034574,-7.18376697154313));
#53693=CARTESIAN_POINT('Ctrl Pts',(-7.,-13.5107346469166,-7.18754103190727));
#53694=CARTESIAN_POINT('Ctrl Pts',(-7.,-13.5039943937985,-7.19121892813308));
#53695=CARTESIAN_POINT('Ctrl Pts',(-7.,-13.5006242672395,-7.19305787624598));
#53696=CARTESIAN_POINT('Ctrl Pts',(-7.,-13.4973071165361,-7.19487278332431));
#53697=CARTESIAN_POINT('Ctrl Pts',(-7.,-13.4940428913842,-7.19666299402289));
#53698=CARTESIAN_POINT('Ctrl Pts',(-7.,-13.4907786662322,-7.19845320472147));
#53699=CARTESIAN_POINT('Ctrl Pts',(-7.,-13.4891249577557,-7.19936055090131));
#53700=CARTESIAN_POINT('Ctrl Pts',(-7.,-13.4844089378928,-7.2019588837331));
#53701=CARTESIAN_POINT('Ctrl Pts',(-7.,-13.4089526200857,-7.24353220904171));
#53702=CARTESIAN_POINT('Ctrl Pts',(-7.,-13.3377436713999,-7.28579001561386));
#53703=CARTESIAN_POINT('Ctrl Pts',(-7.,-13.2712863644665,-7.32835269250401));
#53704=CARTESIAN_POINT('Ctrl Pts',(-7.,-13.2048290575331,-7.37091536939417));
#53705=CARTESIAN_POINT('Ctrl Pts',(-7.,-13.1443246620373,-7.41287378405723));
#53706=CARTESIAN_POINT('Ctrl Pts',(-7.,-13.0863576832307,-7.45602150139235));
#53707=CARTESIAN_POINT('Ctrl Pts',(-7.,-12.9704237256174,-7.54231693606261));
#53708=CARTESIAN_POINT('Ctrl Pts',(-7.,-12.8624865278623,-7.63585832171496));
#53709=CARTESIAN_POINT('Ctrl Pts',(-7.,-12.7672163298947,-7.73520842630034));
#53710=CARTESIAN_POINT('Ctrl Pts',(-7.,-12.6719461319271,-7.83455853088573));
#53711=CARTESIAN_POINT('Ctrl Pts',(-7.,-12.5894789845998,-7.93953599603716));
#53712=CARTESIAN_POINT('Ctrl Pts',(-7.,-12.5220635189387,-8.04447812614683));
#53713=CARTESIAN_POINT('Ctrl Pts',(-6.24994591284326,-12.4626538041299,
-8.55169190192368));
#53714=CARTESIAN_POINT('Ctrl Pts',(-6.29984502952175,-12.4600715183856,
-8.5299538017944));
#53715=CARTESIAN_POINT('Ctrl Pts',(-6.34871496710572,-12.4586373900724,
-8.50669099475367));
#53716=CARTESIAN_POINT('Ctrl Pts',(-6.39657992048361,-12.4582954827157,
-8.48197367229514));
#53717=CARTESIAN_POINT('Ctrl Pts',(-6.42793514231834,-12.458071507129,-8.46578192710052));
#53718=CARTESIAN_POINT('Ctrl Pts',(-6.45885896943399,-12.4583168141412,
-8.44896505528031));
#53719=CARTESIAN_POINT('Ctrl Pts',(-6.48935513207306,-12.4590220513095,
-8.43153301532157));
#53720=CARTESIAN_POINT('Ctrl Pts',(-6.53665120488326,-12.4601157937863,
-8.40449790795816));
#53721=CARTESIAN_POINT('Ctrl Pts',(-6.58292002814214,-12.4623144775476,
-8.37598485615482));
#53722=CARTESIAN_POINT('Ctrl Pts',(-6.62819544396853,-12.465585688379,-8.34601162845821));
#53723=CARTESIAN_POINT('Ctrl Pts',(-6.63503349783147,-12.4660797471404,
-8.34148470050637));
#53724=CARTESIAN_POINT('Ctrl Pts',(-6.64184884345374,-12.4665983213324,
-8.3369243973713));
#53725=CARTESIAN_POINT('Ctrl Pts',(-6.64864154412372,-12.467141352241,-8.33233071027927));
#53726=CARTESIAN_POINT('Ctrl Pts',(-6.69594096035842,-12.4709226236704,
-8.30034362173017));
#53727=CARTESIAN_POINT('Ctrl Pts',(-6.74212293424803,-12.4758915212378,
-8.26674704428514));
#53728=CARTESIAN_POINT('Ctrl Pts',(-6.78718061207176,-12.4820430406497,
-8.23152520023946));
#53729=CARTESIAN_POINT('Ctrl Pts',(-6.83223828989548,-12.4881945600615,
-8.19630335619378));
#53730=CARTESIAN_POINT('Ctrl Pts',(-6.87617234032553,-12.4955288522721,
-8.15945574064839));
#53731=CARTESIAN_POINT('Ctrl Pts',(-6.91893148542368,-12.5040687076553,
-8.12093600965497));
#53732=CARTESIAN_POINT('Ctrl Pts',(-6.94644685185362,-12.5095640759464,
-8.09614869197979));
#53733=CARTESIAN_POINT('Ctrl Pts',(-6.97347471723017,-12.5155592318714,
-8.07066836258662));
#53734=CARTESIAN_POINT('Ctrl Pts',(-7.00000082162213,-12.5220620483258,
-8.04447919620794));
#53735=CARTESIAN_POINT('Ctrl Pts',(-6.26385534042556,-13.9442720969407,
-8.42069792283772));
#53736=CARTESIAN_POINT('Ctrl Pts',(-6.30612913172524,-13.9334276586312,
-8.393074980389));
#53737=CARTESIAN_POINT('Ctrl Pts',(-6.34794395424447,-13.9237064047667,
-8.3623944118752));
#53738=CARTESIAN_POINT('Ctrl Pts',(-6.38887223123086,-13.9151877588231,
-8.32867404218946));
#53739=CARTESIAN_POINT('Ctrl Pts',(-6.43384340086241,-13.9058276415651,
-8.29162277649167));
#53740=CARTESIAN_POINT('Ctrl Pts',(-6.47774452173498,-13.897919689472,-8.25090041315255));
#53741=CARTESIAN_POINT('Ctrl Pts',(-6.52005084106735,-13.8914885296134,
-8.2066635433403));
#53742=CARTESIAN_POINT('Ctrl Pts',(-6.53777952753404,-13.8887935181222,
-8.18812584950294));
#53743=CARTESIAN_POINT('Ctrl Pts',(-6.55522760709187,-13.886357991745,-8.16897117842091));
#53744=CARTESIAN_POINT('Ctrl Pts',(-6.57235390700123,-13.8841845943505,
-8.14921175211991));
#53745=CARTESIAN_POINT('Ctrl Pts',(-6.5861973044387,-13.8824278106855,-8.13323996645292));
#53746=CARTESIAN_POINT('Ctrl Pts',(-6.59983046404273,-13.8808423141501,
-8.11687304420284));
#53747=CARTESIAN_POINT('Ctrl Pts',(-6.61323083027859,-13.8794298320133,
-8.10011755820082));
#53748=CARTESIAN_POINT('Ctrl Pts',(-6.64590221527833,-13.8759860643667,
-8.05926606769717));
#53749=CARTESIAN_POINT('Ctrl Pts',(-6.67719137476755,-13.8735702711939,
-8.01610413538155));
#53750=CARTESIAN_POINT('Ctrl Pts',(-6.70681950479909,-13.8721615260151,
-7.97079335835709));
#53751=CARTESIAN_POINT('Ctrl Pts',(-6.72770964821358,-13.8711682507464,
-7.93884572517013));
#53752=CARTESIAN_POINT('Ctrl Pts',(-6.74777362032552,-13.8706757328006,
-7.90583003453161));
#53753=CARTESIAN_POINT('Ctrl Pts',(-6.76690562480041,-13.8706795466101,
-7.87180523652566));
#53754=CARTESIAN_POINT('Ctrl Pts',(-6.77618565666782,-13.870681396509,-7.85530141382417));
#53755=CARTESIAN_POINT('Ctrl Pts',(-6.78524634454529,-13.8708000658958,
-7.8385601337316));
#53756=CARTESIAN_POINT('Ctrl Pts',(-6.79407489018008,-13.8710353077612,
-7.82158832904041));
#53757=CARTESIAN_POINT('Ctrl Pts',(-6.7943469477008,-13.8710425568961,-7.82106533156185));
#53758=CARTESIAN_POINT('Ctrl Pts',(-6.79461878474062,-13.8710499167433,
-7.82054211518253));
#53759=CARTESIAN_POINT('Ctrl Pts',(-6.79489040101669,-13.8710573872386,
-7.82001868017595));
#53760=CARTESIAN_POINT('Ctrl Pts',(-6.7994333225514,-13.8711823351039,-7.81126396121066));
#53761=CARTESIAN_POINT('Ctrl Pts',(-6.80391449395765,-13.8713382356806,
-7.80244807312468));
#53762=CARTESIAN_POINT('Ctrl Pts',(-6.80833258184899,-13.8715247945615,
-7.79357229387828));
#53763=CARTESIAN_POINT('Ctrl Pts',(-6.81054162579466,-13.871618074002,-7.78913440425508));
#53764=CARTESIAN_POINT('Ctrl Pts',(-6.81273489854703,-13.8717190181075,
-7.78468154176765));
#53765=CARTESIAN_POINT('Ctrl Pts',(-6.81491223129425,-13.8718275909203,
-7.78021386629139));
#53766=CARTESIAN_POINT('Ctrl Pts',(-6.81652751824644,-13.8719081372897,
-7.77689945423717));
#53767=CARTESIAN_POINT('Ctrl Pts',(-6.81855728648138,-13.8720156889984,
-7.77269732427786));
#53768=CARTESIAN_POINT('Ctrl Pts',(-6.82005848244088,-13.8720999717879,
-7.76956453127851));
#53769=CARTESIAN_POINT('Ctrl Pts',(-6.82058082980177,-13.8721292983341,
-7.76847446295995));
#53770=CARTESIAN_POINT('Ctrl Pts',(-6.82103962979231,-13.8721555817735,
-7.7675141188402));
#53771=CARTESIAN_POINT('Ctrl Pts',(-6.82139623906195,-13.8721761601389,
-7.76676656116145));
#53772=CARTESIAN_POINT('Ctrl Pts',(-6.83575184946987,-13.8730045597979,
-7.73667298898843));
#53773=CARTESIAN_POINT('Ctrl Pts',(-6.85002639449847,-13.874185312472,-7.70455942481883));
#53774=CARTESIAN_POINT('Ctrl Pts',(-6.86393641265041,-13.8758132973589,
-7.670365998745));
#53775=CARTESIAN_POINT('Ctrl Pts',(-6.87708941310866,-13.8773526832698,
-7.63803346374));
#53776=CARTESIAN_POINT('Ctrl Pts',(-6.88991660308488,-13.8792919442696,
-7.60384113002283));
#53777=CARTESIAN_POINT('Ctrl Pts',(-6.90213804711071,-13.8817125104589,
-7.56776145381844));
#53778=CARTESIAN_POINT('Ctrl Pts',(-6.90769941303009,-13.8828139886707,
-7.55134340361085));
#53779=CARTESIAN_POINT('Ctrl Pts',(-6.91313476695845,-13.8840151483965,
-7.53453488091171));
#53780=CARTESIAN_POINT('Ctrl Pts',(-6.91841458762728,-13.8853237667971,
-7.51733513890366));
#53781=CARTESIAN_POINT('Ctrl Pts',(-6.92704805286015,-13.887463595434,-7.48921043847256));
#53782=CARTESIAN_POINT('Ctrl Pts',(-6.93526621074753,-13.889890883691,-7.46003892947911));
#53783=CARTESIAN_POINT('Ctrl Pts',(-6.94294163685135,-13.8926328856932,
-7.42983414009522));
#53784=CARTESIAN_POINT('Ctrl Pts',(-6.95237988057618,-13.896004644191,-7.39269220686497));
#53785=CARTESIAN_POINT('Ctrl Pts',(-6.96099870250611,-13.8998523152925,
-7.35398679499351));
#53786=CARTESIAN_POINT('Ctrl Pts',(-6.96853214253001,-13.9042238202432,
-7.31377108169759));
#53787=CARTESIAN_POINT('Ctrl Pts',(-6.97439397820933,-13.9076253265419,
-7.28247888287218));
#53788=CARTESIAN_POINT('Ctrl Pts',(-6.97959814398842,-13.9113439203884,
-7.25027282717614));
#53789=CARTESIAN_POINT('Ctrl Pts',(-6.98400299079825,-13.9154010683865,
-7.21719263050833));
#53790=CARTESIAN_POINT('Ctrl Pts',(-6.98927533587738,-13.920257238239,-7.17759756179238));
#53791=CARTESIAN_POINT('Ctrl Pts',(-6.99340294124102,-13.9255988112762,
-7.1367486794794));
#53792=CARTESIAN_POINT('Ctrl Pts',(-6.99614956769376,-13.9314442793002,
-7.09476435678002));
#53793=CARTESIAN_POINT('Ctrl Pts',(-6.99865578183743,-13.9367780933046,
-7.05645492330856));
#53794=CARTESIAN_POINT('Ctrl Pts',(-7.00001226545564,-13.9425313541841,
-7.01720035980972));
#53795=CARTESIAN_POINT('Ctrl Pts',(-7.00001530585652,-13.9487143147908,
-6.97711954573686));
#53796=CARTESIAN_POINT('Ctrl Pts',(-6.23412706809605,-24.3933911327703,
-11.8700326072878));
#53797=CARTESIAN_POINT('Ctrl Pts',(-6.23490236892324,-23.8924704339311,
-11.9504784732052));
#53798=CARTESIAN_POINT('Ctrl Pts',(-6.23649016701325,-22.7260268100557,
-12.0627656084535));
#53799=CARTESIAN_POINT('Ctrl Pts',(-6.23803702240708,-20.8893388269326,
-11.9701378589627));
#53800=CARTESIAN_POINT('Ctrl Pts',(-6.23758982654153,-18.9411592545323,
-11.5416382303731));
#53801=CARTESIAN_POINT('Ctrl Pts',(-6.23570065532116,-17.0892597438815,
-10.7961461814687));
#53802=CARTESIAN_POINT('Ctrl Pts',(-6.23204684345145,-15.3875898374077,
-9.7563195899027));
#53803=CARTESIAN_POINT('Ctrl Pts',(-6.22725829190456,-14.0755224934574,
-8.61699903004171));
#53804=CARTESIAN_POINT('Ctrl Pts',(-6.22399874199105,-13.3673849692544,
-7.81350344253181));
#53805=CARTESIAN_POINT('Ctrl Pts',(-6.22266320381891,-13.1134091391432,
-7.49367959650599));
#53806=CARTESIAN_POINT('Ctrl Pts',(-6.72598859051384,-24.3745664585965,
-11.7530878020866));
#53807=CARTESIAN_POINT('Ctrl Pts',(-6.7266817490657,-23.8785348888993,-11.8323472612636));
#53808=CARTESIAN_POINT('Ctrl Pts',(-6.72805001567041,-22.7235334782936,
-11.9427161005427));
#53809=CARTESIAN_POINT('Ctrl Pts',(-6.72941756715414,-20.9054810194554,
-11.8502334328646));
#53810=CARTESIAN_POINT('Ctrl Pts',(-6.72902256625366,-18.9767970133252,
-11.426261407818));
#53811=CARTESIAN_POINT('Ctrl Pts',(-6.72736650672518,-17.1431698816911,
-10.6891596966517));
#53812=CARTESIAN_POINT('Ctrl Pts',(-6.72416283555794,-15.4573996370106,
-9.66126047143717));
#53813=CARTESIAN_POINT('Ctrl Pts',(-6.71993196287863,-14.1564693360957,
-8.53486457539566));
#53814=CARTESIAN_POINT('Ctrl Pts',(-6.71707743903688,-13.4537908800506,
-7.74007194970102));
#53815=CARTESIAN_POINT('Ctrl Pts',(-6.71588870767409,-13.2016810518248,
-7.42369098479773));
#53816=CARTESIAN_POINT('Ctrl Pts',(-7.02718530998673,-24.31001596234,-11.3520775656941));
#53817=CARTESIAN_POINT('Ctrl Pts',(-7.02756400531626,-23.8309256023114,
-11.4283612752642));
#53818=CARTESIAN_POINT('Ctrl Pts',(-7.02824891920641,-22.715203036292,-11.5344334835993));
#53819=CARTESIAN_POINT('Ctrl Pts',(-7.02897724317147,-20.9601356719232,
-11.4446336096401));
#53820=CARTESIAN_POINT('Ctrl Pts',(-7.02876731759399,-19.0974432641274,
-11.0353407112804));
#53821=CARTESIAN_POINT('Ctrl Pts',(-7.02790277820779,-17.3268270760829,
-10.3242162170371));
#53822=CARTESIAN_POINT('Ctrl Pts',(-7.02622942251418,-15.6982394083911,
-9.33267672447058));
#53823=CARTESIAN_POINT('Ctrl Pts',(-7.02397939018392,-14.4407075914223,
-8.24600021840375));
#53824=CARTESIAN_POINT('Ctrl Pts',(-7.02249270527262,-13.7610270857261,
-7.4788788442118));
#53825=CARTESIAN_POINT('Ctrl Pts',(-7.02184974022686,-13.5171506741341,
-7.17356208348521));
#53826=CARTESIAN_POINT('Ctrl Pts',(-6.99838062461256,-24.2298260420536,
-10.8539091165241));
#53827=CARTESIAN_POINT('Ctrl Pts',(-6.99835912903231,-23.7718326954283,
-10.9268138766316));
#53828=CARTESIAN_POINT('Ctrl Pts',(-6.9982153209083,-22.7049180611933,-11.0282120131631));
#53829=CARTESIAN_POINT('Ctrl Pts',(-6.99814245032493,-21.0278292767672,
-10.9423805653543));
#53830=CARTESIAN_POINT('Ctrl Pts',(-6.99816421389256,-19.2468670671633,
-10.5510771500295));
#53831=CARTESIAN_POINT('Ctrl Pts',(-6.99828068869748,-17.5546312925736,
-9.87141112190437));
#53832=CARTESIAN_POINT('Ctrl Pts',(-6.99850456716759,-15.9978548244506,
-8.92372022371394));
#53833=CARTESIAN_POINT('Ctrl Pts',(-6.99873523316308,-14.7957513523325,
-7.88504846905375));
#53834=CARTESIAN_POINT('Ctrl Pts',(-6.99894167868191,-14.1458853061617,
-7.15167096124464));
#53835=CARTESIAN_POINT('Ctrl Pts',(-6.99898903069594,-13.9127708169516,
-6.85988336420863));
#53836=CARTESIAN_POINT('',(-7.0000030891977,-24.125943062142,-10.9277695894192));
#53837=CARTESIAN_POINT('Origin',(-5.99998370364475,-24.1259473086388,-10.9277595202031));
#53838=CARTESIAN_POINT('Ctrl Pts',(-7.00001101651448,-24.1259401091717,
-10.9277661762291));
#53839=CARTESIAN_POINT('Ctrl Pts',(-7.00001786894841,-23.9375949534064,
-10.9560764261617));
#53840=CARTESIAN_POINT('Ctrl Pts',(-7.00001802524214,-23.7511662537831,
-10.9791079086878));
#53841=CARTESIAN_POINT('Ctrl Pts',(-7.0000155683377,-23.5669990799827,-10.9972403661653));
#53842=CARTESIAN_POINT('Ctrl Pts',(-7.0000130640501,-23.3792801108786,-11.0157225210181));
#53843=CARTESIAN_POINT('Ctrl Pts',(-7.00000784335894,-23.1939106487979,
-11.0291149206812));
#53844=CARTESIAN_POINT('Ctrl Pts',(-7.00000354816807,-23.0112023806734,
-11.0378133705975));
#53845=CARTESIAN_POINT('Ctrl Pts',(-7.00000225617042,-22.9562435535322,
-11.0404298729061));
#53846=CARTESIAN_POINT('Ctrl Pts',(-7.00000104339694,-22.9015251573104,
-11.0426216150342));
#53847=CARTESIAN_POINT('Ctrl Pts',(-6.99999999753982,-22.847054769903,-11.0443992490626));
#53848=CARTESIAN_POINT('Ctrl Pts',(-6.99999887667118,-22.7886776292046,
-11.0463043794779));
#53849=CARTESIAN_POINT('Ctrl Pts',(-6.99999794691794,-22.7305853442371,
-11.0477338778685));
#53850=CARTESIAN_POINT('Ctrl Pts',(-6.9999971808834,-22.6727849338843,-11.0487021572659));
#53851=CARTESIAN_POINT('Ctrl Pts',(-6.99999462212509,-22.4797162504666,
-11.0519364669757));
#53852=CARTESIAN_POINT('Ctrl Pts',(-6.99999387748843,-22.2899078168075,
-11.050026312357));
#53853=CARTESIAN_POINT('Ctrl Pts',(-6.99999403435033,-22.1035889084951,
-11.0434957480642));
#53854=CARTESIAN_POINT('Ctrl Pts',(-6.99999406717179,-22.0646039374335,
-11.0421293067177));
#53855=CARTESIAN_POINT('Ctrl Pts',(-6.99999414003531,-22.0257715713113,
-11.0405605114676));
#53856=CARTESIAN_POINT('Ctrl Pts',(-6.99999424548476,-21.9870936476159,
-11.0387940517674));
#53857=CARTESIAN_POINT('Ctrl Pts',(-6.99999432422052,-21.9582140730811,
-11.0374750925343));
#53858=CARTESIAN_POINT('Ctrl Pts',(-6.99999441863043,-21.9301065451492,
-11.0360814515155));
#53859=CARTESIAN_POINT('Ctrl Pts',(-6.99999453138995,-21.901184306029,-11.0345337140022));
#53860=CARTESIAN_POINT('Ctrl Pts',(-6.99999463682153,-21.8741416446345,
-11.033086559744));
#53861=CARTESIAN_POINT('Ctrl Pts',(-6.99999475847225,-21.8463866802539,
-11.0315045683461));
#53862=CARTESIAN_POINT('Ctrl Pts',(-6.99999490350815,-21.8166248342906,
-11.0296819413284));
#53863=CARTESIAN_POINT('Ctrl Pts',(-6.99999520366054,-21.7550325699726,
-11.0259100071154));
#53864=CARTESIAN_POINT('Ctrl Pts',(-6.99999556265647,-21.6935868982399,
-11.0216269195953));
#53865=CARTESIAN_POINT('Ctrl Pts',(-6.99999595370132,-21.6322955714664,
-11.0168388713854));
#53866=CARTESIAN_POINT('Ctrl Pts',(-6.99999673579101,-21.5097129179193,
-11.0072627749656));
#53867=CARTESIAN_POINT('Ctrl Pts',(-6.99999764537228,-21.3877476442089,
-10.995666835787));
#53868=CARTESIAN_POINT('Ctrl Pts',(-6.99999847632133,-21.2664591437397,
-10.9821001893882));
#53869=CARTESIAN_POINT('Ctrl Pts',(-6.99999902465859,-21.1864217398015,
-10.9731476575841));
#53870=CARTESIAN_POINT('Ctrl Pts',(-6.99999953897947,-21.1066789849853,
-10.9633369557869));
#53871=CARTESIAN_POINT('Ctrl Pts',(-6.99999996276647,-21.0272472797666,
-10.9526820994163));
#53872=CARTESIAN_POINT('Ctrl Pts',(-7.00000126736821,-20.7827217472362,
-10.9198817910146));
#53873=CARTESIAN_POINT('Ctrl Pts',(-7.00000171385074,-20.5411477461523,
-10.8790828146912));
#53874=CARTESIAN_POINT('Ctrl Pts',(-7.00000170643174,-20.303018854281,-10.8307712657362));
#53875=CARTESIAN_POINT('Ctrl Pts',(-7.00000169893342,-20.0623438256886,
-10.7819431569977));
#53876=CARTESIAN_POINT('Ctrl Pts',(-7.00000122940917,-19.8251879290421,
-10.7254409706034));
#53877=CARTESIAN_POINT('Ctrl Pts',(-7.00000072342062,-19.5920096956152,
-10.6617510391509));
#53878=CARTESIAN_POINT('Ctrl Pts',(-7.00000046988425,-19.4751707606954,
-10.6298378384775));
#53879=CARTESIAN_POINT('Ctrl Pts',(-7.00000020716486,-19.3593297160924,
-10.5961197500517));
#53880=CARTESIAN_POINT('Ctrl Pts',(-6.9999999876648,-19.2445395631775,-10.5606565087878));
#53881=CARTESIAN_POINT('Ctrl Pts',(-6.99999993928972,-19.2192412461647,
-10.552840853028));
#53882=CARTESIAN_POINT('Ctrl Pts',(-6.9999998930078,-19.1939939597544,-10.5449404304622));
#53883=CARTESIAN_POINT('Ctrl Pts',(-6.99999984878645,-19.1687981731766,
-10.5369559936987));
#53884=CARTESIAN_POINT('Ctrl Pts',(-6.99999965374685,-19.0576713989215,
-10.501740395288));
#53885=CARTESIAN_POINT('Ctrl Pts',(-6.99999949863733,-18.9475466272878,
-10.4648905924172));
#53886=CARTESIAN_POINT('Ctrl Pts',(-6.99999938184507,-18.8384626319797,
-10.4264703291383));
#53887=CARTESIAN_POINT('Ctrl Pts',(-6.99999932344894,-18.7839206343257,
-10.4072601974988));
#53888=CARTESIAN_POINT('Ctrl Pts',(-6.99999927466345,-18.7296388307531,
-10.3876574507573));
#53889=CARTESIAN_POINT('Ctrl Pts',(-6.99999923547097,-18.6756218024774,
-10.3676699084702));
#53890=CARTESIAN_POINT('Ctrl Pts',(-6.99999921587473,-18.6486132883395,
-10.3576761373267));
#53891=CARTESIAN_POINT('Ctrl Pts',(-6.99999919867877,-18.6216709680258,
-10.3475861672968));
#53892=CARTESIAN_POINT('Ctrl Pts',(-6.99999918389284,-18.5947954063783,
-10.3374009714111));
#53893=CARTESIAN_POINT('Ctrl Pts',(-6.99999917282753,-18.574682595247,-10.3297786964287));
#53894=CARTESIAN_POINT('Ctrl Pts',(-6.99999916268429,-18.5536617939582,
-10.3217399904519));
#53895=CARTESIAN_POINT('Ctrl Pts',(-6.99999915445564,-18.5338561124317,
-10.3140994170821));
#53896=CARTESIAN_POINT('Ctrl Pts',(-6.99999915168883,-18.5271966314625,
-10.3115303435119));
#53897=CARTESIAN_POINT('Ctrl Pts',(-6.99999914912845,-18.5206743677,-10.3090067028305));
#53898=CARTESIAN_POINT('Ctrl Pts',(-6.999999146783,-18.514369557807,-10.3065606767057));
#53899=CARTESIAN_POINT('Ctrl Pts',(-6.99999907528804,-18.3221834138003,
-10.2319997720873));
#53900=CARTESIAN_POINT('Ctrl Pts',(-6.99999912491154,-18.129618500928,-10.1510712869352));
#53901=CARTESIAN_POINT('Ctrl Pts',(-6.99999933315392,-17.9371558589848,
-10.0634928398734));
#53902=CARTESIAN_POINT('Ctrl Pts',(-6.99999947285248,-17.8080430745273,
-10.0047411930891));
#53903=CARTESIAN_POINT('Ctrl Pts',(-6.99999968442919,-17.6789773237612,
-9.94299703195445));
#53904=CARTESIAN_POINT('Ctrl Pts',(-6.99999998816754,-17.5501167549105,
-9.87817779024853));
#53905=CARTESIAN_POINT('Ctrl Pts',(-7.0000004290411,-17.3630767616226,-9.78409322549982));
#53906=CARTESIAN_POINT('Ctrl Pts',(-7.00000106781896,-17.1764668647133,
-9.68352906351492));
#53907=CARTESIAN_POINT('Ctrl Pts',(-7.00000153332838,-16.9908087713364,
-9.57627873816244));
#53908=CARTESIAN_POINT('Ctrl Pts',(-7.00000199136873,-16.8081295564687,
-9.47074924104577));
#53909=CARTESIAN_POINT('Ctrl Pts',(-7.00000228134209,-16.6263718162228,
-9.35874636734403));
#53910=CARTESIAN_POINT('Ctrl Pts',(-7.00000202664203,-16.4460799745243,
-9.24008933015733));
#53911=CARTESIAN_POINT('Ctrl Pts',(-7.00000181210222,-16.2942159408053,
-9.14014173337999));
#53912=CARTESIAN_POINT('Ctrl Pts',(-7.00000121063474,-16.1433927337385,
-9.03547319345289));
#53913=CARTESIAN_POINT('Ctrl Pts',(-6.9999999866241,-15.9939628611808,-8.92598513115652));
#53914=CARTESIAN_POINT('Ctrl Pts',(-6.99999852879712,-15.8159881827653,
-8.79558213780594));
#53915=CARTESIAN_POINT('Ctrl Pts',(-6.99999617282013,-15.6399894215366,
-8.65834119823577));
#53916=CARTESIAN_POINT('Ctrl Pts',(-6.99999449839202,-15.4665325624122,
-8.51418171570541));
#53917=CARTESIAN_POINT('Ctrl Pts',(-6.99999284818661,-15.2955849730465,
-8.37210767984897));
#53918=CARTESIAN_POINT('Ctrl Pts',(-6.99999186150246,-15.1271062546936,
-8.22331377023279));
#53919=CARTESIAN_POINT('Ctrl Pts',(-6.99999320063255,-14.9616802774441,
-8.06775049235327));
#53920=CARTESIAN_POINT('Ctrl Pts',(-6.99999413393081,-14.8463876882616,
-7.9593316491543));
#53921=CARTESIAN_POINT('Ctrl Pts',(-6.99999620010739,-14.7325787767775,
-7.84762528725475));
#53922=CARTESIAN_POINT('Ctrl Pts',(-6.99999999965516,-14.6204636757736,
-7.73262300683288));
#53923=CARTESIAN_POINT('Ctrl Pts',(-7.00000506889282,-14.4708832189494,
-7.57919056564272));
#53924=CARTESIAN_POINT('Ctrl Pts',(-7.000013298643,-14.3243160482873,-7.4198896663707));
#53925=CARTESIAN_POINT('Ctrl Pts',(-7.0000165774608,-14.1813332730425,-7.25480434059693));
#53926=CARTESIAN_POINT('Ctrl Pts',(-7.00001838122332,-14.1026747488295,
-7.16398663145419));
#53927=CARTESIAN_POINT('Ctrl Pts',(-7.00001867169897,-14.0251016864707,
-7.07141891103329));
#53928=CARTESIAN_POINT('Ctrl Pts',(-7.00001598753963,-13.9487143147424,
-6.9771195452243));
#53929=CARTESIAN_POINT('Origin',(-5.9999949808,-24.1259380084106,-10.9277770011797));
#53930=CARTESIAN_POINT('Origin',(-6.,-24.1259427055448,-10.9277790621884));
#53931=CARTESIAN_POINT('Ctrl Pts',(-7.11139092859113,-15.2184460959384,
-5.12052280876705));
#53932=CARTESIAN_POINT('Ctrl Pts',(-7.11195855208738,-15.223719151167,-5.10426519075832));
#53933=CARTESIAN_POINT('Ctrl Pts',(-7.1136372886512,-15.2578366320999,-5.00059119811903));
#53934=CARTESIAN_POINT('Ctrl Pts',(-7.09280491237501,-15.3302302392258,
-4.7990182300767));
#53935=CARTESIAN_POINT('Ctrl Pts',(-7.00309038524378,-15.4434708112035,
-4.52630930653596));
#53936=CARTESIAN_POINT('Ctrl Pts',(-6.84623752314838,-15.5669468302129,
-4.27377175622976));
#53937=CARTESIAN_POINT('Ctrl Pts',(-6.63334306727782,-15.6888399309992,
-4.07033663875181));
#53938=CARTESIAN_POINT('Ctrl Pts',(-6.41901059637953,-15.7837928943819,
-3.95186938726383));
#53939=CARTESIAN_POINT('Ctrl Pts',(-6.28055126152101,-15.8346590679381,
-3.90855896005759));
#53940=CARTESIAN_POINT('Ctrl Pts',(-6.2306744828422,-15.8517787323193,-3.89680690069701));
#53941=CARTESIAN_POINT('Ctrl Pts',(-6.81161777639602,-14.6714606846117,
-4.93192660160615));
#53942=CARTESIAN_POINT('Ctrl Pts',(-6.81212328893671,-14.6760579235687,
-4.91772778087989));
#53943=CARTESIAN_POINT('Ctrl Pts',(-6.81362107184503,-14.7058456581685,
-4.82713697317831));
#53944=CARTESIAN_POINT('Ctrl Pts',(-6.79504003367809,-14.7695536197022,
-4.65054863615196));
#53945=CARTESIAN_POINT('Ctrl Pts',(-6.71482257063571,-14.8700027075903,
-4.41160379131102));
#53946=CARTESIAN_POINT('Ctrl Pts',(-6.57482808057142,-14.9798985601858,
-4.1910730559742));
#53947=CARTESIAN_POINT('Ctrl Pts',(-6.38564964768888,-15.0883124121041,
-4.01451732905237));
#53948=CARTESIAN_POINT('Ctrl Pts',(-6.19637626652847,-15.1724027362906,
-3.91259797704156));
#53949=CARTESIAN_POINT('Ctrl Pts',(-6.074854837314,-15.2171825715151,-3.87564777537514));
#53950=CARTESIAN_POINT('Ctrl Pts',(-6.03118272070632,-15.2322159785286,
-3.86565437501437));
#53951=CARTESIAN_POINT('Ctrl Pts',(-7.05013766657753,-14.0913326111332,
-4.75158252095379));
#53952=CARTESIAN_POINT('Ctrl Pts',(-7.05080210660599,-14.0972996850573,
-4.73318902546363));
#53953=CARTESIAN_POINT('Ctrl Pts',(-7.05275988231677,-14.1358643779999,
-4.61601626193555));
#53954=CARTESIAN_POINT('Ctrl Pts',(-7.02844934901559,-14.2172150025108,
-4.38943660681483));
#53955=CARTESIAN_POINT('Ctrl Pts',(-6.92428438305125,-14.3441879473141,
-4.08336733342954));
#53956=CARTESIAN_POINT('Ctrl Pts',(-6.74149011609023,-14.4833416388626,
-3.79856184173989));
#53957=CARTESIAN_POINT('Ctrl Pts',(-6.49116329395665,-14.6222984391297,
-3.56690077099674));
#53958=CARTESIAN_POINT('Ctrl Pts',(-6.23599489810763,-14.7324402085332,
-3.43022373396813));
#53959=CARTESIAN_POINT('Ctrl Pts',(-6.06915862423839,-14.7925192353585,
-3.37975541404639));
#53960=CARTESIAN_POINT('Ctrl Pts',(-6.00878489668786,-14.8128876803479,
-3.366032318725));
#53961=CARTESIAN_POINT('Ctrl Pts',(-7.66625772563486,-13.8781838194697,
-4.7040112511534));
#53962=CARTESIAN_POINT('Ctrl Pts',(-7.66719405941554,-13.8866359010153,
-4.67801897499989));
#53963=CARTESIAN_POINT('Ctrl Pts',(-7.66993998357738,-13.9411223884602,
-4.5126554880603));
#53964=CARTESIAN_POINT('Ctrl Pts',(-7.63581514365367,-14.0544598371705,
-4.19506349567618));
#53965=CARTESIAN_POINT('Ctrl Pts',(-7.49054162946217,-14.2292531573274,
-3.76657173189326));
#53966=CARTESIAN_POINT('Ctrl Pts',(-7.23439272786235,-14.4206227014939,
-3.36486723673259));
#53967=CARTESIAN_POINT('Ctrl Pts',(-6.87963590267719,-14.6133863806732,
-3.03354935884729));
#53968=CARTESIAN_POINT('Ctrl Pts',(-6.5124326609995,-14.7687834107463,-2.83442303682432));
#53969=CARTESIAN_POINT('Ctrl Pts',(-6.26884892595884,-14.8551443456087,
-2.75974286449289));
#53970=CARTESIAN_POINT('Ctrl Pts',(-6.18022691312438,-14.8846412572503,
-2.73933575737199));
#53971=CARTESIAN_POINT('',(-6.26386060036066,-15.8144217559011,-3.90573753028149));
#53972=CARTESIAN_POINT('',(-6.24994602117306,-14.8593867195859,-2.765467751532));
#53973=CARTESIAN_POINT('Ctrl Pts',(-6.26385652429609,-15.8144219194311,
-3.90575243311533));
#53974=CARTESIAN_POINT('Ctrl Pts',(-6.25434889993882,-15.7850152629862,
-3.90347479234289));
#53975=CARTESIAN_POINT('Ctrl Pts',(-6.24501694829635,-15.7549827955045,
-3.89975684459112));
#53976=CARTESIAN_POINT('Ctrl Pts',(-6.23596391386494,-15.7244969352914,
-3.89444911839014));
#53977=CARTESIAN_POINT('Ctrl Pts',(-6.22713722592631,-15.6947732910614,
-3.88927409744056));
#53978=CARTESIAN_POINT('Ctrl Pts',(-6.21857597188545,-15.6646189504095,
-3.88258712079457));
#53979=CARTESIAN_POINT('Ctrl Pts',(-6.21038173197456,-15.6342338906057,
-3.87427759589834));
#53980=CARTESIAN_POINT('Ctrl Pts',(-6.20231383173428,-15.6043173109158,
-3.86609618814901));
#53981=CARTESIAN_POINT('Ctrl Pts',(-6.1946020366201,-15.5741775227862,-3.85634126058895));
#53982=CARTESIAN_POINT('Ctrl Pts',(-6.18734459441452,-15.5440393360241,
-3.84494433544094));
#53983=CARTESIAN_POINT('Ctrl Pts',(-6.18021471889425,-15.5144308990662,
-3.83374773816641));
#53984=CARTESIAN_POINT('Ctrl Pts',(-6.1735236967773,-15.4848246440614,-3.82096592640214));
#53985=CARTESIAN_POINT('Ctrl Pts',(-6.16736111007851,-15.4554586832164,
-3.80657778903749));
#53986=CARTESIAN_POINT('Ctrl Pts',(-6.16656426144443,-15.4516615397551,
-3.8047173417665));
#53987=CARTESIAN_POINT('Ctrl Pts',(-6.16577623898295,-15.447868440501,-3.80283010325966));
#53988=CARTESIAN_POINT('Ctrl Pts',(-6.16499722734954,-15.4440799220539,
-3.80091608773727));
#53989=CARTESIAN_POINT('Ctrl Pts',(-6.15906489963985,-15.4152296045508,
-3.78634048086142));
#53990=CARTESIAN_POINT('Ctrl Pts',(-6.15365615351787,-15.3866443021748,
-3.77020801988018));
#53991=CARTESIAN_POINT('Ctrl Pts',(-6.14884557554313,-15.3585670169028,
-3.75255266407344));
#53992=CARTESIAN_POINT('Ctrl Pts',(-6.14409662647095,-15.3308494331651,
-3.73512349318845));
#53993=CARTESIAN_POINT('Ctrl Pts',(-6.13993089002222,-15.3036277392733,
-3.71621021877419));
#53994=CARTESIAN_POINT('Ctrl Pts',(-6.13640685600528,-15.2771366455292,
-3.69589448367759));
#53995=CARTESIAN_POINT('Ctrl Pts',(-6.1329035160769,-15.2508011147102,-3.67569804811645));
#53996=CARTESIAN_POINT('Ctrl Pts',(-6.13003458396478,-15.2251884341616,
-3.65411578637488));
#53997=CARTESIAN_POINT('Ctrl Pts',(-6.12784062593483,-15.2005180877307,
-3.63127496816577));
#53998=CARTESIAN_POINT('Ctrl Pts',(-6.12565411250769,-15.1759314534436,
-3.6085116540916));
#53999=CARTESIAN_POINT('Ctrl Pts',(-6.12413813899947,-15.1522815144872,
-3.58449873898918));
#54000=CARTESIAN_POINT('Ctrl Pts',(-6.1233133216665,-15.1297627974945,-3.55940429861102));
#54001=CARTESIAN_POINT('Ctrl Pts',(-6.1224892469612,-15.107264355321,-3.53433245211507));
#54002=CARTESIAN_POINT('Ctrl Pts',(-6.1223551290373,-15.0858957220768,-3.50818164249182));
#54003=CARTESIAN_POINT('Ctrl Pts',(-6.12291059718962,-15.0658178438706,
-3.48115374423421));
#54004=CARTESIAN_POINT('Ctrl Pts',(-6.12346877188963,-15.0456421351504,
-3.45399415112549));
#54005=CARTESIAN_POINT('Ctrl Pts',(-6.12472322579646,-15.0267702666732,
-3.4259496505214));
#54006=CARTESIAN_POINT('Ctrl Pts',(-6.12665239297863,-15.0093237705288,
-3.39724939775243));
#54007=CARTESIAN_POINT('Ctrl Pts',(-6.12858902383243,-14.9918097763886,
-3.36843810781452));
#54008=CARTESIAN_POINT('Ctrl Pts',(-6.13120544722315,-14.975732443847,-3.3389668257281));
#54009=CARTESIAN_POINT('Ctrl Pts',(-6.13446002689163,-14.9611673003063,
-3.30907972141196));
#54010=CARTESIAN_POINT('Ctrl Pts',(-6.13775200151227,-14.9464348040192,
-3.27884921581207));
#54011=CARTESIAN_POINT('Ctrl Pts',(-6.1416966582409,-14.9332494960981,-3.24819414394665));
#54012=CARTESIAN_POINT('Ctrl Pts',(-6.14623348971912,-14.9216388079144,
-3.21736676232502));
#54013=CARTESIAN_POINT('Ctrl Pts',(-6.14953766811315,-14.9131827334006,
-3.19491515291709));
#54014=CARTESIAN_POINT('Ctrl Pts',(-6.15315556109662,-14.9055607658247,
-3.17237216667401));
#54015=CARTESIAN_POINT('Ctrl Pts',(-6.15705925816722,-14.8987671910623,
-3.14983127721761));
#54016=CARTESIAN_POINT('Ctrl Pts',(-6.16251488973931,-14.8892727963152,
-3.11832914322578));
#54017=CARTESIAN_POINT('Ctrl Pts',(-6.16852868281514,-14.8813980812299,
-3.08683240633574));
#54018=CARTESIAN_POINT('Ctrl Pts',(-6.17501497441148,-14.8750872662013,
-3.0555762596843));
#54019=CARTESIAN_POINT('Ctrl Pts',(-6.18164965391719,-14.8686320776684,
-3.02360506126752));
#54020=CARTESIAN_POINT('Ctrl Pts',(-6.18877834589665,-14.8638126550383,
-2.99188622572886));
#54021=CARTESIAN_POINT('Ctrl Pts',(-6.19630368712461,-14.8605266126875,
-2.96063793694244));
#54022=CARTESIAN_POINT('Ctrl Pts',(-6.2039405004092,-14.8571918945508,-2.92892677067158));
#54023=CARTESIAN_POINT('Ctrl Pts',(-6.21198544673472,-14.8554356045965,
-2.89770057631721));
#54024=CARTESIAN_POINT('Ctrl Pts',(-6.22033644639755,-14.8551167953603,
-2.86714542587604));
#54025=CARTESIAN_POINT('Ctrl Pts',(-6.22888773877028,-14.8547903397142,
-2.83585743216696));
#54026=CARTESIAN_POINT('Ctrl Pts',(-6.23775961330328,-14.8559703733874,
-2.8052732725674));
#54027=CARTESIAN_POINT('Ctrl Pts',(-6.24684741590646,-14.8584816777926,
-2.77554433674993));
#54028=CARTESIAN_POINT('Ctrl Pts',(-6.24787754516983,-14.8587663415634,
-2.77217447407888));
#54029=CARTESIAN_POINT('Ctrl Pts',(-6.24891045694085,-14.8590680933294,
-2.76881554859793));
#54030=CARTESIAN_POINT('Ctrl Pts',(-6.24994600541046,-14.8593866659903,
-2.76546774155524));
#54031=CARTESIAN_POINT('',(-7.00000000902828,-14.5427410186974,-3.16613136210122));
#54032=CARTESIAN_POINT('Ctrl Pts',(-7.00000002511356,-14.542739937087,-3.16613069231016));
#54033=CARTESIAN_POINT('Ctrl Pts',(-6.96011600416233,-14.5636692275086,
-3.13137525098935));
#54034=CARTESIAN_POINT('Ctrl Pts',(-6.91914513183867,-14.584253870872,-3.09860123268627));
#54035=CARTESIAN_POINT('Ctrl Pts',(-6.8771519201577,-14.604510166625,-3.06774662680443));
#54036=CARTESIAN_POINT('Ctrl Pts',(-6.87107538686914,-14.6074413083624,
-3.0632818804266));
#54037=CARTESIAN_POINT('Ctrl Pts',(-6.86497736856078,-14.6103655792405,
-3.05885736617627));
#54038=CARTESIAN_POINT('Ctrl Pts',(-6.85885798311168,-14.6132830322912,
-3.05447294022931));
#54039=CARTESIAN_POINT('Ctrl Pts',(-6.81631977316428,-14.6335633743967,
-3.02399510336446));
#54040=CARTESIAN_POINT('Ctrl Pts',(-6.77275254603296,-14.6535142578584,
-2.99545177547727));
#54041=CARTESIAN_POINT('Ctrl Pts',(-6.72820659561677,-14.673148951286,-2.96879836373911));
#54042=CARTESIAN_POINT('Ctrl Pts',(-6.70154365414986,-14.6849012806603,
-2.95284498637419));
#54043=CARTESIAN_POINT('Ctrl Pts',(-6.6745292329114,-14.6965403430539,-2.93756929117119));
#54044=CARTESIAN_POINT('Ctrl Pts',(-6.64716751507883,-14.708068749641,-2.92296767350332));
#54045=CARTESIAN_POINT('Ctrl Pts',(-6.60219121491642,-14.7270187687235,
-2.89896601019018));
#54046=CARTESIAN_POINT('Ctrl Pts',(-6.55628914166064,-14.7456653224943,
-2.87678981055785));
#54047=CARTESIAN_POINT('Ctrl Pts',(-6.50944454425378,-14.7640218520635,
-2.85644737493458));
#54048=CARTESIAN_POINT('Ctrl Pts',(-6.48523668037748,-14.7735079485112,
-2.84593502260923));
#54049=CARTESIAN_POINT('Ctrl Pts',(-6.46077662967747,-14.7829165125535,
-2.8359130621748));
#54050=CARTESIAN_POINT('Ctrl Pts',(-6.43605934025051,-14.7922487267942,
-2.82638732690259));
#54051=CARTESIAN_POINT('Ctrl Pts',(-6.38889531125482,-14.8100558906559,
-2.80821089797369));
#54052=CARTESIAN_POINT('Ctrl Pts',(-6.34079553367693,-14.8275856751904,
-2.79183826000356));
#54053=CARTESIAN_POINT('Ctrl Pts',(-6.29174550793962,-14.8448349818748,
-2.77732265229406));
#54054=CARTESIAN_POINT('Ctrl Pts',(-6.27788844248412,-14.8497080633502,
-2.77322186492171));
#54055=CARTESIAN_POINT('Ctrl Pts',(-6.26395544574025,-14.8545586992195,
-2.76926958738593));
#54056=CARTESIAN_POINT('Ctrl Pts',(-6.24994600541046,-14.8593866659903,
-2.76546774155524));
#54057=CARTESIAN_POINT('',(-7.00001088476076,-14.7967989998614,-4.92966193866457));
#54058=CARTESIAN_POINT('Ctrl Pts',(-7.,-14.796798999896,-4.92966193873101));
#54059=CARTESIAN_POINT('Ctrl Pts',(-7.,-14.7449205055658,-4.79939605137961));
#54060=CARTESIAN_POINT('Ctrl Pts',(-7.,-14.7001933080234,-4.67547153146728));
#54061=CARTESIAN_POINT('Ctrl Pts',(-7.,-14.6626174072688,-4.55788837899402));
#54062=CARTESIAN_POINT('Ctrl Pts',(-7.,-14.6500921070173,-4.51869399483627));
#54063=CARTESIAN_POINT('Ctrl Pts',(-7.,-14.6389128416482,-4.48210949886636));
#54064=CARTESIAN_POINT('Ctrl Pts',(-7.,-14.6274252721102,-4.44241901566712));
#54065=CARTESIAN_POINT('Ctrl Pts',(-7.,-14.5814749939582,-4.28365708287018));
#54066=CARTESIAN_POINT('Ctrl Pts',(-7.,-14.5473536100588,-4.12819986609514));
#54067=CARTESIAN_POINT('Ctrl Pts',(-7.,-14.5258257394674,-3.98126610507176));
#54068=CARTESIAN_POINT('Ctrl Pts',(-7.,-14.4827699982847,-3.68739858302502));
#54069=CARTESIAN_POINT('Ctrl Pts',(-7.,-14.4884084168554,-3.41568714349165));
#54070=CARTESIAN_POINT('Ctrl Pts',(-7.,-14.5427409951797,-3.16613178647166));
#54071=CARTESIAN_POINT('Ctrl Pts',(-7.00001663766714,-14.7967989999222,
-4.92966193871151));
#54072=CARTESIAN_POINT('Ctrl Pts',(-7.00001663809637,-14.7975367734645,
-4.92865411678288));
#54073=CARTESIAN_POINT('Ctrl Pts',(-7.00001534769258,-14.7982733606461,
-4.9276484327044));
#54074=CARTESIAN_POINT('Ctrl Pts',(-7.000012781729,-14.7990087562765,-4.92664488855557));
#54075=CARTESIAN_POINT('Ctrl Pts',(-6.99994577229626,-14.8182134107743,
-4.90043760929783));
#54076=CARTESIAN_POINT('Ctrl Pts',(-6.99901241540824,-14.83660348244,-4.87569190868736));
#54077=CARTESIAN_POINT('Ctrl Pts',(-6.99748340315736,-14.8541002168799,
-4.85241809457354));
#54078=CARTESIAN_POINT('Ctrl Pts',(-6.99586198477726,-14.8726543695993,
-4.82773772333545));
#54079=CARTESIAN_POINT('Ctrl Pts',(-6.99357070413138,-14.8902040910381,
-4.80471221012978));
#54080=CARTESIAN_POINT('Ctrl Pts',(-6.99088477554742,-14.9066808349925,
-4.78332681937195));
#54081=CARTESIAN_POINT('Ctrl Pts',(-6.98885340324955,-14.9191422241106,
-4.76715301243458));
#54082=CARTESIAN_POINT('Ctrl Pts',(-6.98659528081006,-14.9309904422388,
-4.75191671818498));
#54083=CARTESIAN_POINT('Ctrl Pts',(-6.98421315519464,-14.9422037188569,
-4.73760410263847));
#54084=CARTESIAN_POINT('Ctrl Pts',(-6.98193649879244,-14.9529205248208,
-4.72392518175988));
#54085=CARTESIAN_POINT('Ctrl Pts',(-6.97954644605706,-14.9630574726601,
-4.71108984384714));
#54086=CARTESIAN_POINT('Ctrl Pts',(-6.97712173274568,-14.9726001913429,
-4.69908246542887));
#54087=CARTESIAN_POINT('Ctrl Pts',(-6.97495841148752,-14.9811141736312,
-4.68836952181397));
#54088=CARTESIAN_POINT('Ctrl Pts',(-6.97276741258127,-14.9891552339856,
-4.67831550295479));
#54089=CARTESIAN_POINT('Ctrl Pts',(-6.97059882000231,-14.9967157329114,
-4.66890728451756));
#54090=CARTESIAN_POINT('Ctrl Pts',(-6.96829921293241,-15.0047329957899,
-4.65893067303073));
#54091=CARTESIAN_POINT('Ctrl Pts',(-6.96602484765305,-15.0122098870659,
-4.64968020175899));
#54092=CARTESIAN_POINT('Ctrl Pts',(-6.96382697423633,-15.0191395327482,
-4.64114030304257));
#54093=CARTESIAN_POINT('Ctrl Pts',(-6.96272803752797,-15.0226043555894,
-4.63687035368436));
#54094=CARTESIAN_POINT('Ctrl Pts',(-6.96164809842778,-15.0259323699146,
-4.63277808260133));
#54095=CARTESIAN_POINT('Ctrl Pts',(-6.96059277771306,-15.0291229292358,
-4.62886157934885));
#54096=CARTESIAN_POINT('Ctrl Pts',(-6.9600651173557,-15.0307182088964,-4.6269033277226));
#54097=CARTESIAN_POINT('Ctrl Pts',(-6.95954360389157,-15.0322791249762,
-4.62498902010119));
#54098=CARTESIAN_POINT('Ctrl Pts',(-6.95902889420468,-15.033805600673,-4.62311842999734));
#54099=CARTESIAN_POINT('Ctrl Pts',(-6.95877153936123,-15.0345688385214,
-4.62218313494541));
#54100=CARTESIAN_POINT('Ctrl Pts',(-6.95851588499231,-15.0353234662854,
-4.62125876941255));
#54101=CARTESIAN_POINT('Ctrl Pts',(-6.95826201026872,-15.0360694750285,
-4.62034530544564));
#54102=CARTESIAN_POINT('Ctrl Pts',(-6.95813507290692,-15.0364424794,-4.61988857346219));
#54103=CARTESIAN_POINT('Ctrl Pts',(-6.95807521070884,-15.0366179364207,
-4.61967379541748));
#54104=CARTESIAN_POINT('Ctrl Pts',(-6.95798268246544,-15.0368889292216,
-4.61934206723523));
#54105=CARTESIAN_POINT('Ctrl Pts',(-6.95789015422205,-15.0371599220225,
-4.61901033905299));
#54106=CARTESIAN_POINT('Ctrl Pts',(-6.95776511469508,-15.0375264468331,
-4.61856161381191));
#54107=CARTESIAN_POINT('Ctrl Pts',(-6.95750580230632,-15.038281635463,-4.61763759073908));
#54108=CARTESIAN_POINT('Ctrl Pts',(-6.94614005914319,-15.0713817894802,
-4.57713737024271));
#54109=CARTESIAN_POINT('Ctrl Pts',(-6.9327462899655,-15.1039951502087,-4.53816352059833));
#54110=CARTESIAN_POINT('Ctrl Pts',(-6.91760941176288,-15.1359960352447,
-4.50084476430815));
#54111=CARTESIAN_POINT('Ctrl Pts',(-6.91219238734351,-15.1474481704446,
-4.48748952609994));
#54112=CARTESIAN_POINT('Ctrl Pts',(-6.90655172950781,-15.1588220949498,
-4.47434605023249));
#54113=CARTESIAN_POINT('Ctrl Pts',(-6.90069928966027,-15.1701127885821,
-4.46141953274621));
#54114=CARTESIAN_POINT('Ctrl Pts',(-6.89902619990268,-15.1733405609923,
-4.4577241126187));
#54115=CARTESIAN_POINT('Ctrl Pts',(-6.89733579847696,-15.1765615335403,
-4.45404642133306));
#54116=CARTESIAN_POINT('Ctrl Pts',(-6.89562842115357,-15.1797756007415,
-4.45038651876726));
#54117=CARTESIAN_POINT('Ctrl Pts',(-6.88344418924519,-15.2027119134196,
-4.42426862378707));
#54118=CARTESIAN_POINT('Ctrl Pts',(-6.87039641764602,-15.2252960975963,
-4.3990569651195));
#54119=CARTESIAN_POINT('Ctrl Pts',(-6.85660014356463,-15.2474931839915,
-4.37477093617939));
#54120=CARTESIAN_POINT('Ctrl Pts',(-6.84970200652394,-15.258591727189,-4.36262792170933));
#54121=CARTESIAN_POINT('Ctrl Pts',(-6.8426166363207,-15.2695934999198,-4.35071638136407));
#54122=CARTESIAN_POINT('Ctrl Pts',(-6.83535729734611,-15.2804947496512,
-4.33903818947538));
#54123=CARTESIAN_POINT('Ctrl Pts',(-6.83172762785882,-15.285945374517,-4.33319909353104));
#54124=CARTESIAN_POINT('Ctrl Pts',(-6.8280544601488,-15.2913708688442,-4.32741833799953));
#54125=CARTESIAN_POINT('Ctrl Pts',(-6.82433940590007,-15.2967707803477,
-4.32169615217796));
#54126=CARTESIAN_POINT('Ctrl Pts',(-6.82173742230159,-15.3005528196464,
-4.31768839545131));
#54127=CARTESIAN_POINT('Ctrl Pts',(-6.8193564466768,-15.3039769310697,-4.31407383849168));
#54128=CARTESIAN_POINT('Ctrl Pts',(-6.81669076362756,-15.3077687266043,
-4.31008576083222));
#54129=CARTESIAN_POINT('Ctrl Pts',(-6.81555044377055,-15.3093907723097,
-4.30837975000409));
#54130=CARTESIAN_POINT('Ctrl Pts',(-6.81435755445571,-15.3110800798102,
-4.30660574250561));
#54131=CARTESIAN_POINT('Ctrl Pts',(-6.8130701686411,-15.3128933243765,-4.30470553027457));
#54132=CARTESIAN_POINT('Ctrl Pts',(-6.79825969502292,-15.3337534352373,
-4.28284491724214));
#54133=CARTESIAN_POINT('Ctrl Pts',(-6.78272730742013,-15.354374326057,-4.26171751977155));
#54134=CARTESIAN_POINT('Ctrl Pts',(-6.76652828469596,-15.3747298948658,
-4.24136254811858));
#54135=CARTESIAN_POINT('Ctrl Pts',(-6.7355636332618,-15.4136398404618,-4.20245374399387));
#54136=CARTESIAN_POINT('Ctrl Pts',(-6.70216661465935,-15.4515790298085,
-4.16636672048905));
#54137=CARTESIAN_POINT('Ctrl Pts',(-6.66680173141148,-15.4883912322177,
-4.13326346432175));
#54138=CARTESIAN_POINT('Ctrl Pts',(-6.63958886664646,-15.5167177921796,
-4.10779089519013));
#54139=CARTESIAN_POINT('Ctrl Pts',(-6.61120949516485,-15.5443775351441,
-4.08408532659129));
#54140=CARTESIAN_POINT('Ctrl Pts',(-6.58185638319706,-15.5713077873573,
-4.06222104642336));
#54141=CARTESIAN_POINT('Ctrl Pts',(-6.54207699837613,-15.6078037087195,
-4.03259053857168));
#54142=CARTESIAN_POINT('Ctrl Pts',(-6.50051151132605,-15.6429592491191,
-4.0063409416901));
#54143=CARTESIAN_POINT('Ctrl Pts',(-6.45769611140315,-15.6766488500718,
-3.98352821426703));
#54144=CARTESIAN_POINT('Ctrl Pts',(-6.42609327516521,-15.7015157658018,
-3.96668971946865));
#54145=CARTESIAN_POINT('Ctrl Pts',(-6.39380826821476,-15.7255844436343,
-3.95172398635191));
#54146=CARTESIAN_POINT('Ctrl Pts',(-6.36104005522242,-15.7488112379618,
-3.93865360293187));
#54147=CARTESIAN_POINT('Ctrl Pts',(-6.32903948906336,-15.7714939081676,
-3.92588941376309));
#54148=CARTESIAN_POINT('Ctrl Pts',(-6.29657817025406,-15.7933737950221,
-3.91493248274305));
#54149=CARTESIAN_POINT('Ctrl Pts',(-6.26385652444153,-15.8144219193375,
-3.90575243315613));
#54150=CARTESIAN_POINT('Ctrl Pts',(-6.22266927200468,-14.5714076497178,
-3.97375074908438));
#54151=CARTESIAN_POINT('Ctrl Pts',(-6.22400481395816,-14.9771466562601,
-3.92718887782356));
#54152=CARTESIAN_POINT('Ctrl Pts',(-6.22726440271229,-16.0460349078152,
-3.85976027256915));
#54153=CARTESIAN_POINT('Ctrl Pts',(-6.23205292877977,-17.7794285729011,
-3.98191084033141));
#54154=CARTESIAN_POINT('Ctrl Pts',(-6.23570674183347,-19.7179592036766,
-4.44990468744485));
#54155=CARTESIAN_POINT('Ctrl Pts',(-6.23759590828025,-21.5545920913375,
-5.23225281484869));
#54156=CARTESIAN_POINT('Ctrl Pts',(-6.23804310410169,-23.2351578294011,
-6.30682863397947));
#54157=CARTESIAN_POINT('Ctrl Pts',(-6.2364962539807,-24.5993870470491,-7.54006269483624));
#54158=CARTESIAN_POINT('Ctrl Pts',(-6.23490846670046,-25.3447857086981,
-8.44425797847651));
#54159=CARTESIAN_POINT('Ctrl Pts',(-6.23413317444848,-25.6421043947626,
-8.85534264102317));
#54160=CARTESIAN_POINT('Ctrl Pts',(-6.71589077441495,-14.5843362145528,
-4.08566013088855));
#54161=CARTESIAN_POINT('Ctrl Pts',(-6.71707950162014,-14.9863211817523,
-4.04021329081558));
#54162=CARTESIAN_POINT('Ctrl Pts',(-6.7199340298597,-16.0451951223557,-3.97507849086041));
#54163=CARTESIAN_POINT('Ctrl Pts',(-6.72416488025816,-17.7615742587119,
-4.09849304259662));
#54164=CARTESIAN_POINT('Ctrl Pts',(-6.72736853924326,-19.6804278393728,
-4.5636779526249));
#54165=CARTESIAN_POINT('Ctrl Pts',(-6.72902459162388,-21.4982069937746,
-5.33903826408915));
#54166=CARTESIAN_POINT('Ctrl Pts',(-6.72941958809745,-23.1617854706901,
-6.40302993263691));
#54167=CARTESIAN_POINT('Ctrl Pts',(-6.72805205550861,-24.5127345552137,
-7.62318907122469));
#54168=CARTESIAN_POINT('Ctrl Pts',(-6.72668378134466,-25.2513986694556,
-8.51793692454479));
#54169=CARTESIAN_POINT('Ctrl Pts',(-6.72599063608826,-25.5460990905114,
-8.924725493994));
#54170=CARTESIAN_POINT('Ctrl Pts',(-7.02184867179209,-14.6305390362147,
-4.48559661493872));
#54171=CARTESIAN_POINT('Ctrl Pts',(-7.02249163003048,-15.0188785470189,
-4.44215144359658));
#54172=CARTESIAN_POINT('Ctrl Pts',(-7.02397829161063,-16.041923997109,-4.38032116097713));
#54173=CARTESIAN_POINT('Ctrl Pts',(-7.02622832902972,-17.6995302278369,
-4.50113419981309));
#54174=CARTESIAN_POINT('Ctrl Pts',(-7.02790167456001,-19.5522397357699,
-4.95159520695056));
#54175=CARTESIAN_POINT('Ctrl Pts',(-7.02876621306822,-21.3070950890534,
-5.70076885107868));
#54176=CARTESIAN_POINT('Ctrl Pts',(-7.02897613242694,-22.9136310478051,
-6.72847731338896));
#54177=CARTESIAN_POINT('Ctrl Pts',(-7.02824783070861,-24.2181462496305,
-7.9059965921817));
#54178=CARTESIAN_POINT('Ctrl Pts',(-7.02756288622409,-24.9320744273322,
-8.76993223223512));
#54179=CARTESIAN_POINT('Ctrl Pts',(-7.02718420231269,-25.2168998853482,
-9.16263757723443));
#54180=CARTESIAN_POINT('Ctrl Pts',(-6.99898915412836,-14.6884801947993,
-4.9871430090862));
#54181=CARTESIAN_POINT('Ctrl Pts',(-6.99894179669343,-15.0596433779913,
-4.94565457308912));
#54182=CARTESIAN_POINT('Ctrl Pts',(-6.99873531344683,-16.0377464552832,
-4.88660278316425));
#54183=CARTESIAN_POINT('Ctrl Pts',(-6.998504682319,-17.6222149766872,-5.00216659369601));
#54184=CARTESIAN_POINT('Ctrl Pts',(-6.99828080313596,-19.3931412309868,
-5.43285519773799));
#54185=CARTESIAN_POINT('Ctrl Pts',(-6.99816433582362,-21.0703293317465,
-6.14885025581044));
#54186=CARTESIAN_POINT('Ctrl Pts',(-6.998142566822,-22.6063533391169,-7.13148755499935));
#54187=CARTESIAN_POINT('Ctrl Pts',(-6.99821545410715,-23.8529237850754,
-8.25667423059523));
#54188=CARTESIAN_POINT('Ctrl Pts',(-6.99835921778234,-24.5356449630949,
-9.08279282694947));
#54189=CARTESIAN_POINT('Ctrl Pts',(-6.99838071861337,-24.8079420244304,
-9.45819132371699));
#54190=CARTESIAN_POINT('',(-7.00000355772207,-24.7867164860314,-9.33251602987223));
#54191=CARTESIAN_POINT('Ctrl Pts',(-7.00001601661514,-14.7967989997676,
-4.92966193854915));
#54192=CARTESIAN_POINT('Ctrl Pts',(-7.00002088999496,-15.0161849076412,
-4.90663942338753));
#54193=CARTESIAN_POINT('Ctrl Pts',(-7.00001598309289,-15.2342923928345,
-4.89043249278858));
#54194=CARTESIAN_POINT('Ctrl Pts',(-7.00000988157662,-15.4506295864929,
-4.88069445257409));
#54195=CARTESIAN_POINT('Ctrl Pts',(-7.00000652467729,-15.5696528173402,
-4.87533683011053));
#54196=CARTESIAN_POINT('Ctrl Pts',(-7.00000279094495,-15.6881411279891,
-4.87193736278651));
#54197=CARTESIAN_POINT('Ctrl Pts',(-6.99999999965555,-15.8060192824143,
-4.87043886254274));
#54198=CARTESIAN_POINT('Ctrl Pts',(-6.99999455422801,-16.0359835948731,
-4.86751549154191));
#54199=CARTESIAN_POINT('Ctrl Pts',(-6.99999266081081,-16.2636228788866,
-4.87182624541992));
#54200=CARTESIAN_POINT('Ctrl Pts',(-6.99999257345303,-16.4885261114551,
-4.88291895400832));
#54201=CARTESIAN_POINT('Ctrl Pts',(-6.99999248483031,-16.7166859233864,
-4.89417228405802));
#54202=CARTESIAN_POINT('Ctrl Pts',(-6.99999425319372,-16.9420299260002,
-4.91240537065293));
#54203=CARTESIAN_POINT('Ctrl Pts',(-6.99999619757822,-17.1641819043159,
-4.93715669708171));
#54204=CARTESIAN_POINT('Ctrl Pts',(-6.99999754424684,-17.3180429828072,
-4.95429931182364));
#54205=CARTESIAN_POINT('Ctrl Pts',(-6.99999897835409,-17.4703740013657,
-4.97456885757716));
#54206=CARTESIAN_POINT('Ctrl Pts',(-6.99999998662334,-17.6210642719037,
-4.99781499900363));
#54207=CARTESIAN_POINT('Ctrl Pts',(-7.00000143709259,-17.8378432762666,
-5.03125627809693));
#54208=CARTESIAN_POINT('Ctrl Pts',(-7.00000201442373,-18.051224743139,-5.07085612413644));
#54209=CARTESIAN_POINT('Ctrl Pts',(-7.00000210876075,-18.260914284654,-5.11608683430385));
#54210=CARTESIAN_POINT('Ctrl Pts',(-7.00000220461189,-18.4739693834249,
-5.16204350602229));
#54211=CARTESIAN_POINT('Ctrl Pts',(-7.00000180217035,-18.6832131501843,
-5.21381323096648));
#54212=CARTESIAN_POINT('Ctrl Pts',(-7.00000129011946,-18.8883856688076,
-5.27086615566158));
#54213=CARTESIAN_POINT('Ctrl Pts',(-7.00000086167035,-19.0600599782347,
-5.31860413496579));
#54214=CARTESIAN_POINT('Ctrl Pts',(-7.00000035619256,-19.2288848433898,
-5.37004141745854));
#54215=CARTESIAN_POINT('Ctrl Pts',(-6.99999998816687,-19.3947330689617,
-5.42488007160696));
#54216=CARTESIAN_POINT('Ctrl Pts',(-6.9999997037335,-19.5229109953601,-5.46726282819648));
#54217=CARTESIAN_POINT('Ctrl Pts',(-6.99999950019772,-19.6493114378435,
-5.51167745875434));
#54218=CARTESIAN_POINT('Ctrl Pts',(-6.99999936067303,-19.7738903396788,
-5.55798426808907));
#54219=CARTESIAN_POINT('Ctrl Pts',(-6.99999924478735,-19.8773624232099,
-5.59644553217921));
#54220=CARTESIAN_POINT('Ctrl Pts',(-6.99999917321298,-19.9795780416209,
-5.63621220749404));
#54221=CARTESIAN_POINT('Ctrl Pts',(-6.99999913936349,-20.0805155867661,
-5.67720662381942));
#54222=CARTESIAN_POINT('Ctrl Pts',(-6.99999912243875,-20.1309843593387,
-5.69770383198211));
#54223=CARTESIAN_POINT('Ctrl Pts',(-6.99999911498657,-20.1811336135949,
-5.71850797539744));
#54224=CARTESIAN_POINT('Ctrl Pts',(-6.9999991163999,-20.2309610063002,-5.73960958184171));
#54225=CARTESIAN_POINT('Ctrl Pts',(-6.99999911710657,-20.2558747026529,
-5.75016038506384));
#54226=CARTESIAN_POINT('Ctrl Pts',(-6.99999912003181,-20.2807079336179,
-5.76078555404321));
#54227=CARTESIAN_POINT('Ctrl Pts',(-6.99999912511196,-20.3054604155709,
-5.77148391108337));
#54228=CARTESIAN_POINT('Ctrl Pts',(-6.99999912765204,-20.3178366565475,
-5.77683308960345));
#54229=CARTESIAN_POINT('Ctrl Pts',(-6.99999913073096,-20.330192710271,-5.78220056513874));
#54230=CARTESIAN_POINT('Ctrl Pts',(-6.99999913434146,-20.3425285425323,
-5.78758619130768));
#54231=CARTESIAN_POINT('Ctrl Pts',(-6.99999913749777,-20.3533125294659,
-5.79229430673962));
#54232=CARTESIAN_POINT('Ctrl Pts',(-6.99999914056829,-20.3627039949546,
-5.79641054026109));
#54233=CARTESIAN_POINT('Ctrl Pts',(-6.99999914483357,-20.3743145101157,
-5.80152322606212));
#54234=CARTESIAN_POINT('Ctrl Pts',(-6.99999914544735,-20.3759852951245,
-5.802258955586));
#54235=CARTESIAN_POINT('Ctrl Pts',(-6.99999914608783,-20.3777019974094,
-5.80301539887061));
#54236=CARTESIAN_POINT('Ctrl Pts',(-6.99999914676092,-20.3794753410883,
-5.80379737558169));
#54237=CARTESIAN_POINT('Ctrl Pts',(-6.99999923697264,-20.6171481358953,
-5.90860198430455));
#54238=CARTESIAN_POINT('Ctrl Pts',(-6.99999952144547,-20.8492773499208,
-6.02101208188487));
#54239=CARTESIAN_POINT('Ctrl Pts',(-6.99999999018442,-21.0754641488202,
-6.14041758832291));
#54240=CARTESIAN_POINT('Ctrl Pts',(-7.00000044364504,-21.2942784891113,
-6.25593112512301));
#54241=CARTESIAN_POINT('Ctrl Pts',(-7.00000106797113,-21.5075320214405,
-6.37799078394024));
#54242=CARTESIAN_POINT('Ctrl Pts',(-7.00000142593302,-21.7149314703275,
-6.50595747362906));
#54243=CARTESIAN_POINT('Ctrl Pts',(-7.00000178765839,-21.9245114365704,
-6.63526955545526));
#54244=CARTESIAN_POINT('Ctrl Pts',(-7.0000018762758,-22.1281136184752,-6.77061353997294));
#54245=CARTESIAN_POINT('Ctrl Pts',(-7.0000013155977,-22.325477297402,-6.91136295359017));
#54246=CARTESIAN_POINT('Ctrl Pts',(-7.0000010387387,-22.4229341272705,-6.98086404787235));
#54247=CARTESIAN_POINT('Ctrl Pts',(-7.00000060481352,-22.5188704490222,
-7.05168366000249));
#54248=CARTESIAN_POINT('Ctrl Pts',(-6.999999976358,-22.6132585283086,-7.12374926523835));
#54249=CARTESIAN_POINT('Ctrl Pts',(-6.99999887928019,-22.7780292468715,
-7.24955224426024));
#54250=CARTESIAN_POINT('Ctrl Pts',(-6.99999719586383,-22.9380810757636,
-7.3791511577127));
#54251=CARTESIAN_POINT('Ctrl Pts',(-6.99999590263445,-23.0933375024812,
-7.51215861203649));
#54252=CARTESIAN_POINT('Ctrl Pts',(-6.99999568171304,-23.1198598429666,
-7.53488017703224));
#54253=CARTESIAN_POINT('Ctrl Pts',(-6.99999546002068,-23.1476959266424,
-7.55895202597045));
#54254=CARTESIAN_POINT('Ctrl Pts',(-6.99999525388502,-23.175812124434,-7.58352663462908));
#54255=CARTESIAN_POINT('Ctrl Pts',(-6.9999951202971,-23.1940330588923,-7.59945241296604));
#54256=CARTESIAN_POINT('Ctrl Pts',(-6.9999949932363,-23.2123722665019,-7.61558857541806));
#54257=CARTESIAN_POINT('Ctrl Pts',(-6.99999487630671,-23.2305561250311,
-7.63169548141941));
#54258=CARTESIAN_POINT('Ctrl Pts',(-6.99999457894647,-23.2767989705564,
-7.67265648894783));
#54259=CARTESIAN_POINT('Ctrl Pts',(-6.99999434327551,-23.3225495659397,
-7.71387576700431));
#54260=CARTESIAN_POINT('Ctrl Pts',(-6.99999419420459,-23.3678081332012,
-7.75534001206123));
#54261=CARTESIAN_POINT('Ctrl Pts',(-6.99999365475073,-23.5315886342942,
-7.9053897207413));
#54262=CARTESIAN_POINT('Ctrl Pts',(-6.99999426200425,-23.6889263430828,
-8.05864816970276));
#54263=CARTESIAN_POINT('Ctrl Pts',(-6.99999708872154,-23.8398710235771,
-8.21453737949556));
#54264=CARTESIAN_POINT('Ctrl Pts',(-6.99999738650744,-23.8557725776303,
-8.23095982437877));
#54265=CARTESIAN_POINT('Ctrl Pts',(-6.99999770877207,-23.8716032104523,
-8.24741150351764));
#54266=CARTESIAN_POINT('Ctrl Pts',(-6.99999805666162,-23.8873630000909,
-8.26389176796206));
#54267=CARTESIAN_POINT('Ctrl Pts',(-6.99999863110494,-23.9133859316887,
-8.29110436433449));
#54268=CARTESIAN_POINT('Ctrl Pts',(-6.99999927542365,-23.9392157050888,
-8.31839489775144));
#54269=CARTESIAN_POINT('Ctrl Pts',(-6.99999999465528,-23.9648526940703,
-8.3457604773189));
#54270=CARTESIAN_POINT('Ctrl Pts',(-7.00000393348073,-24.105252005446,-8.49562630319423));
#54271=CARTESIAN_POINT('Ctrl Pts',(-7.00001006470838,-24.2398674196823,
-8.64773911793527));
#54272=CARTESIAN_POINT('Ctrl Pts',(-7.00001375740975,-24.368761885244,-8.80154981297568));
#54273=CARTESIAN_POINT('Ctrl Pts',(-7.00001750459986,-24.4995582908587,
-8.95763010679384));
#54274=CARTESIAN_POINT('Ctrl Pts',(-7.00001874206956,-24.6244637358377,
-9.11545880287537));
#54275=CARTESIAN_POINT('Ctrl Pts',(-7.00001328594145,-24.7435693586713,
-9.27450916479436));
#54276=CARTESIAN_POINT('Ctrl Pts',(-7.00001262322841,-24.7580361834604,
-9.29382776339437));
#54277=CARTESIAN_POINT('Ctrl Pts',(-7.00001186253236,-24.7724174727017,
-9.31316444096061));
#54278=CARTESIAN_POINT('Ctrl Pts',(-7.00001099698694,-24.786713413932,-9.33251829944506));
#54279=CARTESIAN_POINT('',(-6.271594443024,-25.5608538793679,-8.76071211955051));
#54280=CARTESIAN_POINT('Origin',(-5.99998362344702,-24.7867137519324,-9.33252812839853));
#54281=CARTESIAN_POINT('Ctrl Pts',(-6.26386060036066,-15.8144217559011,
-3.90573753028149));
#54282=CARTESIAN_POINT('Ctrl Pts',(-6.26455152101633,-16.0555043624403,
-3.90327937002865));
#54283=CARTESIAN_POINT('Ctrl Pts',(-6.26520985795224,-16.2942797838742,
-3.90810432648021));
#54284=CARTESIAN_POINT('Ctrl Pts',(-6.26583561154063,-16.5303211757527,
-3.9197834877742));
#54285=CARTESIAN_POINT('Ctrl Pts',(-6.26647066563248,-16.769870823628,-3.93163623509615));
#54286=CARTESIAN_POINT('Ctrl Pts',(-6.26707216061391,-17.006604611909,-3.95054842272576));
#54287=CARTESIAN_POINT('Ctrl Pts',(-6.26764009687402,-17.2401298953749,
-3.97608001918924));
#54288=CARTESIAN_POINT('Ctrl Pts',(-6.26812468476161,-17.4393838112797,
-3.99786468635311));
#54289=CARTESIAN_POINT('Ctrl Pts',(-6.26858484108239,-17.6363028076252,
-4.02446858056822));
#54290=CARTESIAN_POINT('Ctrl Pts',(-6.26902056607808,-17.8306725457858,
-4.05562321047439));
#54291=CARTESIAN_POINT('Ctrl Pts',(-6.26953467319349,-18.0600072555133,
-4.0923822145962));
#54292=CARTESIAN_POINT('Ctrl Pts',(-6.27001476853342,-18.2857921847647,
-4.13547499922886));
#54293=CARTESIAN_POINT('Ctrl Pts',(-6.27046085249489,-18.5077369937188,
-4.18435768233148));
#54294=CARTESIAN_POINT('Ctrl Pts',(-6.2706208341698,-18.5873343461017,-4.20188876211064));
#54295=CARTESIAN_POINT('Ctrl Pts',(-6.27077644131375,-18.666438221103,-4.22016475889813));
#54296=CARTESIAN_POINT('Ctrl Pts',(-6.27092767394504,-18.7450366707039,
-4.2391613241562));
#54297=CARTESIAN_POINT('Ctrl Pts',(-6.27136815415621,-18.9739625406082,
-4.29449072631342));
#54298=CARTESIAN_POINT('Ctrl Pts',(-6.2717715237205,-19.1985969459198,-4.35593088266701));
#54299=CARTESIAN_POINT('Ctrl Pts',(-6.2721377826379,-19.4186799866693,-4.42289859637978));
#54300=CARTESIAN_POINT('Ctrl Pts',(-6.27250404155531,-19.6387630274189,
-4.48986631009256));
#54301=CARTESIAN_POINT('Ctrl Pts',(-6.27283318982583,-19.8542949102162,
-4.56236164112509));
#54302=CARTESIAN_POINT('Ctrl Pts',(-6.27312522744947,-20.0650658262731,
-4.63982808853314));
#54303=CARTESIAN_POINT('Ctrl Pts',(-6.27334042054069,-20.2203761058236,
-4.69691061124459));
#54304=CARTESIAN_POINT('Ctrl Pts',(-6.27353526296335,-20.3728239547611,
-4.75658573046659));
#54305=CARTESIAN_POINT('Ctrl Pts',(-6.27370997638795,-20.5226551266523,
-4.81874475214896));
#54306=CARTESIAN_POINT('Ctrl Pts',(-6.27388468981255,-20.6724862985435,
-4.88090377383133));
#54307=CARTESIAN_POINT('Ctrl Pts',(-6.27403927423909,-20.8197011255933,
-4.9455469677457));
#54308=CARTESIAN_POINT('Ctrl Pts',(-6.2741739513381,-20.9645377629538,-5.01262254869206));
#54309=CARTESIAN_POINT('Ctrl Pts',(-6.27427013657007,-21.0679788503139,
-5.06052735478846));
#54310=CARTESIAN_POINT('Ctrl Pts',(-6.27435616768303,-21.1702067690755,
-5.10967398530267));
#54311=CARTESIAN_POINT('Ctrl Pts',(-6.27443212542871,-21.2713096271537,
-5.1600492269349));
#54312=CARTESIAN_POINT('Ctrl Pts',(-6.27457884449751,-21.466598692925,-5.25735343834247));
#54313=CARTESIAN_POINT('Ctrl Pts',(-6.27469165431798,-21.6616526261861,
-5.36122068036853));
#54314=CARTESIAN_POINT('Ctrl Pts',(-6.27477055489012,-21.8559696046935,
-5.47186403281939));
#54315=CARTESIAN_POINT('Ctrl Pts',(-6.27484862803197,-22.0482487810896,
-5.58134706845722));
#54316=CARTESIAN_POINT('Ctrl Pts',(-6.2748934994088,-22.2398064589334,-5.69746491395644));
#54317=CARTESIAN_POINT('Ctrl Pts',(-6.27490516902061,-22.430109432408,-5.82040617935769));
#54318=CARTESIAN_POINT('Ctrl Pts',(-6.27491664504186,-22.6172554148452,
-5.94130793656888));
#54319=CARTESIAN_POINT('Ctrl Pts',(-6.27489601174817,-22.8031880010741,
-6.06880865090116));
#54320=CARTESIAN_POINT('Ctrl Pts',(-6.27484326913954,-22.9873536900837,
-6.20306945318438));
#54321=CARTESIAN_POINT('Ctrl Pts',(-6.27479056659583,-23.1713794811427,
-6.33722826681168));
#54322=CARTESIAN_POINT('Ctrl Pts',(-6.2747058035011,-23.353641205317,-6.4781370005255));
#54323=CARTESIAN_POINT('Ctrl Pts',(-6.27458897985536,-23.5335384516302,
-6.62593686197285));
#54324=CARTESIAN_POINT('Ctrl Pts',(-6.27454781366932,-23.5969304427347,
-6.67801841238085));
#54325=CARTESIAN_POINT('Ctrl Pts',(-6.2745026665428,-23.6600283853014,-6.73095545421918));
#54326=CARTESIAN_POINT('Ctrl Pts',(-6.27445353846372,-23.7228045291254,
-6.78475355165375));
#54327=CARTESIAN_POINT('Ctrl Pts',(-6.27431624089265,-23.8982441601719,
-6.93510235917805));
#54328=CARTESIAN_POINT('Ctrl Pts',(-6.27414785100046,-24.0711731898611,
-7.09217873860768));
#54329=CARTESIAN_POINT('Ctrl Pts',(-6.273948368523,-24.241035364564,-7.25599605961389));
#54330=CARTESIAN_POINT('Ctrl Pts',(-6.2737507271022,-24.4093298532675,-7.4183014835715));
#54331=CARTESIAN_POINT('Ctrl Pts',(-6.27352256436492,-24.5746138826622,
-7.58722407975246));
#54332=CARTESIAN_POINT('Ctrl Pts',(-6.27326388005427,-24.736307790633,-7.76274419335866));
#54333=CARTESIAN_POINT('Ctrl Pts',(-6.27300884371265,-24.8957214893191,
-7.93578912037485));
#54334=CARTESIAN_POINT('Ctrl Pts',(-6.27272414055906,-25.0516456202578,
-8.11524684955891));
#54335=CARTESIAN_POINT('Ctrl Pts',(-6.27240977034733,-25.2034865494107,
-8.3010657208509));
#54336=CARTESIAN_POINT('Ctrl Pts',(-6.27215746715882,-25.3253490832686,
-8.45019783312509));
#54337=CARTESIAN_POINT('Ctrl Pts',(-6.2718860550044,-25.4445808669205,-8.60342664882594));
#54338=CARTESIAN_POINT('Ctrl Pts',(-6.27159553375681,-25.5608567073965,
-8.76070944735595));
#54339=CARTESIAN_POINT('Origin',(-5.999994993365,-24.786719601394,-9.33250915082771));
#54340=CARTESIAN_POINT('',(-5.98852246669785,-25.7188096068216,-9.69456809148799));
#54341=CARTESIAN_POINT('Origin',(-5.999994993365,-24.786719601394,-9.33250915082771));
#54342=CARTESIAN_POINT('Origin',(-6.,-24.7867243682986,-9.33251101023518));
#54343=CARTESIAN_POINT('Ctrl Pts',(-5.98841833130012,-25.7189877482677,
-9.69410640815296));
#54344=CARTESIAN_POINT('Ctrl Pts',(-5.98810627248473,-25.6713270177476,
-9.81679904172914));
#54345=CARTESIAN_POINT('Ctrl Pts',(-5.98726405054396,-25.5029619479273,
-10.2439466060386));
#54346=CARTESIAN_POINT('Ctrl Pts',(-5.98726405054303,-25.276881441752,-10.7897532301295));
#54347=CARTESIAN_POINT('Ctrl Pts',(-5.98810627250475,-25.0938945838116,
-11.2108442545143));
#54348=CARTESIAN_POINT('Ctrl Pts',(-5.988418331338,-25.0408390143962,-11.3313022777533));
#54349=CARTESIAN_POINT('Ctrl Pts',(-6.5801963721225,-25.7253769306717,-9.69658812258632));
#54350=CARTESIAN_POINT('Ctrl Pts',(-6.57988216475446,-25.6778801589542,
-9.81936871691908));
#54351=CARTESIAN_POINT('Ctrl Pts',(-6.57903377348696,-25.5099484810557,
-10.2467760959601));
#54352=CARTESIAN_POINT('Ctrl Pts',(-6.57903377348612,-25.283822418215,-10.7926927035727));
#54353=CARTESIAN_POINT('Ctrl Pts',(-6.57988216477348,-25.1003453891382,
-11.2136609903448));
#54354=CARTESIAN_POINT('Ctrl Pts',(-6.58019637215976,-25.0471116856881,
-11.3340652748482));
#54355=CARTESIAN_POINT('Ctrl Pts',(-7.00079676976986,-25.3372908820653,
-9.54584601778628));
#54356=CARTESIAN_POINT('Ctrl Pts',(-7.00061248512561,-25.2904141391689,
-9.66739289158177));
#54357=CARTESIAN_POINT('Ctrl Pts',(-7.00011448465087,-25.1245686184425,
-10.0904742413177));
#54358=CARTESIAN_POINT('Ctrl Pts',(-7.00011448465083,-24.900795602742,-10.6307100906301));
#54359=CARTESIAN_POINT('Ctrl Pts',(-7.00061248513681,-24.7189024024401,
-11.0471442768304));
#54360=CARTESIAN_POINT('Ctrl Pts',(-7.00079676979122,-24.6661026445716,
-11.1662377625412));
#54361=CARTESIAN_POINT('Ctrl Pts',(-6.99999917319453,-24.7856430606156,
-9.33157252365516));
#54362=CARTESIAN_POINT('Ctrl Pts',(-6.99999957777276,-24.7394735072572,
-9.45129807097163));
#54363=CARTESIAN_POINT('Ctrl Pts',(-7.00000004362276,-24.5761256640229,
-9.8680415723771));
#54364=CARTESIAN_POINT('Ctrl Pts',(-7.00000004362357,-24.355704222059,-10.4001860069027));
#54365=CARTESIAN_POINT('Ctrl Pts',(-6.999999577773,-24.1765264326202,-10.810372532843));
#54366=CARTESIAN_POINT('Ctrl Pts',(-6.99999917319377,-24.1245144885734,
-10.9276780876708));
#54367=CARTESIAN_POINT('Origin',(-5.98852353414726,11.4730434399881,4.75229019692621));
#54368=CARTESIAN_POINT('Origin',(-7.0002100696521,11.4504616060432,4.74293652827744));
#54369=CARTESIAN_POINT('Ctrl Pts',(-6.05508738338166,-25.8431978089075,
-9.37216207432707));
#54370=CARTESIAN_POINT('Ctrl Pts',(-4.03672492225411,-26.0304387093361,
-8.81555276746131));
#54371=CARTESIAN_POINT('Ctrl Pts',(7.59697247682684E-7,-26.2482635689839,
-8.27058109728118));
#54372=CARTESIAN_POINT('Ctrl Pts',(4.03672644164874,-26.0304386273479,-8.81555297258393));
#54373=CARTESIAN_POINT('Ctrl Pts',(6.05508966247359,-25.8431975974789,-9.37216270283815));
#54374=CARTESIAN_POINT('Ctrl Pts',(-6.05508738338166,-25.5527881519605,
-10.1400064040411));
#54375=CARTESIAN_POINT('Ctrl Pts',(-4.03672492225411,-25.6069167071504,
-9.95059902476454));
#54376=CARTESIAN_POINT('Ctrl Pts',(7.59697247682684E-7,-25.7964943223401,
-9.81341146699688));
#54377=CARTESIAN_POINT('Ctrl Pts',(4.03672644164874,-25.6069166358008,-9.95059907640347));
#54378=CARTESIAN_POINT('Ctrl Pts',(6.05508966247359,-25.5527880908442,-10.1400066179177));
#54379=CARTESIAN_POINT('Ctrl Pts',(-6.05508738338166,-25.2383576100257,
-10.8990909622833));
#54380=CARTESIAN_POINT('Ctrl Pts',(-4.03672492225411,-25.1425761077887,
-11.0715861668952));
#54381=CARTESIAN_POINT('Ctrl Pts',(7.59697247682684E-7,-25.1794674505639,
-11.3029246861743));
#54382=CARTESIAN_POINT('Ctrl Pts',(4.03672644164874,-25.1425760939039,-11.0715860798213));
#54383=CARTESIAN_POINT('Ctrl Pts',(6.05508966247359,-25.2383577181847,-10.8990907675073));
#54384=CARTESIAN_POINT('Ctrl Pts',(-6.05508738338166,-24.900747869581,-11.6473837381431));
#54385=CARTESIAN_POINT('Ctrl Pts',(-4.03672492225411,-24.6394316467689,
-12.1736501920162));
#54386=CARTESIAN_POINT('Ctrl Pts',(7.59697247682684E-7,-24.4078877465999,
-12.7132770985331));
#54387=CARTESIAN_POINT('Ctrl Pts',(4.03672644164874,-24.6394317339223,-12.1736499889053));
#54388=CARTESIAN_POINT('Ctrl Pts',(6.05508966247359,-24.9007481646544,-11.647383143894));
#54389=CARTESIAN_POINT('Ctrl Pts',(-5.98852262888631,-25.7188097476013,
-9.69456765092976));
#54390=CARTESIAN_POINT('Ctrl Pts',(-5.9390643825995,-25.724559801551,-9.67819736170012));
#54391=CARTESIAN_POINT('Ctrl Pts',(-5.88263516414606,-25.7310811669272,
-9.65968542650558));
#54392=CARTESIAN_POINT('Ctrl Pts',(-5.8191641443799,-25.7383219151964,-9.63921749653948));
#54393=CARTESIAN_POINT('Ctrl Pts',(-5.75804505445195,-25.7452943562608,
-9.61950800933027));
#54394=CARTESIAN_POINT('Ctrl Pts',(-5.69039610157012,-25.7529339130711,
-9.59798498846537));
#54395=CARTESIAN_POINT('Ctrl Pts',(-5.61614355003017,-25.761179079695,-9.57485600815482));
#54396=CARTESIAN_POINT('Ctrl Pts',(-5.54046210244506,-25.7695829140783,
-9.55128193999465));
#54397=CARTESIAN_POINT('Ctrl Pts',(-5.45792023964537,-25.7786161404993,
-9.52603926689531));
#54398=CARTESIAN_POINT('Ctrl Pts',(-5.36843221659716,-25.7881950956482,
-9.49939300492048));
#54399=CARTESIAN_POINT('Ctrl Pts',(-5.32368820507305,-25.7929845732227,
-9.48606987393307));
#54400=CARTESIAN_POINT('Ctrl Pts',(-5.27720755484741,-25.79791017272,-9.47239656836499));
#54401=CARTESIAN_POINT('Ctrl Pts',(-5.22897913301206,-25.8029594239223,
-9.4584106464505));
#54402=CARTESIAN_POINT('Ctrl Pts',(-5.20486492209439,-25.8054840495234,
-9.45141768549325));
#54403=CARTESIAN_POINT('Ctrl Pts',(-5.18031376829501,-25.8080395842763,
-9.44434656901355));
#54404=CARTESIAN_POINT('Ctrl Pts',(-5.15532426463177,-25.8106243048844,
-9.43720234551523));
#54405=CARTESIAN_POINT('Ctrl Pts',(-5.13033476096853,-25.8132090254925,
-9.4300581220169));
#54406=CARTESIAN_POINT('Ctrl Pts',(-5.10370559224123,-25.8159456101558,
-9.42250242119417));
#54407=CARTESIAN_POINT('Ctrl Pts',(-5.07903930494025,-25.818464270517,-9.41555542182804));
#54408=CARTESIAN_POINT('Ctrl Pts',(-5.06413128986708,-25.8199865193325,
-9.41135673679693));
#54409=CARTESIAN_POINT('Ctrl Pts',(-5.04933271582664,-25.8214915258363,
-9.40720810707613));
#54410=CARTESIAN_POINT('Ctrl Pts',(-5.0346439037231,-25.8229794943833,-9.40310875488214));
#54411=CARTESIAN_POINT('Ctrl Pts',(-4.91716822316177,-25.8348797158908,
-9.37032365385047));
#54412=CARTESIAN_POINT('Ctrl Pts',(-4.80671568615821,-25.8456906475692,
-9.34068705338644));
#54413=CARTESIAN_POINT('Ctrl Pts',(-4.70342528861786,-25.8555215872748,
-9.31382718463705));
#54414=CARTESIAN_POINT('Ctrl Pts',(-4.60047417080891,-25.865320235125,-9.28705554295689));
#54415=CARTESIAN_POINT('Ctrl Pts',(-4.50463790934284,-25.8741455223677,
-9.26304224523494));
#54416=CARTESIAN_POINT('Ctrl Pts',(-4.41602611056628,-25.8820979118167,
-9.24146192010301));
#54417=CARTESIAN_POINT('Ctrl Pts',(-4.38394681488766,-25.8849768405374,
-9.23364939806524));
#54418=CARTESIAN_POINT('Ctrl Pts',(-4.35281410508567,-25.8877412796611,
-9.22615615817267));
#54419=CARTESIAN_POINT('Ctrl Pts',(-4.3226323863034,-25.8903956683114,-9.21896821569922));
#54420=CARTESIAN_POINT('Ctrl Pts',(-4.28802313193754,-25.8934394449979,
-9.21072583125368));
#54421=CARTESIAN_POINT('Ctrl Pts',(-4.25466435763063,-25.8963385236158,
-9.20288485679624));
#54422=CARTESIAN_POINT('Ctrl Pts',(-4.22256207443942,-25.8990992696321,
-9.1954255081038));
#54423=CARTESIAN_POINT('Ctrl Pts',(-4.20651093284382,-25.9004796426402,
-9.19169583375758));
#54424=CARTESIAN_POINT('Ctrl Pts',(-4.19077391402756,-25.901825434645,-9.18806156664566));
#54425=CARTESIAN_POINT('Ctrl Pts',(-4.17535169773152,-25.9031373973644,
-9.18452039028601));
#54426=CARTESIAN_POINT('Ctrl Pts',(-4.1676405895835,-25.9037933787241,-9.18274980210618));
#54427=CARTESIAN_POINT('Ctrl Pts',(-4.16000818206553,-25.9044409028845,
-9.18100248665958));
#54428=CARTESIAN_POINT('Ctrl Pts',(-4.15245455838758,-25.9050800628873,
-9.17927815906634));
#54429=CARTESIAN_POINT('Ctrl Pts',(-4.14867774654861,-25.9053996428886,
-9.17841599526972));
#54430=CARTESIAN_POINT('Ctrl Pts',(-4.14492063066965,-25.9057171318577,
-9.17755957843908));
#54431=CARTESIAN_POINT('Ctrl Pts',(-4.14118322091831,-25.9060325412745,
-9.17670887350226));
#54432=CARTESIAN_POINT('Ctrl Pts',(-4.13931451604264,-25.9061902459829,
-9.17628352103385));
#54433=CARTESIAN_POINT('Ctrl Pts',(-4.13745073769887,-25.9063474308037,
-9.17585959653905));
#54434=CARTESIAN_POINT('Ctrl Pts',(-4.13559188714296,-25.9065040971616,
-9.17543709566931));
#54435=CARTESIAN_POINT('Ctrl Pts',(-4.13373303658705,-25.9066607635196,
-9.17501459479957));
#54436=CARTESIAN_POINT('Ctrl Pts',(-4.13363444556609,-25.9066691641448,
-9.17499191745734));
#54437=CARTESIAN_POINT('Ctrl Pts',(-4.1300301200903,-25.9069725422699,-9.17417385959775));
#54438=CARTESIAN_POINT('Ctrl Pts',(-4.08661760549322,-25.9106265983135,
-9.16432071259167));
#54439=CARTESIAN_POINT('Ctrl Pts',(-4.04433457952546,-25.9141332066327,
-9.15487888299753));
#54440=CARTESIAN_POINT('Ctrl Pts',(-4.00318800195899,-25.9174995886589,
-9.14582562332909));
#54441=CARTESIAN_POINT('Ctrl Pts',(-3.90004608897409,-25.9259380810574,
-9.12313186418366));
#54442=CARTESIAN_POINT('Ctrl Pts',(-3.80404668550376,-25.9334963251751,
-9.10287652665312));
#54443=CARTESIAN_POINT('Ctrl Pts',(-3.71528285380719,-25.9402828195675,
-9.08473148518902));
#54444=CARTESIAN_POINT('Ctrl Pts',(-3.627035643983,-25.9470298153109,-9.06669205121298));
#54445=CARTESIAN_POINT('Ctrl Pts',(-3.54593976008338,-25.9530141365386,
-9.05073831598289));
#54446=CARTESIAN_POINT('Ctrl Pts',(-3.47206598411144,-25.9583296823689,
-9.03659310550064));
#54447=CARTESIAN_POINT('Ctrl Pts',(-3.41362152278194,-25.9625350205777,
-9.02540227091624));
#54448=CARTESIAN_POINT('Ctrl Pts',(-3.35969695816188,-25.9663215400282,
-9.0153442568734));
#54449=CARTESIAN_POINT('Ctrl Pts',(-3.31031961185454,-25.9697293685188,
-9.00630267440747));
#54450=CARTESIAN_POINT('Ctrl Pts',(-3.27705079779092,-25.9720254500398,
-9.00021075678946));
#54451=CARTESIAN_POINT('Ctrl Pts',(-3.24584610897252,-25.9741495022497,
-8.994580642952));
#54452=CARTESIAN_POINT('Ctrl Pts',(-3.21671236822705,-25.9761122277145,
-8.98938162097428));
#54453=CARTESIAN_POINT('Ctrl Pts',(-3.20214549785432,-25.9770935904469,
-8.98678210998543));
#54454=CARTESIAN_POINT('Ctrl Pts',(-3.1880963645055,-25.9780346232269,-8.98429037258426));
#54455=CARTESIAN_POINT('Ctrl Pts',(-3.17456569417812,-25.9789365146577,
-8.98190301543562));
#54456=CARTESIAN_POINT('Ctrl Pts',(-3.16780035901443,-25.9793874603731,
-8.9807093368613));
#54457=CARTESIAN_POINT('Ctrl Pts',(-3.16116463960638,-25.9798286208403,
-8.97954175338216));
#54458=CARTESIAN_POINT('Ctrl Pts',(-3.15465862374933,-25.9802601405916,
-8.97839985366472));
#54459=CARTESIAN_POINT('Ctrl Pts',(-3.1514056158208,-25.9804759004673,-8.97782890380599));
#54460=CARTESIAN_POINT('Ctrl Pts',(-3.14818503378004,-25.9806892501687,
-8.97726437488937));
#54461=CARTESIAN_POINT('Ctrl Pts',(-3.14499688817315,-25.980900207222,-8.97670621709465));
#54462=CARTESIAN_POINT('Ctrl Pts',(-3.14180874256627,-25.9811111642753,
-8.97614805929993));
#54463=CARTESIAN_POINT('Ctrl Pts',(-3.13695795646078,-25.9814316329932,
-8.97530023435297));
#54464=CARTESIAN_POINT('Ctrl Pts',(-3.13552977107617,-25.9815259178094,
-8.97505080774237));
#54465=CARTESIAN_POINT('Ctrl Pts',(-3.11970257976371,-25.9825707848406,
-8.97228665490416));
#54466=CARTESIAN_POINT('Ctrl Pts',(-3.09679456800648,-25.9840828600508,
-8.96828669945725));
#54467=CARTESIAN_POINT('Ctrl Pts',(-3.06678982289584,-25.9860344425227,
-8.96312842074186));
#54468=CARTESIAN_POINT('Ctrl Pts',(-3.03690025826695,-25.9879785333725,
-8.95798994332873));
#54469=CARTESIAN_POINT('Ctrl Pts',(-2.99996826007926,-25.9903587923726,
-8.95170200207538));
#54470=CARTESIAN_POINT('Ctrl Pts',(-2.95596929739872,-25.9931304079546,
-8.94438903715539));
#54471=CARTESIAN_POINT('Ctrl Pts',(-2.9382186804789,-25.9942485680986,-8.94143874853641));
#54472=CARTESIAN_POINT('Ctrl Pts',(-2.91931776614415,-25.9954302236241,
-8.93832217564728));
#54473=CARTESIAN_POINT('Ctrl Pts',(-2.8992645887638,-25.9966716041366,-8.93504972133033));
#54474=CARTESIAN_POINT('Ctrl Pts',(-2.8497154996617,-25.9997389122471,-8.92696386403911));
#54475=CARTESIAN_POINT('Ctrl Pts',(-2.79313189633374,-26.0031721325053,
-8.91792294670148));
#54476=CARTESIAN_POINT('Ctrl Pts',(-2.72948003412134,-26.006901810286,-8.9081174418846));
#54477=CARTESIAN_POINT('Ctrl Pts',(-2.66624669988098,-26.0106069644404,
-8.89837641087733));
#54478=CARTESIAN_POINT('Ctrl Pts',(-2.5960375787483,-26.0146047328404,-8.88788080115353));
#54479=CARTESIAN_POINT('Ctrl Pts',(-2.51881565324327,-26.0188086392253,
-8.87686505424636));
#54480=CARTESIAN_POINT('Ctrl Pts',(-2.46592221941314,-26.0216881199264,
-8.8693197790371));
#54481=CARTESIAN_POINT('Ctrl Pts',(-2.40973856258863,-26.0246639339917,
-8.86153146052812));
#54482=CARTESIAN_POINT('Ctrl Pts',(-2.35025240331417,-26.0277030808939,
-8.8535885713598));
#54483=CARTESIAN_POINT('Ctrl Pts',(-2.31847580468596,-26.029326546797,-8.84934560116087));
#54484=CARTESIAN_POINT('Ctrl Pts',(-2.2857568244182,-26.0309680115456,-8.84505870662713));
#54485=CARTESIAN_POINT('Ctrl Pts',(-2.2520936107303,-26.0326219258945,-8.84074265221651));
#54486=CARTESIAN_POINT('Ctrl Pts',(-2.23526200388636,-26.033448883069,-8.8385846250112));
#54487=CARTESIAN_POINT('Ctrl Pts',(-2.21819433868372,-26.0342789518604,
-8.83641930756526));
#54488=CARTESIAN_POINT('Ctrl Pts',(-2.20089038788782,-26.0351113981157,
-8.83424864635563));
#54489=CARTESIAN_POINT('Ctrl Pts',(-2.19223841248987,-26.0355276212433,
-8.83316331575081));
#54490=CARTESIAN_POINT('Ctrl Pts',(-2.18352736569337,-26.0359444386846,
-8.83207664918696));
#54491=CARTESIAN_POINT('Ctrl Pts',(-2.17475721935004,-26.0363617573365,
-8.83098889277727));
#54492=CARTESIAN_POINT('Ctrl Pts',(-2.16817960959255,-26.0366747463254,
-8.83017307547));
#54493=CARTESIAN_POINT('Ctrl Pts',(-2.16156875633996,-26.0369880172407,
-8.82935664512291));
#54494=CARTESIAN_POINT('Ctrl Pts',(-2.15492464778689,-26.0373015303008,
-8.8285397067524));
#54495=CARTESIAN_POINT('Ctrl Pts',(-2.15270994493586,-26.0374060346541,
-8.82826739396223));
#54496=CARTESIAN_POINT('Ctrl Pts',(-2.14918581021123,-26.0375720050318,
-8.82783494548843));
#54497=CARTESIAN_POINT('Ctrl Pts',(-2.14826945370358,-26.037615122561,-8.82772260303836));
#54498=CARTESIAN_POINT('Ctrl Pts',(-2.01266622350348,-26.0439956918975,
-8.81109806990979));
#54499=CARTESIAN_POINT('Ctrl Pts',(-1.87302045106776,-26.0499592140147,
-8.79562775335127));
#54500=CARTESIAN_POINT('Ctrl Pts',(-1.72934561672299,-26.0553981437514,
-8.78158323778946));
#54501=CARTESIAN_POINT('Ctrl Pts',(-1.55031236599416,-26.0621755955974,
-8.76408236307183));
#54502=CARTESIAN_POINT('Ctrl Pts',(-1.36502204175769,-26.0681392785514,
-8.74879507273714));
#54503=CARTESIAN_POINT('Ctrl Pts',(-1.17351855624395,-26.0730598440868,
-8.73625149146255));
#54504=CARTESIAN_POINT('Ctrl Pts',(-0.994986214400786,-26.0776471239783,
-8.72455752707311));
#54505=CARTESIAN_POINT('Ctrl Pts',(-0.811053940501206,-26.0813276621787,
-8.71524850658676));
#54506=CARTESIAN_POINT('Ctrl Pts',(-0.621782179047148,-26.0838950606796,
-8.70877900139082));
#54507=CARTESIAN_POINT('Ctrl Pts',(-0.437432969141425,-26.0863956866659,
-8.70247775411448));
#54508=CARTESIAN_POINT('Ctrl Pts',(-0.24801674368234,-26.0878397285108,
-8.69887053619326));
#54509=CARTESIAN_POINT('Ctrl Pts',(-0.0536790750609311,-26.0880417664438,
-8.69839184997735));
#54510=CARTESIAN_POINT('Ctrl Pts',(0.0580605512452798,-26.0881579335424,
-8.69811661656912));
#54511=CARTESIAN_POINT('Ctrl Pts',(0.171426389472391,-26.0878632658087,
-8.69887602550745));
#54512=CARTESIAN_POINT('Ctrl Pts',(0.286383677659182,-26.0871206111961,
-8.700755502493));
#54513=CARTESIAN_POINT('Ctrl Pts',(0.308582461111033,-26.0869772011593,
-8.70111843818209));
#54514=CARTESIAN_POINT('Ctrl Pts',(0.330840572337808,-26.0868170817409,
-8.70152314662147));
#54515=CARTESIAN_POINT('Ctrl Pts',(0.353157737064551,-26.0866399792483,
-8.70197025192061));
#54516=CARTESIAN_POINT('Ctrl Pts',(0.484497400390817,-26.0855977060906,
-8.70460152969178));
#54517=CARTESIAN_POINT('Ctrl Pts',(0.617882879397884,-26.0839671724966,
-8.70870081522193));
#54518=CARTESIAN_POINT('Ctrl Pts',(0.753271868137669,-26.0817077353392,
-8.71440618982747));
#54519=CARTESIAN_POINT('Ctrl Pts',(0.832468974465638,-26.0803860555892,
-8.71774360421753));
#54520=CARTESIAN_POINT('Ctrl Pts',(0.912351579049761,-26.0788492375685,
-8.72163053479288));
#54521=CARTESIAN_POINT('Ctrl Pts',(0.992910103713763,-26.0770891929669,
-8.7260955784618));
#54522=CARTESIAN_POINT('Ctrl Pts',(1.03318936604576,-26.0762091706661,-8.72832810029627));
#54523=CARTESIAN_POINT('Ctrl Pts',(1.0736376083974,-26.0752733456166,-8.73070515169355));
#54524=CARTESIAN_POINT('Ctrl Pts',(1.11425355911735,-26.0742807242355,-8.73323033517445));
#54525=CARTESIAN_POINT('Ctrl Pts',(1.13456153447733,-26.0737844135449,-8.7344929269149));
#54526=CARTESIAN_POINT('Ctrl Pts',(1.15491143693055,-26.0732739040251,-8.73579255176232));
#54527=CARTESIAN_POINT('Ctrl Pts',(1.17530310417698,-26.0727490719265,-8.73712966381612));
#54528=CARTESIAN_POINT('Ctrl Pts',(1.1854989378002,-26.0724866558773,-8.73779821984302));
#54529=CARTESIAN_POINT('Ctrl Pts',(1.19570521262178,-26.0722206591995,-8.73847614767697));
#54530=CARTESIAN_POINT('Ctrl Pts',(1.20592190804525,-26.0719510664548,-8.73916350431498));
#54531=CARTESIAN_POINT('Ctrl Pts',(1.20990015194453,-26.071846090663,-8.73943115175267));
#54532=CARTESIAN_POINT('Ctrl Pts',(1.21387997583525,-26.0717405696339,-8.73970022879072));
#54533=CARTESIAN_POINT('Ctrl Pts',(1.21786137849269,-26.0716345024541,-8.73997073880825));
#54534=CARTESIAN_POINT('Ctrl Pts',(1.2189923796168,-26.0716043718419,-8.74004758286554));
#54535=CARTESIAN_POINT('Ctrl Pts',(1.22012350814158,-26.0715741971573,-8.74012454255906));
#54536=CARTESIAN_POINT('Ctrl Pts',(1.22125476403901,-26.071543978378,-8.74020161795894));
#54537=CARTESIAN_POINT('Ctrl Pts',(1.2238115417489,-26.0714756802134,-8.74037581785909));
#54538=CARTESIAN_POINT('Ctrl Pts',(1.22636897009813,-26.0714071567992,-8.7405506088244));
#54539=CARTESIAN_POINT('Ctrl Pts',(1.22892704876324,-26.0713384078877,-8.74072599163071));
#54540=CARTESIAN_POINT('Ctrl Pts',(1.23148512742836,-26.0712696589762,-8.74090137443703));
#54541=CARTESIAN_POINT('Ctrl Pts',(1.23542074353098,-26.071163456459,-8.74117233826181));
#54542=CARTESIAN_POINT('Ctrl Pts',(1.23660323538091,-26.0711314843902,-8.74125391641842));
#54543=CARTESIAN_POINT('Ctrl Pts',(1.30395073383312,-26.0693105510324,-8.74590010892824));
#54544=CARTESIAN_POINT('Ctrl Pts',(1.37844760563595,-26.067146299812,-8.75143637844141));
#54545=CARTESIAN_POINT('Ctrl Pts',(1.46006216964867,-26.064542777595,-8.75811811399493));
#54546=CARTESIAN_POINT('Ctrl Pts',(1.54172917708157,-26.0619375824215,-8.76480414305991));
#54547=CARTESIAN_POINT('Ctrl Pts',(1.63052324890772,-26.0588924819595,-8.77263715624206));
#54548=CARTESIAN_POINT('Ctrl Pts',(1.72639942053101,-26.0552949733739,-8.7819207900803));
#54549=CARTESIAN_POINT('Ctrl Pts',(1.81110726429991,-26.0521165277804,-8.79012300123937));
#54550=CARTESIAN_POINT('Ctrl Pts',(1.90134329068553,-26.0485066029823,-8.79945826899446));
#54551=CARTESIAN_POINT('Ctrl Pts',(1.99706565552955,-26.0443777045615,-8.81016651175319));
#54552=CARTESIAN_POINT('Ctrl Pts',(2.10635221589194,-26.0396637267232,-8.82239215014537));
#54553=CARTESIAN_POINT('Ctrl Pts',(2.22279080382339,-26.0342733681395,-8.83640677412009));
#54554=CARTESIAN_POINT('Ctrl Pts',(2.34629930883073,-26.0280648257203,-8.85260839878758));
#54555=CARTESIAN_POINT('Ctrl Pts',(2.462528553975,-26.0222221981314,-8.86785514317251));
#54556=CARTESIAN_POINT('Ctrl Pts',(2.58501896755301,-26.0156547777424,-8.88503916917858));
#54557=CARTESIAN_POINT('Ctrl Pts',(2.71368124103882,-26.0082351007993,-8.90452762382412));
#54558=CARTESIAN_POINT('Ctrl Pts',(2.74250184117935,-26.0065730786963,-8.90889307566542));
#54559=CARTESIAN_POINT('Ctrl Pts',(2.77163203637594,-26.0048682608314,-8.913374290048));
#54560=CARTESIAN_POINT('Ctrl Pts',(2.80107067532219,-26.0031191765166,-8.91797557208791));
#54561=CARTESIAN_POINT('Ctrl Pts',(2.82649121064435,-26.0016088261337,-8.92194882142312));
#54562=CARTESIAN_POINT('Ctrl Pts',(2.85493636831501,-25.9998980382213,-8.92645224024806));
#54563=CARTESIAN_POINT('Ctrl Pts',(2.88361403628995,-25.9981472674012,-8.93106468954868));
#54564=CARTESIAN_POINT('Ctrl Pts',(2.89878519010301,-25.9972210688893,-8.93350478258051));
#54565=CARTESIAN_POINT('Ctrl Pts',(2.9140215577521,-25.9962839629684,-8.93597460837235));
#54566=CARTESIAN_POINT('Ctrl Pts',(2.92891080622877,-25.9953617172812,-8.93840622669497));
#54567=CARTESIAN_POINT('Ctrl Pts',(3.02425371736574,-25.9894561412721,-8.95397703068931));
#54568=CARTESIAN_POINT('Ctrl Pts',(3.11262114766818,-25.9837161646081,-8.96915081969007));
#54569=CARTESIAN_POINT('Ctrl Pts',(3.19406215928281,-25.9782486650069,-8.98363485151774));
#54570=CARTESIAN_POINT('Ctrl Pts',(3.25118405732209,-25.9744138163409,-8.99379380427207));
#54571=CARTESIAN_POINT('Ctrl Pts',(3.30489854065411,-25.9707125845228,-9.00361447197882));
#54572=CARTESIAN_POINT('Ctrl Pts',(3.35522197544709,-25.9671762224164,-9.01301002420905));
#54573=CARTESIAN_POINT('Ctrl Pts',(3.427773408449,-25.962077839536,-9.02655561744909));
#54574=CARTESIAN_POINT('Ctrl Pts',(3.49327684430623,-25.9573229291771,-9.03921551278359));
#54575=CARTESIAN_POINT('Ctrl Pts',(3.55177751951473,-25.9529893719757,-9.05077090283914));
#54576=CARTESIAN_POINT('Ctrl Pts',(3.61056551398029,-25.9486345310124,-9.06238304584795));
#54577=CARTESIAN_POINT('Ctrl Pts',(3.66228194477024,-25.9447051257599,-9.07287986166669));
#54578=CARTESIAN_POINT('Ctrl Pts',(3.70696567207482,-25.9412618732795,-9.08208825809521));
#54579=CARTESIAN_POINT('Ctrl Pts',(3.75187527224184,-25.9378012154182,-9.09134320227131));
#54580=CARTESIAN_POINT('Ctrl Pts',(3.78968101170105,-25.9348315888708,-9.09929670080249));
#54581=CARTESIAN_POINT('Ctrl Pts',(3.82041316876645,-25.9323970499494,-9.10582170121249));
#54582=CARTESIAN_POINT('Ctrl Pts',(3.8268804092965,-25.9318847283199,-9.10719481495197));
#54583=CARTESIAN_POINT('Ctrl Pts',(3.83303436389836,-25.9313960424363,-9.10850483834948));
#54584=CARTESIAN_POINT('Ctrl Pts',(3.83887525621521,-25.9309313071267,-9.10975085836551));
#54585=CARTESIAN_POINT('Ctrl Pts',(3.8511418551453,-25.9299553052862,-9.11236765507504));
#54586=CARTESIAN_POINT('Ctrl Pts',(3.86202771366167,-25.9290849785934,-9.11470204665891));
#54587=CARTESIAN_POINT('Ctrl Pts',(3.87153458996032,-25.9283227689994,-9.11674693379315));
#54588=CARTESIAN_POINT('Ctrl Pts',(3.87628802810965,-25.9279416642024,-9.11776937736027));
#54589=CARTESIAN_POINT('Ctrl Pts',(3.8806967207052,-25.9275875891028,-9.11871944496946));
#54590=CARTESIAN_POINT('Ctrl Pts',(3.88476083919448,-25.927260777662,-9.1195964528732));
#54591=CARTESIAN_POINT('Ctrl Pts',(3.88679289843912,-25.9270973719416,-9.12003495682507));
#54592=CARTESIAN_POINT('Ctrl Pts',(3.88873881415724,-25.9269407821652,-9.1204551958613));
#54593=CARTESIAN_POINT('Ctrl Pts',(3.89059860635588,-25.926791035726,-9.12085709015195));
#54594=CARTESIAN_POINT('Ctrl Pts',(3.8915285024552,-25.9267161625064,-9.12105803729728));
#54595=CARTESIAN_POINT('Ctrl Pts',(3.89243686767465,-25.926643000123,-9.12125439825693));
#54596=CARTESIAN_POINT('Ctrl Pts',(3.89332370434875,-25.9265715517621,-9.12144616374056));
#54597=CARTESIAN_POINT('Ctrl Pts',(3.89376712268579,-25.9265358275816,-9.12154204648237));
#54598=CARTESIAN_POINT('Ctrl Pts',(3.89420515887107,-25.9265005318859,-9.12163678041626));
#54599=CARTESIAN_POINT('Ctrl Pts',(3.89463512416906,-25.9264658820949,-9.12172978186106));
#54600=CARTESIAN_POINT('Ctrl Pts',(3.89506508946705,-25.9264312323039,-9.12182278330586));
#54601=CARTESIAN_POINT('Ctrl Pts',(3.89549238058995,-25.926396819668,-9.12191514342382));
#54602=CARTESIAN_POINT('Ctrl Pts',(3.89721720697796,-25.9262577386616,-9.12228846130778));
#54603=CARTESIAN_POINT('Ctrl Pts',(3.9060039205876,-25.9255492238917,-9.12419023957051));
#54604=CARTESIAN_POINT('Ctrl Pts',(3.91477185382022,-25.9248400577957,-9.12609425770661));
#54605=CARTESIAN_POINT('Ctrl Pts',(3.92352101537451,-25.9241302699203,-9.12800043834213));
#54606=CARTESIAN_POINT('Ctrl Pts',(4.08352595055138,-25.9111496474579,-9.16286072834021));
#54607=CARTESIAN_POINT('Ctrl Pts',(4.2372515957779,-25.8979630799124,-9.19844051498696));
#54608=CARTESIAN_POINT('Ctrl Pts',(4.38475854301892,-25.8847426375439,-9.23428876981734));
#54609=CARTESIAN_POINT('Ctrl Pts',(4.40472993871036,-25.8829526833031,-9.23914236956607));
#54610=CARTESIAN_POINT('Ctrl Pts',(4.42458735601385,-25.8811620725191,-9.2440009577067));
#54611=CARTESIAN_POINT('Ctrl Pts',(4.44433096147399,-25.879371199339,-9.24886347726735));
#54612=CARTESIAN_POINT('Ctrl Pts',(4.59308062293749,-25.8658786394415,-9.28549802914619));
#54613=CARTESIAN_POINT('Ctrl Pts',(4.73536929234841,-25.8523732550644,-9.32235201322874));
#54614=CARTESIAN_POINT('Ctrl Pts',(4.87127285544964,-25.8390137277172,-9.35900010657507));
#54615=CARTESIAN_POINT('Ctrl Pts',(4.89543477021471,-25.836638574677,-9.36551566869522));
#54616=CARTESIAN_POINT('Ctrl Pts',(4.9193948852595,-25.8342679688519,-9.37202483785233));
#54617=CARTESIAN_POINT('Ctrl Pts',(4.9431536540866,-25.8319027217208,-9.37852537158515));
#54618=CARTESIAN_POINT('Ctrl Pts',(5.07994861810915,-25.8182844278368,-9.41595324861781));
#54619=CARTESIAN_POINT('Ctrl Pts',(5.21006827342324,-25.8048459299023,-9.45309118221072));
#54620=CARTESIAN_POINT('Ctrl Pts',(5.33360072841922,-25.7917314277818,-9.489540727972));
#54621=CARTESIAN_POINT('Ctrl Pts',(5.36979447838387,-25.787889012356,-9.50022007329588));
#54622=CARTESIAN_POINT('Ctrl Pts',(5.40542280302128,-25.7840742393724,-9.51084062080672));
#54623=CARTESIAN_POINT('Ctrl Pts',(5.44048800084055,-25.7802903253814,-9.52139307544913));
#54624=CARTESIAN_POINT('Ctrl Pts',(5.56340174988859,-25.7670266028409,-9.55838250777583));
#54625=CARTESIAN_POINT('Ctrl Pts',(5.6793960161412,-25.7541441947357,-9.59453182277264));
#54626=CARTESIAN_POINT('Ctrl Pts',(5.78856808116882,-25.7417693278559,-9.62947415865375));
#54627=CARTESIAN_POINT('Ctrl Pts',(5.84238474412072,-25.735669103959,-9.64669907706479));
#54628=CARTESIAN_POINT('Ctrl Pts',(5.89454365554831,-25.7296917865968,-9.66363139276406));
#54629=CARTESIAN_POINT('Ctrl Pts',(5.94505661807474,-25.7238501735518,-9.68023115871441));
#54630=CARTESIAN_POINT('Ctrl Pts',(5.9596842864737,-25.722158544824,-9.68503815992117));
#54631=CARTESIAN_POINT('Ctrl Pts',(5.97417392860902,-25.720478286976,-9.68981729094707));
#54632=CARTESIAN_POINT('Ctrl Pts',(5.98852581858797,-25.7188097024617,-9.6945676349031));
#54633=CARTESIAN_POINT('Ctrl Pts',(-6.39567215644055,-25.5334667653534,
-8.78352118705417));
#54634=CARTESIAN_POINT('Ctrl Pts',(-6.35564925718895,-25.5378748085094,
-8.77012419398008));
#54635=CARTESIAN_POINT('Ctrl Pts',(-5.98525024729305,-25.578353672155,-8.64740198386364));
#54636=CARTESIAN_POINT('Ctrl Pts',(-5.25616848901603,-25.6522246220423,
-8.42856426610991));
#54637=CARTESIAN_POINT('Ctrl Pts',(-4.17576488242819,-25.743621550053,-8.16491332440422));
#54638=CARTESIAN_POINT('Ctrl Pts',(-3.01937236728622,-25.8195370899232,
-7.95089144637005));
#54639=CARTESIAN_POINT('Ctrl Pts',(-1.83578745054832,-25.8725333118012,
-7.80507997421356));
#54640=CARTESIAN_POINT('Ctrl Pts',(-0.697920992822499,-25.8989854873888,
-7.73463084102237));
#54641=CARTESIAN_POINT('Ctrl Pts',(0.331415178953193,-25.9017875496813,
-7.72744135310422));
#54642=CARTESIAN_POINT('Ctrl Pts',(1.24581749154929,-25.8874717448211,-7.76509324630723));
#54643=CARTESIAN_POINT('Ctrl Pts',(2.07031043576891,-25.8615908861053,-7.83520428425946));
#54644=CARTESIAN_POINT('Ctrl Pts',(2.81707948213384,-25.8276633033017,-7.9287568097775));
#54645=CARTESIAN_POINT('Ctrl Pts',(3.49019584722931,-25.7886676982261,-8.037881035032));
#54646=CARTESIAN_POINT('Ctrl Pts',(4.09498188336493,-25.7470110244898,-8.15592462114486));
#54647=CARTESIAN_POINT('Ctrl Pts',(4.65006137406161,-25.7034067880011,-8.28093045992463));
#54648=CARTESIAN_POINT('Ctrl Pts',(5.1805088354666,-25.6570334421092,-8.41545276582232));
#54649=CARTESIAN_POINT('Ctrl Pts',(5.70542717861576,-25.6067226998712,-8.56333529062248));
#54650=CARTESIAN_POINT('Ctrl Pts',(6.10978535963893,-25.5646819644592,-8.68891077621009));
#54651=CARTESIAN_POINT('Ctrl Pts',(6.34031713688981,-25.5395629979994,-8.76499255552385));
#54652=CARTESIAN_POINT('Ctrl Pts',(6.39541677264867,-25.5334956821542,-8.783436799282));
#54653=CARTESIAN_POINT('Ctrl Pts',(-6.33018760766523,-25.7767195002423,
-9.0673579311918));
#54654=CARTESIAN_POINT('Ctrl Pts',(-6.29063887077213,-25.7811601733469,
-9.05404229513906));
#54655=CARTESIAN_POINT('Ctrl Pts',(-5.9246008136023,-25.8219416068059,-8.9320552503747));
#54656=CARTESIAN_POINT('Ctrl Pts',(-5.20363827098165,-25.8964098971313,
-8.7143622180441));
#54657=CARTESIAN_POINT('Ctrl Pts',(-4.13466637401218,-25.9886138348841,
-8.45189574262935));
#54658=CARTESIAN_POINT('Ctrl Pts',(-2.99013371586683,-26.0652394577625,
-8.23872385364562));
#54659=CARTESIAN_POINT('Ctrl Pts',(-1.8183506761573,-26.1187440570414,-8.09343083226769));
#54660=CARTESIAN_POINT('Ctrl Pts',(-0.69152385866634,-26.1454448732183,
-8.02320443539093));
#54661=CARTESIAN_POINT('Ctrl Pts',(0.328416326756525,-26.1482718798261,
-8.01603491323138));
#54662=CARTESIAN_POINT('Ctrl Pts',(1.23411374808423,-26.1338238284116,-8.05357264195744));
#54663=CARTESIAN_POINT('Ctrl Pts',(2.05053453836073,-26.1076962181796,-8.12344815886598));
#54664=CARTESIAN_POINT('Ctrl Pts',(2.78984559872145,-26.073444587786,-8.21666390189123));
#54665=CARTESIAN_POINT('Ctrl Pts',(3.45612791104389,-26.0340809624483,-8.32536882872224));
#54666=CARTESIAN_POINT('Ctrl Pts',(4.05467909015723,-25.9920396096016,-8.44292969175125));
#54667=CARTESIAN_POINT('Ctrl Pts',(4.60394317824861,-25.9480439491093,-8.56739151877058));
#54668=CARTESIAN_POINT('Ctrl Pts',(5.12872579717185,-25.9012684884609,-8.70128826221729));
#54669=CARTESIAN_POINT('Ctrl Pts',(5.64789551119545,-25.8505397548962,-8.84842891857438));
#54670=CARTESIAN_POINT('Ctrl Pts',(6.04766431563905,-25.8081682551775,-8.97331340642041));
#54671=CARTESIAN_POINT('Ctrl Pts',(6.27548853167199,-25.7828608658207,-9.0489418703681));
#54672=CARTESIAN_POINT('Ctrl Pts',(6.32993492696099,-25.7767485946731,-9.06727395103012));
#54673=CARTESIAN_POINT('Ctrl Pts',(-6.21932807443185,-25.8366561953098,
-9.42526544364698));
#54674=CARTESIAN_POINT('Ctrl Pts',(-6.18048319064934,-25.8411258831892,
-9.41216291856682));
#54675=CARTESIAN_POINT('Ctrl Pts',(-5.82094596423115,-25.8821753788867,
-9.2921233703167));
#54676=CARTESIAN_POINT('Ctrl Pts',(-5.11256521731997,-25.9571564779671,
-9.07782999761601));
#54677=CARTESIAN_POINT('Ctrl Pts',(-4.06220012752473,-26.050033738679,-8.81943609738017));
#54678=CARTESIAN_POINT('Ctrl Pts',(-2.93773661016636,-26.1272380042585,
-8.60958393773643));
#54679=CARTESIAN_POINT('Ctrl Pts',(-1.78661031458413,-26.181144206621,-8.46656055933674));
#54680=CARTESIAN_POINT('Ctrl Pts',(-0.679624998528299,-26.2080305784431,
-8.39742173764442));
#54681=CARTESIAN_POINT('Ctrl Pts',(0.322797658933812,-26.2108747126336,
-8.39036078365421));
#54682=CARTESIAN_POINT('Ctrl Pts',(1.21266000783635,-26.1963305309027,-8.42732124814706));
#54683=CARTESIAN_POINT('Ctrl Pts',(2.01470259288328,-26.1700129285436,-8.49610835129674));
#54684=CARTESIAN_POINT('Ctrl Pts',(2.74098505369467,-26.1355047474246,-8.58786922908991));
#54685=CARTESIAN_POINT('Ctrl Pts',(3.39555710167175,-26.0958440060889,-8.69487932361028));
#54686=CARTESIAN_POINT('Ctrl Pts',(3.98362867447789,-26.0534876192753,-8.81061117452099));
#54687=CARTESIAN_POINT('Ctrl Pts',(4.52330902351571,-26.0091675072182,-8.93313965918623));
#54688=CARTESIAN_POINT('Ctrl Pts',(5.03895227535259,-25.9620546978064,-9.06495615570801));
#54689=CARTESIAN_POINT('Ctrl Pts',(5.54907007362038,-25.9109702775198,-9.20980289930939));
#54690=CARTESIAN_POINT('Ctrl Pts',(5.94182116576813,-25.8683117841367,-9.33272190788584));
#54691=CARTESIAN_POINT('Ctrl Pts',(6.16560261524064,-25.842837696862,-9.40714417382229));
#54692=CARTESIAN_POINT('Ctrl Pts',(6.21907959820766,-25.8366854345371,-9.42518270291576));
#54693=CARTESIAN_POINT('Ctrl Pts',(-6.09477939300047,-25.6963156654864,
-9.75500591347859));
#54694=CARTESIAN_POINT('Ctrl Pts',(-6.05666692574697,-25.7008024726199,
-9.74218730560947));
#54695=CARTESIAN_POINT('Ctrl Pts',(-5.70391276856241,-25.742009023419,-9.62475061279524));
#54696=CARTESIAN_POINT('Ctrl Pts',(-5.0089808343114,-25.8172720694164,-9.41513947846463));
#54697=CARTESIAN_POINT('Ctrl Pts',(-3.97907981782402,-25.9104968519052,
-9.16254124191398));
#54698=CARTESIAN_POINT('Ctrl Pts',(-2.87715857377971,-25.9879832334434,
-8.95752879977658));
#54699=CARTESIAN_POINT('Ctrl Pts',(-1.74963945844121,-26.0420697001683,
-8.81787687582311));
#54700=CARTESIAN_POINT('Ctrl Pts',(-0.665625857011165,-26.0690256208802,
-8.75037927471988));
#54701=CARTESIAN_POINT('Ctrl Pts',(0.316165362970241,-26.0718741826498,
-8.7434844242914));
#54702=CARTESIAN_POINT('Ctrl Pts',(1.18758896401743,-26.0572974010932,-8.77956970368741));
#54703=CARTESIAN_POINT('Ctrl Pts',(1.97305721072115,-26.0309007595064,-8.84672692345386));
#54704=CARTESIAN_POINT('Ctrl Pts',(2.68446448312301,-25.9962767107602,-8.93633110958157));
#54705=CARTESIAN_POINT('Ctrl Pts',(3.32579714718034,-25.9564745219278,-9.04085572994667));
#54706=CARTESIAN_POINT('Ctrl Pts',(3.90213960567823,-25.9139626268742,-9.15393553592159));
#54707=CARTESIAN_POINT('Ctrl Pts',(4.43120697430674,-25.8694776070166,-9.27369442375866));
#54708=CARTESIAN_POINT('Ctrl Pts',(4.9368483277969,-25.8221884699618,-9.40257105750336));
#54709=CARTESIAN_POINT('Ctrl Pts',(5.43719781099545,-25.7709121598798,-9.54422799064497));
#54710=CARTESIAN_POINT('Ctrl Pts',(5.82250829244966,-25.7280923401021,-9.66446919527306));
#54711=CARTESIAN_POINT('Ctrl Pts',(6.04206701108776,-25.7025208518976,-9.73727734754774));
#54712=CARTESIAN_POINT('Ctrl Pts',(6.09453542110669,-25.6963449753506,-9.75492488947298));
#54713=CARTESIAN_POINT('',(6.2715945487114,-25.5608537657928,-8.76071457496679));
#54714=CARTESIAN_POINT('Origin',(5.999999949026,-24.7867247244533,-9.33250966433407));
#54715=CARTESIAN_POINT('Ctrl Pts',(-6.27159387328033,-25.5608571664718,
-8.76070928018898));
#54716=CARTESIAN_POINT('Ctrl Pts',(-6.13239662748639,-25.5759656514786,
-8.7150479758369));
#54717=CARTESIAN_POINT('Ctrl Pts',(-5.98564488114135,-25.5914802309821,
-8.66855401201454));
#54718=CARTESIAN_POINT('Ctrl Pts',(-5.8313285777228,-25.6072278292077,-8.62173958399663));
#54719=CARTESIAN_POINT('Ctrl Pts',(-5.67907400717005,-25.6227650326784,
-8.57555061707842));
#54720=CARTESIAN_POINT('Ctrl Pts',(-5.5194553658102,-25.638529254758,-8.5290498308945));
#54721=CARTESIAN_POINT('Ctrl Pts',(-5.3524722987654,-25.6543232435974,-8.48276837708628));
#54722=CARTESIAN_POINT('Ctrl Pts',(-5.32566767468479,-25.6568585421822,
-8.47533913894142));
#54723=CARTESIAN_POINT('Ctrl Pts',(-5.29867331186681,-25.6593945386632,
-8.46791563305459));
#54724=CARTESIAN_POINT('Ctrl Pts',(-5.27148923944926,-25.6619303363728,
-8.46050014861381));
#54725=CARTESIAN_POINT('Ctrl Pts',(-5.14595591345888,-25.6736403964273,
-8.42625618356754));
#54726=CARTESIAN_POINT('Ctrl Pts',(-5.01637663597878,-25.6853468539278,
-8.39218216515349));
#54727=CARTESIAN_POINT('Ctrl Pts',(-4.88275737867318,-25.6969639530219,
-8.35851823953318));
#54728=CARTESIAN_POINT('Ctrl Pts',(-4.71106404924362,-25.7118912805792,
-8.31526196354444));
#54729=CARTESIAN_POINT('Ctrl Pts',(-4.53269546289204,-25.7266725141005,
-8.2726803045729));
#54730=CARTESIAN_POINT('Ctrl Pts',(-4.34764543288302,-25.7411116027605,
-8.23131616579629));
#54731=CARTESIAN_POINT('Ctrl Pts',(-4.29584179776617,-25.7451537381783,
-8.21973652567409));
#54732=CARTESIAN_POINT('Ctrl Pts',(-4.24351464845383,-25.749168908436,-8.20825255408196));
#54733=CARTESIAN_POINT('Ctrl Pts',(-4.1906640978516,-25.7531524513767,-8.19687675629923));
#54734=CARTESIAN_POINT('Ctrl Pts',(-4.1433877342813,-25.7567158470692,-8.18670077240217));
#54735=CARTESIAN_POINT('Ctrl Pts',(-4.09569255336367,-25.7602539316812,
-8.17661135076348));
#54736=CARTESIAN_POINT('Ctrl Pts',(-4.04757898367837,-25.763763442795,-8.16661761563247));
#54737=CARTESIAN_POINT('Ctrl Pts',(-3.90056246621801,-25.7744871555712,
-8.13608061442903));
#54738=CARTESIAN_POINT('Ctrl Pts',(-3.74963596581336,-25.7849451013877,
-8.10643536982598));
#54739=CARTESIAN_POINT('Ctrl Pts',(-3.59479965807767,-25.7950405862901,
-8.07795017483715));
#54740=CARTESIAN_POINT('Ctrl Pts',(-3.51738150420983,-25.8000883287413,
-8.06370757734273));
#54741=CARTESIAN_POINT('Ctrl Pts',(-3.43898588989754,-25.8050453466729,
-8.04975523678017));
#54742=CARTESIAN_POINT('Ctrl Pts',(-3.35961278777928,-25.8098988466742,
-8.03612821016658));
#54743=CARTESIAN_POINT('Ctrl Pts',(-3.31992623672015,-25.8123255966748,
-8.02931469685979));
#54744=CARTESIAN_POINT('Ctrl Pts',(-3.27999531131834,-25.8147264547301,
-8.02258252194119));
#54745=CARTESIAN_POINT('Ctrl Pts',(-3.23982000760281,-25.8170997783463,
-8.01593617415272));
#54746=CARTESIAN_POINT('Ctrl Pts',(-3.21973235574504,-25.8182864401545,
-8.01261300025848));
#54747=CARTESIAN_POINT('Ctrl Pts',(-3.19958360915905,-25.8194662175381,
-8.00931128379531));
#54748=CARTESIAN_POINT('Ctrl Pts',(-3.17937376685695,-25.8206389011645,
-8.00603159108714));
#54749=CARTESIAN_POINT('Ctrl Pts',(-3.16169015484261,-25.8216649993376,
-8.00316185996749));
#54750=CARTESIAN_POINT('Ctrl Pts',(-3.1439597664119,-25.8226856663045,-8.00030899082377));
#54751=CARTESIAN_POINT('Ctrl Pts',(-3.12618260080978,-25.8237007603499,
-7.99747336560969));
#54752=CARTESIAN_POINT('Ctrl Pts',(-3.12364300572377,-25.8238457737849,
-7.99706827629339));
#54753=CARTESIAN_POINT('Ctrl Pts',(-3.119862030777,-25.8240613385894,-7.99646617212091));
#54754=CARTESIAN_POINT('Ctrl Pts',(-3.11856095164579,-25.8241354590471,
-7.99625915455978));
#54755=CARTESIAN_POINT('Ctrl Pts',(-3.09161417078269,-25.8256705753082,
-7.99197159301134));
#54756=CARTESIAN_POINT('Ctrl Pts',(-3.06344233361257,-25.8272571050421,
-7.98754642079284));
#54757=CARTESIAN_POINT('Ctrl Pts',(-3.03404546696661,-25.8288893695084,
-7.98299952580576));
#54758=CARTESIAN_POINT('Ctrl Pts',(-2.96197962651402,-25.8328908337468,
-7.97185290216591));
#54759=CARTESIAN_POINT('Ctrl Pts',(-2.88255169635183,-25.8371684006697,
-7.95997137232352));
#54760=CARTESIAN_POINT('Ctrl Pts',(-2.79576131083062,-25.841626199276,-7.94762271516167));
#54761=CARTESIAN_POINT('Ctrl Pts',(-2.70930117926136,-25.8460670351093,
-7.93532104699295));
#54762=CARTESIAN_POINT('Ctrl Pts',(-2.61553427012774,-25.8506867792073,
-7.92255580484241));
#54763=CARTESIAN_POINT('Ctrl Pts',(-2.51446131570232,-25.8553724137153,
-7.9096401288769));
#54764=CARTESIAN_POINT('Ctrl Pts',(-2.50259867559497,-25.855922353075,-7.90812425337299));
#54765=CARTESIAN_POINT('Ctrl Pts',(-2.4906353982387,-25.8564731788712,-7.90660636062048));
#54766=CARTESIAN_POINT('Ctrl Pts',(-2.47857148836738,-25.8570246913402,
-7.90508700081806));
#54767=CARTESIAN_POINT('Ctrl Pts',(-2.3768856639869,-25.861673350081,-7.89228042685596));
#54768=CARTESIAN_POINT('Ctrl Pts',(-2.26804985194134,-25.8663725618713,
-7.8793660063024));
#54769=CARTESIAN_POINT('Ctrl Pts',(-2.1520628455556,-25.8709939026914,-7.86670051264183));
#54770=CARTESIAN_POINT('Ctrl Pts',(-2.11969740242275,-25.8722834587216,
-7.86316628645914));
#54771=CARTESIAN_POINT('Ctrl Pts',(-2.08677517449752,-25.873566836411,-7.85965172837312));
#54772=CARTESIAN_POINT('Ctrl Pts',(-2.05329625573017,-25.8748409749134,
-7.85616525556634));
#54773=CARTESIAN_POINT('Ctrl Pts',(-1.9765681295929,-25.8777610889233,-7.84817483845787));
#54774=CARTESIAN_POINT('Ctrl Pts',(-1.89691552648792,-25.8806329588327,
-7.840331393524));
#54775=CARTESIAN_POINT('Ctrl Pts',(-1.81433840119601,-25.883417618283,-7.83274216281742));
#54776=CARTESIAN_POINT('Ctrl Pts',(-1.81240188497499,-25.8834829213337,
-7.83256418776299));
#54777=CARTESIAN_POINT('Ctrl Pts',(-1.81046376043746,-25.8835481761546,
-7.83238635274822));
#54778=CARTESIAN_POINT('Ctrl Pts',(-1.80852402756431,-25.8836133822471,
-7.83220865924));
#54779=CARTESIAN_POINT('Ctrl Pts',(-1.76910661538462,-25.8849384386295,
-7.8285977402562));
#54780=CARTESIAN_POINT('Ctrl Pts',(-1.72902503616309,-25.8862433884901,
-7.82504522437304));
#54781=CARTESIAN_POINT('Ctrl Pts',(-1.68827931318858,-25.8875239411659,
-7.82156332394353));
#54782=CARTESIAN_POINT('Ctrl Pts',(-1.66690390214362,-25.8881957255352,
-7.8197367014795));
#54783=CARTESIAN_POINT('Ctrl Pts',(-1.6453457107572,-25.8888607906522,-7.81792951673663));
#54784=CARTESIAN_POINT('Ctrl Pts',(-1.62360473988849,-25.8895184934827,
-7.81614356885966));
#54785=CARTESIAN_POINT('Ctrl Pts',(-1.61273425445413,-25.889847344898,-7.81525059492118));
#54786=CARTESIAN_POINT('Ctrl Pts',(-1.60181807411424,-25.8901743553977,
-7.81436293047768));
#54787=CARTESIAN_POINT('Ctrl Pts',(-1.59085619897136,-25.8904994435564,
-7.81348080339152));
#54788=CARTESIAN_POINT('Ctrl Pts',(-1.58537526139992,-25.8906619876357,
-7.81303973984844));
#54789=CARTESIAN_POINT('Ctrl Pts',(-1.57988290012557,-25.8908240511081,
-7.81260006066224));
#54790=CARTESIAN_POINT('Ctrl Pts',(-1.57437911516126,-25.8909856237326,
-7.8121617945058));
#54791=CARTESIAN_POINT('Ctrl Pts',(-1.56887533019695,-25.891147196357,-7.81172352834936));
#54792=CARTESIAN_POINT('Ctrl Pts',(-1.56205960297571,-25.8913460657113,
-7.81118421489639));
#54793=CARTESIAN_POINT('Ctrl Pts',(-1.5578334892067,-25.891468858754,-7.8108512638946));
#54794=CARTESIAN_POINT('Ctrl Pts',(-1.3321001972036,-25.8980277162027,-7.79306704656922));
#54795=CARTESIAN_POINT('Ctrl Pts',(-1.11005352541792,-25.9030588998715,
-7.77943809159168));
#54796=CARTESIAN_POINT('Ctrl Pts',(-0.891696532275825,-25.9066954304679,
-7.76958901908101));
#54797=CARTESIAN_POINT('Ctrl Pts',(-0.848420448729468,-25.9074161529858,
-7.76763703541109));
#54798=CARTESIAN_POINT('Ctrl Pts',(-0.805289186957621,-25.9080820818315,
-7.76583364729354));
#54799=CARTESIAN_POINT('Ctrl Pts',(-0.762302618692336,-25.9086942325735,
-7.76417611600142));
#54800=CARTESIAN_POINT('Ctrl Pts',(-0.724715197699748,-25.9092294966938,
-7.76272677196211));
#54801=CARTESIAN_POINT('Ctrl Pts',(-0.687238390643442,-25.9097236225523,
-7.76138892166378));
#54802=CARTESIAN_POINT('Ctrl Pts',(-0.649872395352755,-25.9101771897174,
-7.76016066762126));
#54803=CARTESIAN_POINT('Ctrl Pts',(-0.558062488216829,-25.9112916243521,
-7.75714279298135));
#54804=CARTESIAN_POINT('Ctrl Pts',(-0.466921605523578,-25.9121612251801,
-7.75478648506841));
#54805=CARTESIAN_POINT('Ctrl Pts',(-0.376448981809044,-25.912796745889,
-7.75306363614118));
#54806=CARTESIAN_POINT('Ctrl Pts',(-0.312801804844112,-25.9132438325033,
-7.75185161789683));
#54807=CARTESIAN_POINT('Ctrl Pts',(-0.249485514272613,-25.9135750126004,
-7.75095306738243));
#54808=CARTESIAN_POINT('Ctrl Pts',(-0.186500110414278,-25.9137938241859,
-7.75035834249019));
#54809=CARTESIAN_POINT('Ctrl Pts',(-0.155007408485111,-25.9139032299786,
-7.75006098004408));
#54810=CARTESIAN_POINT('Ctrl Pts',(-0.123597428111178,-25.913984541275,
-7.74983957593512));
#54811=CARTESIAN_POINT('Ctrl Pts',(-0.0922701689136151,-25.9140381882415,
-7.74969293845181));
#54812=CARTESIAN_POINT('Ctrl Pts',(-0.0647192814703127,-25.9140853682876,
-7.7495639775117));
#54813=CARTESIAN_POINT('Ctrl Pts',(-0.038338168266232,-25.9141107437916,
-7.74949397649207));
#54814=CARTESIAN_POINT('Ctrl Pts',(-0.0102093428318921,-25.9141157543342,
-7.74947894130717));
#54815=CARTESIAN_POINT('Ctrl Pts',(-0.00635375371269017,-25.9141164411241,
-7.74947688044987));
#54816=CARTESIAN_POINT('Ctrl Pts',(-0.00246532864027055,-25.9141167170767,
-7.74947592678315));
#54817=CARTESIAN_POINT('Ctrl Pts',(0.00146344560313601,-25.914116558326,
-7.74947614275909));
#54818=CARTESIAN_POINT('Ctrl Pts',(0.123999816235535,-25.9141116069754,
-7.74948287893321));
#54819=CARTESIAN_POINT('Ctrl Pts',(0.246532789979175,-25.913695197672,-7.75063931458382));
#54820=CARTESIAN_POINT('Ctrl Pts',(0.369067470035637,-25.9128590922614,
-7.75293722185313));
#54821=CARTESIAN_POINT('Ctrl Pts',(0.644882197451568,-25.9109770929301,
-7.75810960788148));
#54822=CARTESIAN_POINT('Ctrl Pts',(0.920705383094992,-25.906969775555,-7.76906208263353));
#54823=CARTESIAN_POINT('Ctrl Pts',(1.19652643911715,-25.9008589498774,-7.78581258443593));
#54824=CARTESIAN_POINT('Ctrl Pts',(1.22212487704151,-25.9002918155403,-7.78736716727589));
#54825=CARTESIAN_POINT('Ctrl Pts',(1.24772329840508,-25.8997065511409,-7.78897172567729));
#54826=CARTESIAN_POINT('Ctrl Pts',(1.27332169550984,-25.8991031670055,-7.79062629563441));
#54827=CARTESIAN_POINT('Ctrl Pts',(1.37083378686459,-25.8968046930544,-7.79692905655149));
#54828=CARTESIAN_POINT('Ctrl Pts',(1.46834552751268,-25.8942433061664,-7.8039574668929));
#54829=CARTESIAN_POINT('Ctrl Pts',(1.56585687063046,-25.891418310992,-7.81170938496717));
#54830=CARTESIAN_POINT('Ctrl Pts',(1.74018381696231,-25.8863678956618,-7.82556795939445));
#54831=CARTESIAN_POINT('Ctrl Pts',(1.91451114826134,-25.8804759883749,-7.84173976099296));
#54832=CARTESIAN_POINT('Ctrl Pts',(2.08883802674337,-25.8737418647172,-7.86022512769866));
#54833=CARTESIAN_POINT('Ctrl Pts',(2.17524324653938,-25.8704040923677,-7.86938741057279));
#54834=CARTESIAN_POINT('Ctrl Pts',(2.26164833787882,-25.866859375497,-7.87911818625325));
#54835=CARTESIAN_POINT('Ctrl Pts',(2.34805359177775,-25.8631079380462,-7.88941699555171));
#54836=CARTESIAN_POINT('Ctrl Pts',(2.47841969237041,-25.8574478624142,-7.90495558317692));
#54837=CARTESIAN_POINT('Ctrl Pts',(2.60878583208703,-25.8513174296,-7.92178731761465));
#54838=CARTESIAN_POINT('Ctrl Pts',(2.73915198362067,-25.8447165664372,-7.93991205113027));
#54839=CARTESIAN_POINT('Ctrl Pts',(2.77255027453888,-25.8430255021109,-7.94455539693475));
#54840=CARTESIAN_POINT('Ctrl Pts',(2.80594857215923,-25.8413035482865,-7.94928360557479));
#54841=CARTESIAN_POINT('Ctrl Pts',(2.83934685804493,-25.839550699752,-7.95409669970059));
#54842=CARTESIAN_POINT('Ctrl Pts',(2.87113163810415,-25.8378825331479,-7.9586772682578));
#54843=CARTESIAN_POINT('Ctrl Pts',(2.90291640750873,-25.8361863848123,-7.96333471870051));
#54844=CARTESIAN_POINT('Ctrl Pts',(2.93470118226646,-25.8344622612576,-7.9680690215513));
#54845=CARTESIAN_POINT('Ctrl Pts',(2.98358847357107,-25.8318104340509,-7.97535072306892));
#54846=CARTESIAN_POINT('Ctrl Pts',(3.03247576140606,-25.8290924419971,-7.98281424467595));
#54847=CARTESIAN_POINT('Ctrl Pts',(3.08136305166704,-25.8263083279687,-7.99045953951483));
#54848=CARTESIAN_POINT('Ctrl Pts',(3.09765881508736,-25.8253802899592,-7.99300797112779));
#54849=CARTESIAN_POINT('Ctrl Pts',(3.11203760519597,-25.8245558042673,-7.99527206014206));
#54850=CARTESIAN_POINT('Ctrl Pts',(3.13025034275539,-25.8235021734813,-7.99816542476062));
#54851=CARTESIAN_POINT('Ctrl Pts',(3.25877662888247,-25.8160667590396,-8.01858373955937));
#54852=CARTESIAN_POINT('Ctrl Pts',(3.38588318060853,-25.8082995024302,-8.04008654538536));
#54853=CARTESIAN_POINT('Ctrl Pts',(3.51155623329027,-25.8002302720259,-8.06258873711801));
#54854=CARTESIAN_POINT('Ctrl Pts',(3.7138153469081,-25.7872435946569,-8.09880392611186));
#54855=CARTESIAN_POINT('Ctrl Pts',(3.91236064810576,-25.7734753352644,-8.1376067494722));
#54856=CARTESIAN_POINT('Ctrl Pts',(4.10715837540643,-25.7590471476669,-8.1786507566697));
#54857=CARTESIAN_POINT('Ctrl Pts',(4.29250871330393,-25.7453187049201,-8.21770419280647));
#54858=CARTESIAN_POINT('Ctrl Pts',(4.47446644684118,-25.7309927563673,-8.25878685121989));
#54859=CARTESIAN_POINT('Ctrl Pts',(4.65302175618465,-25.7161700471708,-8.30161450758188));
#54860=CARTESIAN_POINT('Ctrl Pts',(4.83066123692135,-25.7014233651795,-8.34422249647499));
#54861=CARTESIAN_POINT('Ctrl Pts',(5.00493325561088,-25.6861850570542,-8.38855772601219));
#54862=CARTESIAN_POINT('Ctrl Pts',(5.17584377090514,-25.6705512675105,-8.43435749453037));
#54863=CARTESIAN_POINT('Ctrl Pts',(5.35321544765739,-25.6543264526676,-8.48188869366663));
#54864=CARTESIAN_POINT('Ctrl Pts',(5.52696673857987,-25.637675856963,-8.53099734398442));
#54865=CARTESIAN_POINT('Ctrl Pts',(5.69711918676562,-25.6207045183267,-8.58141278880069));
#54866=CARTESIAN_POINT('Ctrl Pts',(5.87745056215045,-25.6027179135436,-8.63484420634003));
#54867=CARTESIAN_POINT('Ctrl Pts',(6.05373965417498,-25.5843713774276,-8.6897436347901));
#54868=CARTESIAN_POINT('Ctrl Pts',(6.22602530087962,-25.5657888055731,-8.74582073094045));
#54869=CARTESIAN_POINT('Ctrl Pts',(6.24124677966927,-25.56414703083,-8.7507751560244));
#54870=CARTESIAN_POINT('Ctrl Pts',(6.25643701466447,-25.5625034022857,-8.75573878175259));
#54871=CARTESIAN_POINT('Ctrl Pts',(6.27159604017614,-25.5608580130601,-8.76071143363601));
#54872=CARTESIAN_POINT('Origin',(5.999999999061,-24.7867247845918,-9.33250979146072));
#54873=CARTESIAN_POINT('Origin',(5.99996968604069,-24.7866936472161,-9.33251391760964));
#54874=CARTESIAN_POINT('Ctrl Pts',(6.2381662493015,-15.8434653591368,-3.89871982521923));
#54875=CARTESIAN_POINT('Ctrl Pts',(6.28270685588528,-15.8280466725275,-3.90962901102358));
#54876=CARTESIAN_POINT('Ctrl Pts',(6.4154468492204,-15.7792172453928,-3.95133964265943));
#54877=CARTESIAN_POINT('Ctrl Pts',(6.62496348493694,-15.6869699783287,-4.06531809963326));
#54878=CARTESIAN_POINT('Ctrl Pts',(6.83862806647333,-15.5655783391514,-4.26654921887387));
#54879=CARTESIAN_POINT('Ctrl Pts',(6.99712296257017,-15.442135225343,-4.51768655011421));
#54880=CARTESIAN_POINT('Ctrl Pts',(7.08874537959131,-15.3284821169024,-4.79018566349332));
#54881=CARTESIAN_POINT('Ctrl Pts',(7.11061770868682,-15.2560930725951,-4.99096328383844));
#54882=CARTESIAN_POINT('Ctrl Pts',(7.10961146250444,-15.222090971502,-5.09378162079904));
#54883=CARTESIAN_POINT('Ctrl Pts',(7.10920395886533,-15.2171853595682,-5.10881479487898));
#54884=CARTESIAN_POINT('Ctrl Pts',(6.03906557358641,-15.2264275198782,-3.86392206373007));
#54885=CARTESIAN_POINT('Ctrl Pts',(6.07822367443455,-15.2128353613506,-3.87323986549437));
#54886=CARTESIAN_POINT('Ctrl Pts',(6.19515881189246,-15.1696984985832,-3.90896870950711));
#54887=CARTESIAN_POINT('Ctrl Pts',(6.38078979300515,-15.0877569698194,-4.00735611687519));
#54888=CARTESIAN_POINT('Ctrl Pts',(6.57124098797509,-14.9794788173172,-4.18254724403121));
#54889=CARTESIAN_POINT('Ctrl Pts',(6.71312520739851,-14.8692976146181,-4.40251563354182));
#54890=CARTESIAN_POINT('Ctrl Pts',(6.7952965756176,-14.7681803773293,-4.64199449680407));
#54891=CARTESIAN_POINT('Ctrl Pts',(6.81486950788481,-14.7042676737426,-4.81843665892518));
#54892=CARTESIAN_POINT('Ctrl Pts',(6.81396801300512,-14.6744725826796,-4.90857742684284));
#54893=CARTESIAN_POINT('Ctrl Pts',(6.81360381237917,-14.6701794058539,-4.9217513094863));
#54894=CARTESIAN_POINT('Ctrl Pts',(6.02069930843359,-14.8094597286314,-3.36567359206999));
#54895=CARTESIAN_POINT('Ctrl Pts',(6.07475684431375,-14.7910755618093,-3.3784527664935));
#54896=CARTESIAN_POINT('Ctrl Pts',(6.23519938320304,-14.7332353813749,-3.42721134903272));
#54897=CARTESIAN_POINT('Ctrl Pts',(6.48547730175931,-14.6258688961522,-3.55919023320549));
#54898=CARTESIAN_POINT('Ctrl Pts',(6.73750978253762,-14.4870496263752,-3.78912848623333));
#54899=CARTESIAN_POINT('Ctrl Pts',(6.92276415304904,-14.3475283510534,-4.07325817936266));
#54900=CARTESIAN_POINT('Ctrl Pts',(7.02943302213632,-14.219745403388,-4.37999050482277));
#54901=CARTESIAN_POINT('Ctrl Pts',(7.05501806254693,-14.1381849340581,-4.60629545051647));
#54902=CARTESIAN_POINT('Ctrl Pts',(7.0538438996794,-14.0996506859718,-4.72280681189381));
#54903=CARTESIAN_POINT('Ctrl Pts',(7.05336593073427,-14.0940854822575,-4.73985802582531));
#54904=CARTESIAN_POINT('Ctrl Pts',(6.19651102201121,-14.8792022748334,-2.74314825562037));
#54905=CARTESIAN_POINT('Ctrl Pts',(6.27563796232849,-14.8526593570817,-2.76209401164177));
#54906=CARTESIAN_POINT('Ctrl Pts',(6.50937290672894,-14.7696970350242,-2.83405688006437));
#54907=CARTESIAN_POINT('Ctrl Pts',(6.8689582011957,-14.6184250149389,-3.02602829313312));
#54908=CARTESIAN_POINT('Ctrl Pts',(7.22557715812671,-14.4261278195948,-3.35437471770514));
#54909=CARTESIAN_POINT('Ctrl Pts',(7.48475247284693,-14.2345643866072,-3.75448887950438));
#54910=CARTESIAN_POINT('Ctrl Pts',(7.63324425106608,-14.0589978633,-4.18314620121717));
#54911=CARTESIAN_POINT('Ctrl Pts',(7.66907320432673,-13.9456327396364,-4.49970129815192));
#54912=CARTESIAN_POINT('Ctrl Pts',(7.66743397918277,-13.891339277167,-4.66374917088238));
#54913=CARTESIAN_POINT('Ctrl Pts',(7.6667623725601,-13.8834801583075,-4.68778504726345));
#54914=CARTESIAN_POINT('',(6.999999953679,-14.796797858554,-4.9296888417313));
#54915=CARTESIAN_POINT('',(6.99999996004463,-14.5427407425438,-3.16613273045081));
#54916=CARTESIAN_POINT('Ctrl Pts',(7.,-14.796797858554,-4.9296888417313));
#54917=CARTESIAN_POINT('Ctrl Pts',(7.,-14.754906007383,-4.82443917935157));
#54918=CARTESIAN_POINT('Ctrl Pts',(7.,-14.7198932163359,-4.72994340387162));
#54919=CARTESIAN_POINT('Ctrl Pts',(7.,-14.692006860887,-4.64804677830323));
#54920=CARTESIAN_POINT('Ctrl Pts',(7.,-14.6780636831625,-4.60709846551903));
#54921=CARTESIAN_POINT('Ctrl Pts',(7.,-14.6658488264905,-4.56931600454163));
#54922=CARTESIAN_POINT('Ctrl Pts',(7.,-14.655164565243,-4.53496157999509));
#54923=CARTESIAN_POINT('Ctrl Pts',(7.,-14.6498224346192,-4.51778436772182));
#54924=CARTESIAN_POINT('Ctrl Pts',(7.,-14.6448613847077,-4.50146376159314));
#54925=CARTESIAN_POINT('Ctrl Pts',(7.,-14.6402500967837,-4.48603013365108));
#54926=CARTESIAN_POINT('Ctrl Pts',(7.,-14.6379444528216,-4.47831331968006));
#54927=CARTESIAN_POINT('Ctrl Pts',(7.,-14.6357262493564,-4.47081825025569));
#54928=CARTESIAN_POINT('Ctrl Pts',(7.,-14.6335913344904,-4.46354849404081));
#54929=CARTESIAN_POINT('Ctrl Pts',(7.,-14.6325238770573,-4.45991361593337));
#54930=CARTESIAN_POINT('Ctrl Pts',(7.,-14.6314772417741,-4.4563350661283));
#54931=CARTESIAN_POINT('Ctrl Pts',(7.,-14.6304509145204,-4.45281327894708));
#54932=CARTESIAN_POINT('Ctrl Pts',(7.,-14.6294245872668,-4.44929149176586));
#54933=CARTESIAN_POINT('Ctrl Pts',(7.,-14.6289298517031,-4.44759316899773));
#54934=CARTESIAN_POINT('Ctrl Pts',(7.,-14.6274323416498,-4.4424186347167));
#54935=CARTESIAN_POINT('Ctrl Pts',(7.,-14.6034721807969,-4.35962608622025));
#54936=CARTESIAN_POINT('Ctrl Pts',(7.,-14.5830070402295,-4.27937186692289));
#54937=CARTESIAN_POINT('Ctrl Pts',(7.,-14.5661203115116,-4.20227971847956));
#54938=CARTESIAN_POINT('Ctrl Pts',(7.,-14.5492335827938,-4.12518757003624));
#54939=CARTESIAN_POINT('Ctrl Pts',(7.,-14.5361411909217,-4.05283234742234));
#54940=CARTESIAN_POINT('Ctrl Pts',(7.,-14.525657599663,-3.98131352903846));
#54941=CARTESIAN_POINT('Ctrl Pts',(7.,-14.5046904171456,-3.83827589227071));
#54942=CARTESIAN_POINT('Ctrl Pts',(7.,-14.4945119231233,-3.69577454270348));
#54943=CARTESIAN_POINT('Ctrl Pts',(7.,-14.4973995817608,-3.55814511608832));
#54944=CARTESIAN_POINT('Ctrl Pts',(7.,-14.5002872403983,-3.42051568947317));
#54945=CARTESIAN_POINT('Ctrl Pts',(7.,-14.5162103430636,-3.28798606398169));
#54946=CARTESIAN_POINT('Ctrl Pts',(7.,-14.5427407867182,-3.16613306625888));
#54947=CARTESIAN_POINT('',(6.24994468128209,-14.8593881421341,-2.7654624279623));
#54948=CARTESIAN_POINT('Ctrl Pts',(6.24994466999289,-14.8593881037488,-2.76546242081725));
#54949=CARTESIAN_POINT('Ctrl Pts',(6.29949253242022,-14.8423128454431,-2.77890846415222));
#54950=CARTESIAN_POINT('Ctrl Pts',(6.34809291873447,-14.8249522944953,-2.79423376364713));
#54951=CARTESIAN_POINT('Ctrl Pts',(6.39576306624784,-14.8073119088175,-2.81137470270461));
#54952=CARTESIAN_POINT('Ctrl Pts',(6.40561146986023,-14.8036674972288,-2.81491593122894));
#54953=CARTESIAN_POINT('Ctrl Pts',(6.4154201217803,-14.8000111072706,-2.81853482140992));
#54954=CARTESIAN_POINT('Ctrl Pts',(6.42518909072932,-14.7963427361861,-2.82223106921286));
#54955=CARTESIAN_POINT('Ctrl Pts',(6.47313505804959,-14.778338420577,-2.84037220337882));
#54956=CARTESIAN_POINT('Ctrl Pts',(6.52012706823349,-14.7600460751789,-2.86037304645751));
#54957=CARTESIAN_POINT('Ctrl Pts',(6.56619556493753,-14.7414556825689,-2.88220221975805));
#54958=CARTESIAN_POINT('Ctrl Pts',(6.59344693697557,-14.7304587162775,-2.89511505532804));
#54959=CARTESIAN_POINT('Ctrl Pts',(6.62037471767466,-14.7193573113327,-2.90866855706025));
#54960=CARTESIAN_POINT('Ctrl Pts',(6.64698065073811,-14.7081484355682,-2.92286341778547));
#54961=CARTESIAN_POINT('Ctrl Pts',(6.69272061293139,-14.6888785399223,-2.94726671126749));
#54962=CARTESIAN_POINT('Ctrl Pts',(6.73750177898171,-14.6692956536967,-2.9735559602869));
#54963=CARTESIAN_POINT('Ctrl Pts',(6.78129414167393,-14.6493873062218,-3.00175771322334));
#54964=CARTESIAN_POINT('Ctrl Pts',(6.80384852332261,-14.6391339095257,-3.01628246274099));
#54965=CARTESIAN_POINT('Ctrl Pts',(6.82614003401257,-14.6287941458886,-3.03131510454672));
#54966=CARTESIAN_POINT('Ctrl Pts',(6.84816042293265,-14.6183662324647,-3.04686275341766));
#54967=CARTESIAN_POINT('Ctrl Pts',(6.89066022810777,-14.5982401442968,-3.07687003668339));
#54968=CARTESIAN_POINT('Ctrl Pts',(6.93215285126177,-14.5777855466898,-3.10879426210764));
#54969=CARTESIAN_POINT('Ctrl Pts',(6.97258071543327,-14.5569859365848,-3.14269338952529));
#54970=CARTESIAN_POINT('Ctrl Pts',(6.98177604604753,-14.5522550586252,-3.15040375688028));
#54971=CARTESIAN_POINT('Ctrl Pts',(6.99091610578742,-14.5475063422576,-3.15821639324445));
#54972=CARTESIAN_POINT('Ctrl Pts',(6.99999987588419,-14.5427396158966,-3.1661321485828));
#54973=CARTESIAN_POINT('',(6.26386081962776,-15.8144408557884,-3.90572621562457));
#54974=CARTESIAN_POINT('Ctrl Pts',(6.26385680272581,-15.8144410175731,-3.90574090061969));
#54975=CARTESIAN_POINT('Ctrl Pts',(6.25434739267814,-15.785035322926,-3.90346327992607));
#54976=CARTESIAN_POINT('Ctrl Pts',(6.24501465448848,-15.7550032667797,-3.89974567582242));
#54977=CARTESIAN_POINT('Ctrl Pts',(6.23596151625569,-15.724517427388,-3.89443848692829));
#54978=CARTESIAN_POINT('Ctrl Pts',(6.22713568305973,-15.6947970225525,-3.88926455025411));
#54979=CARTESIAN_POINT('Ctrl Pts',(6.21857587660778,-15.6646456440639,-3.88257916996334));
#54980=CARTESIAN_POINT('Ctrl Pts',(6.21038339038277,-15.6342633509603,-3.87427169593729));
#54981=CARTESIAN_POINT('Ctrl Pts',(6.20231719059348,-15.6043493981626,-3.86609228087353));
#54982=CARTESIAN_POINT('Ctrl Pts',(6.1946073963697,-15.5742120457398,-3.85633977680809));
#54983=CARTESIAN_POINT('Ctrl Pts',(6.18735199987957,-15.5440761704759,-3.8449456613132));
#54984=CARTESIAN_POINT('Ctrl Pts',(6.18022409990826,-15.5144698622994,-3.83375177058379));
#54985=CARTESIAN_POINT('Ctrl Pts',(6.17353510231177,-15.4848656159052,-3.82097302339114));
#54986=CARTESIAN_POINT('Ctrl Pts',(6.16737434330549,-15.4555016018223,-3.80658826970777));
#54987=CARTESIAN_POINT('Ctrl Pts',(6.16657568470721,-15.451694956845,-3.80472348207339));
#54988=CARTESIAN_POINT('Ctrl Pts',(6.16578589435225,-15.4478923758297,-3.8028317707424));
#54989=CARTESIAN_POINT('Ctrl Pts',(6.16500515775714,-15.444094399648,-3.80091314997598));
#54990=CARTESIAN_POINT('Ctrl Pts',(6.15907432331299,-15.4152432248763,-3.78633842375209));
#54991=CARTESIAN_POINT('Ctrl Pts',(6.15366693892629,-15.3866570736564,-3.77020678733933));
#54992=CARTESIAN_POINT('Ctrl Pts',(6.14885762209861,-15.3585789395669,-3.75255219896567));
#54993=CARTESIAN_POINT('Ctrl Pts',(6.1441072471592,-15.3308449246739,-3.73511398119362));
#54994=CARTESIAN_POINT('Ctrl Pts',(6.13994064449411,-15.3036073583595,-3.71618992922669));
#54995=CARTESIAN_POINT('Ctrl Pts',(6.1364164212586,-15.2771013424223,-3.695861834686));
#54996=CARTESIAN_POINT('Ctrl Pts',(6.1329126344815,-15.2507490310199,-3.67565161981157));
#54997=CARTESIAN_POINT('Ctrl Pts',(6.13004401913192,-15.225120618436,-3.65405381053664));
#54998=CARTESIAN_POINT('Ctrl Pts',(6.1278512193941,-15.2004359938299,-3.63119595624287));
#54999=CARTESIAN_POINT('Ctrl Pts',(6.12566730832878,-15.1758514301367,-3.60843075791641));
#55000=CARTESIAN_POINT('Ctrl Pts',(6.12415388155219,-15.1522037620878,-3.58441614318941));
#55001=CARTESIAN_POINT('Ctrl Pts',(6.12333154166847,-15.1296874723247,-3.55932021761716));
#55002=CARTESIAN_POINT('Ctrl Pts',(6.12302921506252,-15.1214095405384,-3.55009390359353));
#55003=CARTESIAN_POINT('Ctrl Pts',(6.1228200957212,-15.1132842492035,-3.54072181573136));
#55004=CARTESIAN_POINT('Ctrl Pts',(6.12270449763779,-15.1053201949041,-3.53121353501667));
#55005=CARTESIAN_POINT('Ctrl Pts',(6.12239025057169,-15.0836703489532,-3.50536579403046));
#55006=CARTESIAN_POINT('Ctrl Pts',(6.12276865950795,-15.0632149366601,-3.47850974789018));
#55007=CARTESIAN_POINT('Ctrl Pts',(6.12383157496324,-15.044100649971,-3.45085760590152));
#55008=CARTESIAN_POINT('Ctrl Pts',(6.12490061466795,-15.0248762316071,-3.42304613928017));
#55009=CARTESIAN_POINT('Ctrl Pts',(6.12666199158116,-15.0070088394718,-3.39443016446765));
#55010=CARTESIAN_POINT('Ctrl Pts',(6.12908657998587,-14.9906035321586,-3.36524562850755));
#55011=CARTESIAN_POINT('Ctrl Pts',(6.13152236548042,-14.9741224628318,-3.33592631426071));
#55012=CARTESIAN_POINT('Ctrl Pts',(6.13462731787943,-14.9591171667997,-3.30603402985629));
#55013=CARTESIAN_POINT('Ctrl Pts',(6.1383529517025,-14.945645493166,-3.27581569596834));
#55014=CARTESIAN_POINT('Ctrl Pts',(6.14212000873812,-14.9320240356226,-3.24526138153937));
#55015=CARTESIAN_POINT('Ctrl Pts',(6.14652137385283,-14.9199704463401,-3.2143745768921));
#55016=CARTESIAN_POINT('Ctrl Pts',(6.15149089059401,-14.9094939790091,-3.18340537369647));
#55017=CARTESIAN_POINT('Ctrl Pts',(6.15328515498051,-14.9057114075424,-3.17222381595833));
#55018=CARTESIAN_POINT('Ctrl Pts',(6.15515335276949,-14.902133962306,-3.16103140626657));
#55019=CARTESIAN_POINT('Ctrl Pts',(6.15709197107948,-14.8987605391209,-3.14983943667008));
#55020=CARTESIAN_POINT('Ctrl Pts',(6.1625485231329,-14.8892654987031,-3.11833784382476));
#55021=CARTESIAN_POINT('Ctrl Pts',(6.1685631653214,-14.8813901398998,-3.08684159759775));
#55022=CARTESIAN_POINT('Ctrl Pts',(6.17504972278387,-14.8750788685375,-3.05558574897629));
#55023=CARTESIAN_POINT('Ctrl Pts',(6.18168467070373,-14.8686232166698,-3.02361487243744));
#55024=CARTESIAN_POINT('Ctrl Pts',(6.18881302060891,-14.8638035249704,-2.99189615705139));
#55025=CARTESIAN_POINT('Ctrl Pts',(6.19633675700028,-14.8605176411598,-2.96064760775454));
#55026=CARTESIAN_POINT('Ctrl Pts',(6.20397194257905,-14.8571830835174,-2.92893617336372));
#55027=CARTESIAN_POINT('Ctrl Pts',(6.21201396047443,-14.8554273949708,-2.89770931890753));
#55028=CARTESIAN_POINT('Ctrl Pts',(6.22035994366165,-14.8551099062963,-2.86715290245178));
#55029=CARTESIAN_POINT('Ctrl Pts',(6.22890611290103,-14.8547848023651,-2.83586356235581));
#55030=CARTESIAN_POINT('Ctrl Pts',(6.23777067522327,-14.8559669469053,-2.80527742314284));
#55031=CARTESIAN_POINT('Ctrl Pts',(6.2468480287175,-14.8584814517712,-2.77554561910762));
#55032=CARTESIAN_POINT('Ctrl Pts',(6.24787754648693,-14.8587666370339,-2.77217355470682));
#55033=CARTESIAN_POINT('Ctrl Pts',(6.24890980941479,-14.8590689433739,-2.76881242822435));
#55034=CARTESIAN_POINT('Ctrl Pts',(6.24994466999289,-14.8593881037488,-2.76546242081725));
#55035=CARTESIAN_POINT('Ctrl Pts',(6.26385680289834,-15.8144410175599,-3.90574090066702));
#55036=CARTESIAN_POINT('Ctrl Pts',(6.29464231014065,-15.7946386727068,-3.91437791970859));
#55037=CARTESIAN_POINT('Ctrl Pts',(6.32519901986354,-15.7740985767096,-3.92458862745004));
#55038=CARTESIAN_POINT('Ctrl Pts',(6.35535969010304,-15.7528444265997,-3.93639986371284));
#55039=CARTESIAN_POINT('Ctrl Pts',(6.39985352172865,-15.7214897329266,-3.95382411700011));
#55040=CARTESIAN_POINT('Ctrl Pts',(6.44348728197708,-15.6885800104884,-3.97473232893006));
#55041=CARTESIAN_POINT('Ctrl Pts',(6.48575810107706,-15.6542249774097,-3.9990727963858));
#55042=CARTESIAN_POINT('Ctrl Pts',(6.51303557488992,-15.6320555817108,-4.01477976582129));
#55043=CARTESIAN_POINT('Ctrl Pts',(6.53974464965851,-15.6092847175838,-4.03191581203157));
#55044=CARTESIAN_POINT('Ctrl Pts',(6.56573941608896,-15.5859462401836,-4.05046724920638));
#55045=CARTESIAN_POINT('Ctrl Pts',(6.56926098315705,-15.5827845263189,-4.05298045240809));
#55046=CARTESIAN_POINT('Ctrl Pts',(6.57276942762224,-15.5796124004499,-4.05551963423667));
#55047=CARTESIAN_POINT('Ctrl Pts',(6.57626437337287,-15.5764299517938,-4.05808476273979));
#55048=CARTESIAN_POINT('Ctrl Pts',(6.61460947149103,-15.5415134424451,-4.08622829089611));
#55049=CARTESIAN_POINT('Ctrl Pts',(6.65133308425788,-15.5053526401255,-4.11749543403956));
#55050=CARTESIAN_POINT('Ctrl Pts',(6.68600408697268,-15.4680864724447,-4.15172691181702));
#55051=CARTESIAN_POINT('Ctrl Pts',(6.7111562078007,-15.4410516860551,-4.17656017874796));
#55052=CARTESIAN_POINT('Ctrl Pts',(6.73522739077866,-15.4134355611798,-4.20295334288734));
#55053=CARTESIAN_POINT('Ctrl Pts',(6.75803716642575,-15.3852981854079,-4.23084617397227));
#55054=CARTESIAN_POINT('Ctrl Pts',(6.75931380622222,-15.3837233652854,-4.23240730717894));
#55055=CARTESIAN_POINT('Ctrl Pts',(6.76058649060395,-15.3821469139671,-4.23397313859397));
#55056=CARTESIAN_POINT('Ctrl Pts',(6.76185518645526,-15.3805688425827,-4.23554365783243));
#55057=CARTESIAN_POINT('Ctrl Pts',(6.7700468794139,-15.3703795791482,-4.24568415870487));
#55058=CARTESIAN_POINT('Ctrl Pts',(6.77807230818569,-15.3601227655933,-4.25602009707487));
#55059=CARTESIAN_POINT('Ctrl Pts',(6.78592456218493,-15.3498016129747,-4.26654660476092));
#55060=CARTESIAN_POINT('Ctrl Pts',(6.79045875165238,-15.3438417877449,-4.27262500980026));
#55061=CARTESIAN_POINT('Ctrl Pts',(6.79493519828708,-15.3378605072598,-4.27876696178125));
#55062=CARTESIAN_POINT('Ctrl Pts',(6.79935253216999,-15.3318584131363,-4.28497151510868));
#55063=CARTESIAN_POINT('Ctrl Pts',(6.80156119911144,-15.3288573660746,-4.28807379177239));
#55064=CARTESIAN_POINT('Ctrl Pts',(6.8037550875957,-15.3258511156132,-4.29119171892957));
#55065=CARTESIAN_POINT('Ctrl Pts',(6.80593402451752,-15.3228397423737,-4.2943251791777));
#55066=CARTESIAN_POINT('Ctrl Pts',(6.80759005980613,-15.3205510389688,-4.29670667113113));
#55067=CARTESIAN_POINT('Ctrl Pts',(6.80965642237721,-15.3176739784075,-4.29970838286095));
#55068=CARTESIAN_POINT('Ctrl Pts',(6.81117695486563,-15.3155432926217,-4.30193722155344));
#55069=CARTESIAN_POINT('Ctrl Pts',(6.81165707079494,-15.3148705176603,-4.30264098879832));
#55070=CARTESIAN_POINT('Ctrl Pts',(6.81208312885854,-15.3142721780336,-4.30326741588872));
#55071=CARTESIAN_POINT('Ctrl Pts',(6.81242580594044,-15.3137903355188,-4.3037720420517));
#55072=CARTESIAN_POINT('Ctrl Pts',(6.82705299909326,-15.2932228569605,-4.32531204208564));
#55073=CARTESIAN_POINT('Ctrl Pts',(6.84166190719415,-15.2714248648976,-4.34856896054824));
#55074=CARTESIAN_POINT('Ctrl Pts',(6.85595717412585,-15.2484182524569,-4.373666513424));
#55075=CARTESIAN_POINT('Ctrl Pts',(6.86936271662908,-15.2268435506759,-4.3972020174066));
#55076=CARTESIAN_POINT('Ctrl Pts',(6.88249251343736,-15.2042058902949,-4.42235627841688));
#55077=CARTESIAN_POINT('Ctrl Pts',(6.89505966326525,-15.1805403619258,-4.44921795667627));
#55078=CARTESIAN_POINT('Ctrl Pts',(6.89589374366113,-15.1789696833279,-4.45100076340202));
#55079=CARTESIAN_POINT('Ctrl Pts',(6.89672532848846,-15.1773944839582,-4.45279108572735));
#55080=CARTESIAN_POINT('Ctrl Pts',(6.89755432638955,-15.1758147771217,-4.45458894715883));
#55081=CARTESIAN_POINT('Ctrl Pts',(6.90969329051585,-15.1526832292701,-4.48091491902407));
#55082=CARTESIAN_POINT('Ctrl Pts',(6.92128063254415,-15.1285834265236,-4.50885955213998));
#55083=CARTESIAN_POINT('Ctrl Pts',(6.93203465924816,-15.103570623826,-4.53846268874816));
#55084=CARTESIAN_POINT('Ctrl Pts',(6.93454271509536,-15.0977371339354,-4.54536673705574));
#55085=CARTESIAN_POINT('Ctrl Pts',(6.93700528186122,-15.0918540797584,-4.55236087968532));
#55086=CARTESIAN_POINT('Ctrl Pts',(6.93941847433871,-15.0859223430359,-4.55944540688696));
#55087=CARTESIAN_POINT('Ctrl Pts',(6.94912526570966,-15.062062608941,-4.58794210913917));
#55088=CARTESIAN_POINT('Ctrl Pts',(6.95803613112938,-15.0374135620583,-4.61790307748903));
#55089=CARTESIAN_POINT('Ctrl Pts',(6.96587583092441,-15.0120452933159,-4.64933257084334));
#55090=CARTESIAN_POINT('Ctrl Pts',(6.9693799351623,-15.0007064588793,-4.66338058591238));
#55091=CARTESIAN_POINT('Ctrl Pts',(6.97266954009498,-14.9892242191139,-4.67772166388442));
#55092=CARTESIAN_POINT('Ctrl Pts',(6.97571741922449,-14.9776062938991,-4.69235455327343));
#55093=CARTESIAN_POINT('Ctrl Pts',(6.98225036636205,-14.9527039640981,-4.72371927896829));
#55094=CARTESIAN_POINT('Ctrl Pts',(6.98767463465472,-14.9271766313242,-4.75642696399957));
#55095=CARTESIAN_POINT('Ctrl Pts',(6.99173368562324,-14.901120484089,-4.79041861766872));
#55096=CARTESIAN_POINT('Ctrl Pts',(6.99559723923891,-14.8763192872967,-4.82277312059423));
#55097=CARTESIAN_POINT('Ctrl Pts',(6.99822422923869,-14.851038940224,-4.85629082491783));
#55098=CARTESIAN_POINT('Ctrl Pts',(6.99936263918771,-14.8253844806674,-4.89089220479161));
#55099=CARTESIAN_POINT('Ctrl Pts',(6.99968896476072,-14.8180306216972,-4.90081070130889));
#55100=CARTESIAN_POINT('Ctrl Pts',(6.99989275741611,-14.8106461698658,-4.91081805718665));
#55101=CARTESIAN_POINT('Ctrl Pts',(6.99996751968053,-14.8032339673454,-4.92091194510101));
#55102=CARTESIAN_POINT('Ctrl Pts',(6.99998913554391,-14.8010908921153,-4.9238303706439));
#55103=CARTESIAN_POINT('Ctrl Pts',(6.99999996330327,-14.7989454981677,-4.92675602852862));
#55104=CARTESIAN_POINT('Ctrl Pts',(6.99999987085796,-14.7967978585547,-4.92968884172919));
#55105=CARTESIAN_POINT('Ctrl Pts',(6.99990204847876,-14.6847053727042,-4.95612542422809));
#55106=CARTESIAN_POINT('Ctrl Pts',(6.99990204847876,-15.0109966856309,-4.91843511379028));
#55107=CARTESIAN_POINT('Ctrl Pts',(6.99990204847876,-15.8988773644907,-4.8561641130756));
#55108=CARTESIAN_POINT('Ctrl Pts',(6.99990204847876,-17.3517264997127,-4.93000583026503));
#55109=CARTESIAN_POINT('Ctrl Pts',(6.99990204847876,-19.0057036593414,-5.27370352517816));
#55110=CARTESIAN_POINT('Ctrl Pts',(6.99990204847876,-20.5902612526977,-5.86661657541822));
#55111=CARTESIAN_POINT('Ctrl Pts',(6.99990204847876,-22.0651320115504,-6.69609676488873));
#55112=CARTESIAN_POINT('Ctrl Pts',(6.99990204847876,-23.3944663504207,-7.73957935185531));
#55113=CARTESIAN_POINT('Ctrl Pts',(6.99990204847876,-24.2870419231056,-8.69530609464369));
#55114=CARTESIAN_POINT('Ctrl Pts',(6.99990204847876,-24.7366373563668,-9.28612088063576));
#55115=CARTESIAN_POINT('Ctrl Pts',(6.99990204847876,-24.8428462632706,-9.43308828770487));
#55116=CARTESIAN_POINT('Ctrl Pts',(7.00659078506582,-14.6298576689916,-4.48143047120262));
#55117=CARTESIAN_POINT('Ctrl Pts',(7.00659078506582,-14.9704072356705,-4.44209164486882));
#55118=CARTESIAN_POINT('Ctrl Pts',(7.00659078506582,-15.8968485520861,-4.37713026806021));
#55119=CARTESIAN_POINT('Ctrl Pts',(7.00659078506582,-17.4127173390504,-4.45416586533225));
#55120=CARTESIAN_POINT('Ctrl Pts',(7.00659078506582,-19.1390748339291,-4.81286872482972));
#55121=CARTESIAN_POINT('Ctrl Pts',(7.00659078506582,-20.792516687395,-5.43161542968116));
#55122=CARTESIAN_POINT('Ctrl Pts',(7.00659078506582,-22.3315011340853,-6.29709341005203));
#55123=CARTESIAN_POINT('Ctrl Pts',(7.00659078506582,-23.7189804924501,-7.38626117312299));
#55124=CARTESIAN_POINT('Ctrl Pts',(7.00659078506582,-24.6502122945406,-8.38339439103266));
#55125=CARTESIAN_POINT('Ctrl Pts',(7.00659078506582,-25.1193210874972,-8.99983838783685));
#55126=CARTESIAN_POINT('Ctrl Pts',(7.00659078506582,-25.2301483657287,-9.15319520571074));
#55127=CARTESIAN_POINT('Ctrl Pts',(6.71769910521849,-14.5861379424571,-4.10304574168264));
#55128=CARTESIAN_POINT('Ctrl Pts',(6.71769910521849,-14.9380529248673,-4.06239286463224));
#55129=CARTESIAN_POINT('Ctrl Pts',(6.71769910521849,-15.8952313627117,-3.99528695853561));
#55130=CARTESIAN_POINT('Ctrl Pts',(6.71769910521849,-17.4613338286547,-4.07486843383928));
#55131=CARTESIAN_POINT('Ctrl Pts',(6.71769910521849,-19.2453865094556,-4.44553208016281));
#55132=CARTESIAN_POINT('Ctrl Pts',(6.71769910521849,-20.9537367877186,-5.0848710840269));
#55133=CARTESIAN_POINT('Ctrl Pts',(6.71769910521849,-22.5438269819634,-5.97904331169807));
#55134=CARTESIAN_POINT('Ctrl Pts',(6.71769910521849,-23.9776543946596,-7.10462724665685));
#55135=CARTESIAN_POINT('Ctrl Pts',(6.71769910521849,-24.9396995155246,-8.13476603538479));
#55136=CARTESIAN_POINT('Ctrl Pts',(6.71769910521849,-25.424362628746,-8.77163936672992));
#55137=CARTESIAN_POINT('Ctrl Pts',(6.71769910521849,-25.5388712631324,-8.93008925640513));
#55138=CARTESIAN_POINT('Ctrl Pts',(6.25532321980198,-14.5721230213941,-3.98174964636385));
#55139=CARTESIAN_POINT('Ctrl Pts',(6.25532321980198,-14.9276813340999,-3.94067553344174));
#55140=CARTESIAN_POINT('Ctrl Pts',(6.25532321980198,-15.8947129518397,-3.87288217087801));
#55141=CARTESIAN_POINT('Ctrl Pts',(6.25532321980198,-17.4769184701448,-3.95327976015244));
#55142=CARTESIAN_POINT('Ctrl Pts',(6.25532321980198,-19.2794660854095,-4.32777759064623));
#55143=CARTESIAN_POINT('Ctrl Pts',(6.25532321980198,-21.0054179659765,-4.97371772100629));
#55144=CARTESIAN_POINT('Ctrl Pts',(6.25532321980198,-22.6118907653904,-5.87708825897841));
#55145=CARTESIAN_POINT('Ctrl Pts',(6.25532321980198,-24.0605756434636,-7.01434586655842));
#55146=CARTESIAN_POINT('Ctrl Pts',(6.25532321980198,-25.0324983702633,-8.05506501583201));
#55147=CARTESIAN_POINT('Ctrl Pts',(6.25532321980198,-25.5221476210515,-8.69848723331493));
#55148=CARTESIAN_POINT('Ctrl Pts',(6.25532321980198,-25.6378363615289,-8.85856977270761));
#55149=CARTESIAN_POINT('Ctrl Pts',(7.0000000000004,-14.796797858554,-4.92968884173129));
#55150=CARTESIAN_POINT('Ctrl Pts',(7.0000000000004,-14.9621718211134,-4.91233286861492));
#55151=CARTESIAN_POINT('Ctrl Pts',(6.99999999998289,-15.1274388227087,-4.89876704773387));
#55152=CARTESIAN_POINT('Ctrl Pts',(6.9999999993942,-15.2926819700917,-4.88893416787038));
#55153=CARTESIAN_POINT('Ctrl Pts',(6.99999999894932,-15.4175591375174,-4.88150328674497));
#55154=CARTESIAN_POINT('Ctrl Pts',(6.99999999821322,-15.5424229437211,-4.87620540119634));
#55155=CARTESIAN_POINT('Ctrl Pts',(6.99999999796755,-15.6673108058121,-4.87303547957403));
#55156=CARTESIAN_POINT('Ctrl Pts',(6.99999999764153,-15.8330446050339,-4.86882880051888));
#55157=CARTESIAN_POINT('Ctrl Pts',(6.99999999919545,-15.9988211310191,-4.86836780068467));
#55158=CARTESIAN_POINT('Ctrl Pts',(6.99999999987699,-16.1647597219873,-4.87168759212841));
#55159=CARTESIAN_POINT('Ctrl Pts',(6.99999999995264,-16.1831793000345,-4.87205609687008));
#55160=CARTESIAN_POINT('Ctrl Pts',(7.00000000000042,-16.2016008696669,-4.87247123934923));
#55161=CARTESIAN_POINT('Ctrl Pts',(7.00000000000042,-16.2200245895141,-4.87293310700196));
#55162=CARTESIAN_POINT('Ctrl Pts',(7.00000000000042,-16.4234357726081,-4.87803245970895));
#55163=CARTESIAN_POINT('Ctrl Pts',(6.99999999555751,-16.6270899052425,-4.8887471286057));
#55164=CARTESIAN_POINT('Ctrl Pts',(6.99999999493389,-16.8304432106282,-4.90512255000003));
#55165=CARTESIAN_POINT('Ctrl Pts',(6.99999999440532,-17.0028030857336,-4.91900216499311));
#55166=CARTESIAN_POINT('Ctrl Pts',(6.99999999611259,-17.1749465731231,-4.93694763771438));
#55167=CARTESIAN_POINT('Ctrl Pts',(6.99999999794676,-17.3465425019982,-4.95895729935852));
#55168=CARTESIAN_POINT('Ctrl Pts',(6.99999999900155,-17.4452234773389,-4.9716145628041));
#55169=CARTESIAN_POINT('Ctrl Pts',(7.00000000000042,-17.5437233863106,-4.9856154106428));
#55170=CARTESIAN_POINT('Ctrl Pts',(7.00000000000042,-17.6419802648722,-5.00094556168401));
#55171=CARTESIAN_POINT('Ctrl Pts',(7.00000000000042,-17.9008409010356,-5.04133329543972));
#55172=CARTESIAN_POINT('Ctrl Pts',(6.99999999747738,-18.158010911339,-5.09103787417142));
#55173=CARTESIAN_POINT('Ctrl Pts',(6.99999999839647,-18.4130245932067,-5.14984752267489));
#55174=CARTESIAN_POINT('Ctrl Pts',(6.99999999910283,-18.6090113775211,-5.19504475998561));
#55175=CARTESIAN_POINT('Ctrl Pts',(6.99999999994416,-18.8037248579095,-5.2456209122658));
#55176=CARTESIAN_POINT('Ctrl Pts',(6.99999999999558,-18.9969550950569,-5.30150070689851));
#55177=CARTESIAN_POINT('Ctrl Pts',(6.99999999999892,-19.0094781659271,-5.30512222410372));
#55178=CARTESIAN_POINT('Ctrl Pts',(7.00000000000042,-19.0219950067074,-5.30876602405832));
#55179=CARTESIAN_POINT('Ctrl Pts',(7.00000000000042,-19.0345055606664,-5.3124320838912));
#55180=CARTESIAN_POINT('Ctrl Pts',(7.00000000000042,-19.37829694462,-5.41317580696964));
#55181=CARTESIAN_POINT('Ctrl Pts',(7.00000000000848,-19.717337955919,-5.53070296422703));
#55182=CARTESIAN_POINT('Ctrl Pts',(6.99999999997893,-20.0498647476411,-5.66455067298009));
#55183=CARTESIAN_POINT('Ctrl Pts',(6.99999999996922,-20.159096338497,-5.70851825250593));
#55184=CARTESIAN_POINT('Ctrl Pts',(7.00000000000042,-20.2676248241435,-5.75424653186144));
#55185=CARTESIAN_POINT('Ctrl Pts',(7.00000000000042,-20.3753872113398,-5.80171797264263));
#55186=CARTESIAN_POINT('Ctrl Pts',(7.00000000000042,-20.4431561669975,-5.83157152404412));
#55187=CARTESIAN_POINT('Ctrl Pts',(6.99999999997258,-20.5106234743014,-5.86211220561406));
#55188=CARTESIAN_POINT('Ctrl Pts',(6.99999999993318,-20.5777739523651,-5.89333485504115));
#55189=CARTESIAN_POINT('Ctrl Pts',(6.99999999971921,-20.9424626713701,-6.06290249404886));
#55190=CARTESIAN_POINT('Ctrl Pts',(7.00000000000042,-21.2978034884988,-6.25258824524381));
#55191=CARTESIAN_POINT('Ctrl Pts',(7.00000000000042,-21.6416259231186,-6.46100648199057));
#55192=CARTESIAN_POINT('Ctrl Pts',(7.00000000000042,-21.7794446663838,-6.54454942907526));
#55193=CARTESIAN_POINT('Ctrl Pts',(6.99999999962401,-21.9154122185717,-6.63110373594479));
#55194=CARTESIAN_POINT('Ctrl Pts',(6.9999999991279,-22.0494161776191,-6.72060846296995));
#55195=CARTESIAN_POINT('Ctrl Pts',(6.99999999825563,-22.2850230329977,-6.87797640512509));
#55196=CARTESIAN_POINT('Ctrl Pts',(6.99999999886891,-22.51456232569,-7.04446337791262));
#55197=CARTESIAN_POINT('Ctrl Pts',(6.99999999982076,-22.7374335824926,-7.21972686077438));
#55198=CARTESIAN_POINT('Ctrl Pts',(6.99999999992681,-22.7622653187281,-7.23925426256033));
#55199=CARTESIAN_POINT('Ctrl Pts',(7.00000000000042,-22.7870142347845,-7.25889064419841));
#55200=CARTESIAN_POINT('Ctrl Pts',(7.00000000000042,-22.8116794661682,-7.27863555348144));
#55201=CARTESIAN_POINT('Ctrl Pts',(7.00000000000042,-22.9843713301579,-7.41687813208722));
#55202=CARTESIAN_POINT('Ctrl Pts',(6.99999999634688,-23.1529951472481,-7.56040930321861));
#55203=CARTESIAN_POINT('Ctrl Pts',(6.99999999542238,-23.3170682079529,-7.70885139832025));
#55204=CARTESIAN_POINT('Ctrl Pts',(6.9999999953121,-23.3366383426619,-7.7265571190836));
#55205=CARTESIAN_POINT('Ctrl Pts',(6.9999999952367,-23.3561437763943,-7.74433266391942));
#55206=CARTESIAN_POINT('Ctrl Pts',(6.99999999520118,-23.3755837254306,-7.76217735716987));
#55207=CARTESIAN_POINT('Ctrl Pts',(6.9999999948931,-23.5442002619243,-7.91695710299456));
#55208=CARTESIAN_POINT('Ctrl Pts',(7.00000000000042,-23.7078863139086,-8.07694208893929));
#55209=CARTESIAN_POINT('Ctrl Pts',(7.00000000000042,-23.8662409010678,-8.24158764729914));
#55210=CARTESIAN_POINT('Ctrl Pts',(7.00000000000042,-23.9842449793353,-8.36427968738245));
#55211=CARTESIAN_POINT('Ctrl Pts',(6.99999999741473,-24.0992427801723,-8.48959370330393));
#55212=CARTESIAN_POINT('Ctrl Pts',(6.99999999745776,-24.2113303506499,-8.61757573537637));
#55213=CARTESIAN_POINT('Ctrl Pts',(6.99999999749883,-24.3183213987655,-8.73973853802289));
#55214=CARTESIAN_POINT('Ctrl Pts',(6.99999999865173,-24.4226608384595,-8.86433273762792));
#55215=CARTESIAN_POINT('Ctrl Pts',(6.99999999924105,-24.5244006140281,-8.99142942662163));
#55216=CARTESIAN_POINT('Ctrl Pts',(6.99999999975917,-24.6138492002674,-9.10317155581979));
#55217=CARTESIAN_POINT('Ctrl Pts',(6.99999999990904,-24.7012880004826,-9.21684861925867));
#55218=CARTESIAN_POINT('Ctrl Pts',(6.99999999989438,-24.7867157006584,-9.33251047983016));
#55219=CARTESIAN_POINT('Ctrl Pts',(6.26386081962776,-15.8144408557884,-3.90572621562457));
#55220=CARTESIAN_POINT('Ctrl Pts',(6.2646071586712,-16.0736409969805,-3.9030665414647));
#55221=CARTESIAN_POINT('Ctrl Pts',(6.26531568823028,-16.3306820728263,-3.90881653564373));
#55222=CARTESIAN_POINT('Ctrl Pts',(6.26598639114327,-16.5850710475842,-3.92256329479193));
#55223=CARTESIAN_POINT('Ctrl Pts',(6.26666474239918,-16.8423609402882,-3.93646681474453));
#55224=CARTESIAN_POINT('Ctrl Pts',(6.26730439940407,-17.0969379570018,-3.95855050562228));
#55225=CARTESIAN_POINT('Ctrl Pts',(6.26790534774945,-17.3483447734508,-3.98839371483313));
#55226=CARTESIAN_POINT('Ctrl Pts',(6.26800177179145,-17.3886837836389,-3.99318215111106));
#55227=CARTESIAN_POINT('Ctrl Pts',(6.26809719927749,-17.4289412844092,-3.9981703715966));
#55228=CARTESIAN_POINT('Ctrl Pts',(6.26819163015533,-17.4691155095948,-4.00335665446775));
#55229=CARTESIAN_POINT('Ctrl Pts',(6.26876871904396,-17.7146294717142,-4.03505122606151));
#55230=CARTESIAN_POINT('Ctrl Pts',(6.26930858726239,-17.9570293256807,-4.07414120498853));
#55231=CARTESIAN_POINT('Ctrl Pts',(6.26981122436712,-18.1959065670098,-4.12010977122704));
#55232=CARTESIAN_POINT('Ctrl Pts',(6.2701791280684,-18.3707520378482,-4.15375632358596));
#55233=CARTESIAN_POINT('Ctrl Pts',(6.27052708539201,-18.5437113313115,-4.19108847665381));
#55234=CARTESIAN_POINT('Ctrl Pts',(6.27085509303089,-18.7146405947199,-4.23191026973416));
#55235=CARTESIAN_POINT('Ctrl Pts',(6.2712113775946,-18.9003053501125,-4.27625123321704));
#55236=CARTESIAN_POINT('Ctrl Pts',(6.27154412351328,-19.0835747569271,-4.32470934801864));
#55237=CARTESIAN_POINT('Ctrl Pts',(6.27185332670676,-19.2642821898755,-4.37704086000345));
#55238=CARTESIAN_POINT('Ctrl Pts',(6.27227096822154,-19.5083641645074,-4.44772516209511));
#55239=CARTESIAN_POINT('Ctrl Pts',(6.27264565837955,-19.7477704004717,-4.52547486619641));
#55240=CARTESIAN_POINT('Ctrl Pts',(6.27297738924788,-19.9821807614481,-4.6096809486922));
#55241=CARTESIAN_POINT('Ctrl Pts',(6.27330912011622,-20.2165911224246,-4.69388703118799));
#55242=CARTESIAN_POINT('Ctrl Pts',(6.27359789171407,-20.4460057935968,-4.78454955708087));
#55243=CARTESIAN_POINT('Ctrl Pts',(6.27384369825113,-20.6701561128595,-4.88108731395748));
#55244=CARTESIAN_POINT('Ctrl Pts',(6.27395596446719,-20.7725313729845,-4.92517860949804));
#55245=CARTESIAN_POINT('Ctrl Pts',(6.27405926829797,-20.8738091877889,-4.97049584617027));
#55246=CARTESIAN_POINT('Ctrl Pts',(6.27415361636911,-20.9739673872759,-5.01698553344749));
#55247=CARTESIAN_POINT('Ctrl Pts',(6.27415652052491,-20.9770503863449,-5.01841654621858));
#55248=CARTESIAN_POINT('Ctrl Pts',(6.27415941613443,-20.9801323246383,-5.0198486698902));
#55249=CARTESIAN_POINT('Ctrl Pts',(6.27416230320351,-20.9832132015518,-5.02128190292619));
#55250=CARTESIAN_POINT('Ctrl Pts',(6.27420631261963,-21.0301769528704,-5.04312957869283));
#55251=CARTESIAN_POINT('Ctrl Pts',(6.27424833750549,-21.0768940659048,-5.06523502894291));
#55252=CARTESIAN_POINT('Ctrl Pts',(6.27428839847348,-21.1233628572361,-5.08759201950987));
#55253=CARTESIAN_POINT('Ctrl Pts',(6.27431785036691,-21.1575256335968,-5.10402835983542));
#55254=CARTESIAN_POINT('Ctrl Pts',(6.27434670151799,-21.1921531263297,-5.12089368240502));
#55255=CARTESIAN_POINT('Ctrl Pts',(6.27437398777163,-21.2260042193405,-5.13758066042605));
#55256=CARTESIAN_POINT('Ctrl Pts',(6.27438625154805,-21.2412185555358,-5.14508060418307));
#55257=CARTESIAN_POINT('Ctrl Pts',(6.27439819920825,-21.2562763691942,-5.15254387739071));
#55258=CARTESIAN_POINT('Ctrl Pts',(6.2744097432151,-21.2710665000488,-5.15991228247023));
#55259=CARTESIAN_POINT('Ctrl Pts',(6.27456064730716,-21.4644041598464,-5.25623260637502));
#55260=CARTESIAN_POINT('Ctrl Pts',(6.2746773653161,-21.6577057048019,-5.3590789236825));
#55261=CARTESIAN_POINT('Ctrl Pts',(6.27475989550217,-21.850472368102,-5.46870175362177));
#55262=CARTESIAN_POINT('Ctrl Pts',(6.27484107219999,-22.0400776740309,-5.57652677819603));
#55263=CARTESIAN_POINT('Ctrl Pts',(6.27488917324043,-22.2291655493083,-5.69090793688106));
#55264=CARTESIAN_POINT('Ctrl Pts',(6.27490419794014,-22.4172131850419,-5.8120683919335));
#55265=CARTESIAN_POINT('Ctrl Pts',(6.27490863190822,-22.4727082850861,-5.84782428723265));
#55266=CARTESIAN_POINT('Ctrl Pts',(6.27491018522934,-22.528112462999,-5.88417049254058));
#55267=CARTESIAN_POINT('Ctrl Pts',(6.27490885790158,-22.5834114504708,-5.92111247066758));
#55268=CARTESIAN_POINT('Ctrl Pts',(6.27490450920186,-22.7645865146092,-6.04214479987562));
#55269=CARTESIAN_POINT('Ctrl Pts',(6.2748692394911,-22.9446359710181,-6.16957378427421));
#55270=CARTESIAN_POINT('Ctrl Pts',(6.27480304923703,-23.1230252934947,-6.30354372742591));
#55271=CARTESIAN_POINT('Ctrl Pts',(6.27475277065118,-23.2585310864459,-6.40530824520284));
#55272=CARTESIAN_POINT('Ctrl Pts',(6.27468465083775,-23.3930780744229,-6.51084651979255));
#55273=CARTESIAN_POINT('Ctrl Pts',(6.27459869032304,-23.5264136418796,-6.62021342797622));
#55274=CARTESIAN_POINT('Ctrl Pts',(6.27448994615905,-23.6950895143096,-6.75856779961703));
#55275=CARTESIAN_POINT('Ctrl Pts',(6.27435264959262,-23.8618281643152,-6.90305003869651));
#55276=CARTESIAN_POINT('Ctrl Pts',(6.2741868031039,-24.0260801485733,-7.05375344142317));
#55277=CARTESIAN_POINT('Ctrl Pts',(6.27401315348193,-24.1980602440996,-7.21154749008647));
#55278=CARTESIAN_POINT('Ctrl Pts',(6.27380820415679,-24.3673135015332,-7.37616273233735));
#55279=CARTESIAN_POINT('Ctrl Pts',(6.27357195890655,-24.5332705410363,-7.54763129887915));
#55280=CARTESIAN_POINT('Ctrl Pts',(6.27333930669852,-24.6967035482112,-7.71649200855313));
#55281=CARTESIAN_POINT('Ctrl Pts',(6.27307630327827,-24.8569398563571,-7.8919992254237));
#55282=CARTESIAN_POINT('Ctrl Pts',(6.27278295324511,-25.0133970264588,-8.0741513007398));
#55283=CARTESIAN_POINT('Ctrl Pts',(6.27261682273637,-25.1020021272812,-8.17730798565161));
#55284=CARTESIAN_POINT('Ctrl Pts',(6.2724409594699,-25.1893944759236,-8.2825952175158));
#55285=CARTESIAN_POINT('Ctrl Pts',(6.27225536443483,-25.2754626136126,-8.39000786636834));
#55286=CARTESIAN_POINT('Ctrl Pts',(6.27204648913939,-25.3723267763896,-8.51089390598911));
#55287=CARTESIAN_POINT('Ctrl Pts',(6.27182528752588,-25.4675139092961,-8.63447218014262));
#55288=CARTESIAN_POINT('Ctrl Pts',(6.27159176118745,-25.5608443099078,-8.76072156011458));
#55289=CARTESIAN_POINT('Ctrl Pts',(-6.390310997303,-15.4600784053605,-3.94962015010527));
#55290=CARTESIAN_POINT('Ctrl Pts',(-4.260207331535,-16.2181814867602,-3.32898635579781));
#55291=CARTESIAN_POINT('Ctrl Pts',(0.0001535201438716,-16.9763032808813,
-2.70680215368588));
#55292=CARTESIAN_POINT('Ctrl Pts',(4.260514371823,-16.2181268476495,-3.32903119765556));
#55293=CARTESIAN_POINT('Ctrl Pts',(6.390771557735,-15.4599144861734,-3.94975434528492));
#55294=CARTESIAN_POINT('Ctrl Pts',(-6.390310997303,-16.2401890659177,-3.91822923290135));
#55295=CARTESIAN_POINT('Ctrl Pts',(-4.260207331535,-16.958959273677,-3.34433191874026));
#55296=CARTESIAN_POINT('Ctrl Pts',(0.0001535201438716,-17.677737083364,
-2.76848699945107));
#55297=CARTESIAN_POINT('Ctrl Pts',(4.260514371823,-16.9589074701588,-3.34437342085115));
#55298=CARTESIAN_POINT('Ctrl Pts',(6.390771557735,-16.2400336513955,-3.91835332258528));
#55299=CARTESIAN_POINT('Ctrl Pts',(-6.390310997303,-18.1257601336346,-4.02650683733696));
#55300=CARTESIAN_POINT('Ctrl Pts',(-4.260207331535,-18.7394139170257,-3.53811573879116));
#55301=CARTESIAN_POINT('Ctrl Pts',(0.0001535201438716,-19.3530458146751,
-3.05103811570896));
#55302=CARTESIAN_POINT('Ctrl Pts',(4.260514371823,-18.7393696915499,-3.53815084329452));
#55303=CARTESIAN_POINT('Ctrl Pts',(6.390771557735,-18.1256274476752,-4.02661243864776));
#55304=CARTESIAN_POINT('Ctrl Pts',(-6.390310997303,-21.0044951210519,-4.89945800150725));
#55305=CARTESIAN_POINT('Ctrl Pts',(-4.260207331535,-21.4424839510746,-4.44478850539219));
#55306=CARTESIAN_POINT('Ctrl Pts',(0.0001535201438716,-21.8807678511962,
-3.98943347064956));
#55307=CARTESIAN_POINT('Ctrl Pts',(4.260514371823,-21.4424523632204,-4.44482132359356));
#55308=CARTESIAN_POINT('Ctrl Pts',(6.390771557735,-21.0044004178749,-4.89955631142534));
#55309=CARTESIAN_POINT('Ctrl Pts',(-6.390310997303,-23.7052287527357,-6.63374442412537));
#55310=CARTESIAN_POINT('Ctrl Pts',(-4.260207331535,-23.9981322521798,-6.09525912369956));
#55311=CARTESIAN_POINT('Ctrl Pts',(0.0001535201438716,-24.2900551830466,
-5.55782158681654));
#55312=CARTESIAN_POINT('Ctrl Pts',(4.260514371823,-23.9981112128033,-6.09529785772377));
#55313=CARTESIAN_POINT('Ctrl Pts',(6.390771557735,-23.7051654203099,-6.63386085694714));
#55314=CARTESIAN_POINT('Ctrl Pts',(-6.390310997303,-25.1149831379802,-8.18394766638624));
#55315=CARTESIAN_POINT('Ctrl Pts',(-4.260207331535,-25.3660571924324,-7.53598855301376));
#55316=CARTESIAN_POINT('Ctrl Pts',(0.0001535201438716,-25.6190353418683,
-6.88615733883246));
#55317=CARTESIAN_POINT('Ctrl Pts',(4.260514371823,-25.366038959873,-7.53603538743866));
#55318=CARTESIAN_POINT('Ctrl Pts',(6.390771557735,-25.1149288500562,-8.18408776992176));
#55319=CARTESIAN_POINT('Ctrl Pts',(-6.390310997303,-25.6807362935916,-8.9842586986279));
#55320=CARTESIAN_POINT('Ctrl Pts',(-4.260207331535,-25.9287981973013,-8.27687157370651));
#55321=CARTESIAN_POINT('Ctrl Pts',(0.0001535201438716,-26.1774653804787,
-7.56887552599929));
#55322=CARTESIAN_POINT('Ctrl Pts',(4.260514371823,-25.9287802754393,-8.27692260016797));
#55323=CARTESIAN_POINT('Ctrl Pts',(6.390771557735,-25.680682656946,-8.98441165186304));
#55324=CARTESIAN_POINT('Ctrl Pts',(-6.26386107908002,-15.8144217366209,
-3.90573578027562));
#55325=CARTESIAN_POINT('Ctrl Pts',(-6.12401716319831,-15.8609391874445,
-3.86696795218159));
#55326=CARTESIAN_POINT('Ctrl Pts',(-5.98376053165562,-15.9057297542361,
-3.82937120018312));
#55327=CARTESIAN_POINT('Ctrl Pts',(-5.84314866563788,-15.9488113053792,
-3.79297601711986));
#55328=CARTESIAN_POINT('Ctrl Pts',(-5.52871437968464,-16.0451496668211,
-3.71158961835612));
#55329=CARTESIAN_POINT('Ctrl Pts',(-5.21250664998199,-16.1329423990905,
-3.63621373671984));
#55330=CARTESIAN_POINT('Ctrl Pts',(-4.89516718476226,-16.2124037512588,
-3.56716941662384));
#55331=CARTESIAN_POINT('Ctrl Pts',(-4.65229613832461,-16.273218316945,-3.51432737171561));
#55332=CARTESIAN_POINT('Ctrl Pts',(-4.40876127626954,-16.3291527723426,
-3.46519332271945));
#55333=CARTESIAN_POINT('Ctrl Pts',(-4.16483356053705,-16.3803011892008,
-3.4198993433696));
#55334=CARTESIAN_POINT('Ctrl Pts',(-3.84173002158442,-16.448051729352,-3.35990351642046));
#55335=CARTESIAN_POINT('Ctrl Pts',(-3.51793901645062,-16.507405349351,-3.30664570419035));
#55336=CARTESIAN_POINT('Ctrl Pts',(-3.19411251218769,-16.5586055111643,
-3.26031478599686));
#55337=CARTESIAN_POINT('Ctrl Pts',(-3.17358297433124,-16.5618514334293,
-3.25737755780072));
#55338=CARTESIAN_POINT('Ctrl Pts',(-3.15305327848952,-16.5650645834705,
-3.25446816200489));
#55339=CARTESIAN_POINT('Ctrl Pts',(-3.13252358460693,-16.5682450223921,
-3.25158664359035));
#55340=CARTESIAN_POINT('Ctrl Pts',(-2.82078843643712,-16.6165387088018,
-3.20783194490625));
#55341=CARTESIAN_POINT('Ctrl Pts',(-2.50902475984557,-16.6572953705827,
-3.17050248577678));
#55342=CARTESIAN_POINT('Ctrl Pts',(-2.19780052300139,-16.6907193045148,
-3.1397510112421));
#55343=CARTESIAN_POINT('Ctrl Pts',(-1.86506876129886,-16.726453039564,-3.10687441910832));
#55344=CARTESIAN_POINT('Ctrl Pts',(-1.53295439181552,-16.7538058312664,
-3.08151509558727));
#55345=CARTESIAN_POINT('Ctrl Pts',(-1.20216613281015,-16.7730740139961,
-3.06357945409478));
#55346=CARTESIAN_POINT('Ctrl Pts',(-0.869774260649804,-16.7924356060608,
-3.04555686323255));
#55347=CARTESIAN_POINT('Ctrl Pts',(-0.538721361552426,-16.8036339974548,
-3.03503012321186));
#55348=CARTESIAN_POINT('Ctrl Pts',(-0.209675401395077,-16.8069665914283,
-3.03189242033579));
#55349=CARTESIAN_POINT('Ctrl Pts',(-0.139707438544078,-16.8076752304622,
-3.03122522272557));
#55350=CARTESIAN_POINT('Ctrl Pts',(-0.0698300377265377,-16.8080282039476,
-3.03089207963549));
#55351=CARTESIAN_POINT('Ctrl Pts',(-4.93267029250509E-5,-16.8080283533074,
-3.03089189447942));
#55352=CARTESIAN_POINT('Ctrl Pts',(0.000256727375841293,-16.8080283539625,
-3.03089189366733));
#55353=CARTESIAN_POINT('Ctrl Pts',(0.000562783265965696,-16.8080283478307,
-3.03089189926015));
#55354=CARTESIAN_POINT('Ctrl Pts',(0.000868840966959984,-16.8080283349116,
-3.03089191125823));
#55355=CARTESIAN_POINT('Ctrl Pts',(0.330223347700769,-16.8080144324858,
-3.03090482262456));
#55356=CARTESIAN_POINT('Ctrl Pts',(0.661679104087344,-16.8001415993432,
-3.03833569807948));
#55357=CARTESIAN_POINT('Ctrl Pts',(0.994608533444343,-16.7841147967613,
-3.05329056982103));
#55358=CARTESIAN_POINT('Ctrl Pts',(1.32345073774953,-16.7682847480354,-3.06806184731997));
#55359=CARTESIAN_POINT('Ctrl Pts',(1.65373070732275,-16.7444997130104,-3.09017351227283));
#55360=CARTESIAN_POINT('Ctrl Pts',(1.98479404869071,-16.7124651864611,-3.11972239231826));
#55361=CARTESIAN_POINT('Ctrl Pts',(2.05630999150204,-16.7055451228889,-3.12610550923702));
#55362=CARTESIAN_POINT('Ctrl Pts',(2.12786230171351,-16.6982400651354,-3.13283565777945));
#55363=CARTESIAN_POINT('Ctrl Pts',(2.1994440690604,-16.6905469802818,-3.13991378115135));
#55364=CARTESIAN_POINT('Ctrl Pts',(2.50988585026661,-16.657182968,-3.17061077716883));
#55365=CARTESIAN_POINT('Ctrl Pts',(2.82088461213451,-16.6165211571424,-3.20785426138439));
#55366=CARTESIAN_POINT('Ctrl Pts',(3.1319039030523,-16.5683497168773,-3.25150005214996));
#55367=CARTESIAN_POINT('Ctrl Pts',(3.45498851193197,-16.5183095701993,-3.29683898658431));
#55368=CARTESIAN_POINT('Ctrl Pts',(3.77809569404769,-16.4601659132149,-3.34908678857731));
#55369=CARTESIAN_POINT('Ctrl Pts',(4.10058014142998,-16.3936746989229,-3.40805934070719));
#55370=CARTESIAN_POINT('Ctrl Pts',(4.12247803430224,-16.3891596982792,-3.41206379623807));
#55371=CARTESIAN_POINT('Ctrl Pts',(4.14437303812036,-16.3846062051229,-3.41609925003709));
#55372=CARTESIAN_POINT('Ctrl Pts',(4.16626494305972,-16.3800141418853,-3.42016564051079));
#55373=CARTESIAN_POINT('Ctrl Pts',(4.48426643316004,-16.3133098986396,-3.47923396889741));
#55374=CARTESIAN_POINT('Ctrl Pts',(4.80161746509365,-16.2384676068073,-3.54483250854387));
#55375=CARTESIAN_POINT('Ctrl Pts',(5.11771182738074,-16.1552757166658,-3.61666694204498));
#55376=CARTESIAN_POINT('Ctrl Pts',(5.36077908835196,-16.0913036017398,-3.67190550709942));
#55377=CARTESIAN_POINT('Ctrl Pts',(5.60310246923606,-16.0223941423869,-3.73083088379307));
#55378=CARTESIAN_POINT('Ctrl Pts',(5.84438925839552,-15.9484491529106,-3.79329715013008));
#55379=CARTESIAN_POINT('Ctrl Pts',(5.98458157661485,-15.9054856755834,-3.82959126601931));
#55380=CARTESIAN_POINT('Ctrl Pts',(6.12442366940432,-15.8608222503357,-3.86708052801428));
#55381=CARTESIAN_POINT('Ctrl Pts',(6.26385845645402,-15.8144409512224,-3.90573485384998));
#55382=CARTESIAN_POINT('Ctrl Pts',(-6.3837685640945,-15.7767343726346,-3.93925153079634));
#55383=CARTESIAN_POINT('Ctrl Pts',(-6.20607782972262,-15.8406682009394,
-3.88901212835295));
#55384=CARTESIAN_POINT('Ctrl Pts',(-5.4836198762884,-16.0875649593149,-3.69326716669371));
#55385=CARTESIAN_POINT('Ctrl Pts',(-4.1035174816222,-16.4626408119468,-3.38487949324654));
#55386=CARTESIAN_POINT('Ctrl Pts',(-2.14467957257126,-16.7896566974073,
-3.10376395696803));
#55387=CARTESIAN_POINT('Ctrl Pts',(0.000847861998201127,-16.9109161991796,
-2.996367192768));
#55388=CARTESIAN_POINT('Ctrl Pts',(2.14629737698611,-16.7894735254493,-3.10392477724487));
#55389=CARTESIAN_POINT('Ctrl Pts',(4.10495670713201,-16.4623223834777,-3.38514788225707));
#55390=CARTESIAN_POINT('Ctrl Pts',(5.48449760235313,-16.0872874995829,-3.6934902959204));
#55391=CARTESIAN_POINT('Ctrl Pts',(6.20649253218868,-15.8405191837971,-3.88912925735201));
#55392=CARTESIAN_POINT('Ctrl Pts',(6.38378443801723,-15.7767286639177,-3.93925601899087));
#55393=CARTESIAN_POINT('Ctrl Pts',(-6.17892139218255,-15.1602625279266,
-3.89269138696012));
#55394=CARTESIAN_POINT('Ctrl Pts',(-6.00683890361596,-15.2221601613956,
-3.84473793976352));
#55395=CARTESIAN_POINT('Ctrl Pts',(-5.30721149445514,-15.461200315072,-3.65787934807116));
#55396=CARTESIAN_POINT('Ctrl Pts',(-3.97097810938147,-15.8243579582481,
-3.36339135340124));
#55397=CARTESIAN_POINT('Ctrl Pts',(-2.07510068658041,-16.1409487021963,
-3.09490132827578));
#55398=CARTESIAN_POINT('Ctrl Pts',(0.000820296697672055,-16.2583236281581,
-2.9923308284817));
#55399=CARTESIAN_POINT('Ctrl Pts',(2.07666620641412,-16.1407713880041,-3.09505492534853));
#55400=CARTESIAN_POINT('Ctrl Pts',(3.9723713467328,-15.8240496584546,-3.36364767993662));
#55401=CARTESIAN_POINT('Ctrl Pts',(5.30806143406014,-15.4609316732643,-3.6580923832534));
#55402=CARTESIAN_POINT('Ctrl Pts',(6.00724051639534,-15.2220158906671,-3.84484973879705));
#55403=CARTESIAN_POINT('Ctrl Pts',(6.17893676471506,-15.1602570013782,-3.89269567046585));
#55404=CARTESIAN_POINT('Ctrl Pts',(-6.17564082336744,-14.7487479575801,
-3.38940352206825));
#55405=CARTESIAN_POINT('Ctrl Pts',(-6.00404507762524,-14.809901241264,-3.34205562192575));
#55406=CARTESIAN_POINT('Ctrl Pts',(-5.30627654165239,-15.0461285322073,
-3.15749986835487));
#55407=CARTESIAN_POINT('Ctrl Pts',(-3.97251250102238,-15.4054450914358,
-2.86622749566697));
#55408=CARTESIAN_POINT('Ctrl Pts',(-2.07720323431513,-15.7192792537822,
-2.600083132903));
#55409=CARTESIAN_POINT('Ctrl Pts',(0.000821374932474116,-15.8358083161971,
-2.49822962199973));
#55410=CARTESIAN_POINT('Ctrl Pts',(2.07876949073072,-15.7191033001096,-2.60023557233471));
#55411=CARTESIAN_POINT('Ctrl Pts',(3.97390417607718,-15.4051397524895,-2.86648131292695));
#55412=CARTESIAN_POINT('Ctrl Pts',(5.30712443090202,-15.0458629393537,-3.15771038243398));
#55413=CARTESIAN_POINT('Ctrl Pts',(6.00444555828538,-14.8097587041699,-3.34216601186277));
#55414=CARTESIAN_POINT('Ctrl Pts',(6.17565615402447,-14.7487424970808,-3.38940775256534));
#55415=CARTESIAN_POINT('Ctrl Pts',(-6.37449173036292,-14.8207095476402,
-2.77587757352679));
#55416=CARTESIAN_POINT('Ctrl Pts',(-6.19797218928426,-14.8829064861205,
-2.72705638613095));
#55417=CARTESIAN_POINT('Ctrl Pts',(-5.47999872535319,-15.1232382790275,
-2.53670636090267));
#55418=CARTESIAN_POINT('Ctrl Pts',(-4.10596568664865,-15.489339540839,-2.23586437891013));
#55419=CARTESIAN_POINT('Ctrl Pts',(-2.14896198146769,-15.8098992465146,
-1.96027369700207));
#55420=CARTESIAN_POINT('Ctrl Pts',(0.000850125320108021,-15.9291719775344,
-1.85457369962847));
#55421=CARTESIAN_POINT('Ctrl Pts',(2.15058105504337,-15.809719266933,-1.96043178241714));
#55422=CARTESIAN_POINT('Ctrl Pts',(4.10740092124632,-15.4890280381271,-2.23612686966137));
#55423=CARTESIAN_POINT('Ctrl Pts',(5.48087148341781,-15.1229679377722,-2.53692358082765));
#55424=CARTESIAN_POINT('Ctrl Pts',(6.19838416728458,-14.8827615143263,-2.72717021488259));
#55425=CARTESIAN_POINT('Ctrl Pts',(6.37450750336995,-14.8207039930432,-2.77588193753119));
#55426=CARTESIAN_POINT('Ctrl Pts',(-6.24994605269825,-14.8593868267772,
-2.76546777148552));
#55427=CARTESIAN_POINT('Ctrl Pts',(-6.11224128919459,-14.9068450911447,
-2.72809069871833));
#55428=CARTESIAN_POINT('Ctrl Pts',(-5.97365547012716,-14.9527218912298,
-2.69169109149479));
#55429=CARTESIAN_POINT('Ctrl Pts',(-5.83421266230798,-14.9970062068934,
-2.65632554963629));
#55430=CARTESIAN_POINT('Ctrl Pts',(-5.52516534036188,-15.0951536077819,
-2.57794484164944));
#55431=CARTESIAN_POINT('Ctrl Pts',(-5.21190774264299,-15.1854811987466,
-2.50464131142876));
#55432=CARTESIAN_POINT('Ctrl Pts',(-4.89477543421764,-15.2678455319869,
-2.43707517713196));
#55433=CARTESIAN_POINT('Ctrl Pts',(-4.66466389456281,-15.3276091796224,
-2.38804911835932));
#55434=CARTESIAN_POINT('Ctrl Pts',(-4.43251153326942,-15.3831813833709,
-2.34203415873297));
#55435=CARTESIAN_POINT('Ctrl Pts',(-4.1984578515508,-15.4345020292727,-2.2992338678819));
#55436=CARTESIAN_POINT('Ctrl Pts',(-4.18854879210617,-15.4366747758291,
-2.29742184500246));
#55437=CARTESIAN_POINT('Ctrl Pts',(-4.1786363290934,-15.4388399004789,-2.29561557911493));
#55438=CARTESIAN_POINT('Ctrl Pts',(-4.16872047032422,-15.4409973987708,
-2.29381508614649));
#55439=CARTESIAN_POINT('Ctrl Pts',(-4.06152918762868,-15.4643201401194,
-2.274351602926));
#55440=CARTESIAN_POINT('Ctrl Pts',(-3.95394109213383,-15.4867517351017,
-2.25556268317071));
#55441=CARTESIAN_POINT('Ctrl Pts',(-3.84597072661888,-15.5082870367113,
-2.23746575262707));
#55442=CARTESIAN_POINT('Ctrl Pts',(-3.78699157947931,-15.5200507620286,
-2.22758024817205));
#55443=CARTESIAN_POINT('Ctrl Pts',(-3.72789835363644,-15.5315470317432,
-2.2179012300442));
#55444=CARTESIAN_POINT('Ctrl Pts',(-3.66869348220133,-15.5427749527341,
-2.20843132159147));
#55445=CARTESIAN_POINT('Ctrl Pts',(-3.63909104648377,-15.5483889132295,
-2.2036963673651));
#55446=CARTESIAN_POINT('Ctrl Pts',(-3.60946069920004,-15.5539357857702,
-2.19901369043729));
#55447=CARTESIAN_POINT('Ctrl Pts',(-3.57980274610709,-15.5594154544918,
-2.19438361195204));
#55448=CARTESIAN_POINT('Ctrl Pts',(-3.56497376956061,-15.5621552888526,
-2.19206857270941));
#55449=CARTESIAN_POINT('Ctrl Pts',(-3.55013789155253,-15.5648783222099,
-2.18976668307023));
#55450=CARTESIAN_POINT('Ctrl Pts',(-3.53529515056274,-15.5675845398395,
-2.18747798241135));
#55451=CARTESIAN_POINT('Ctrl Pts',(-3.52787378006785,-15.5689376486542,
-2.18633363208192));
#55452=CARTESIAN_POINT('Ctrl Pts',(-3.52045069382698,-15.5702865535341,
-2.18519257899711));
#55453=CARTESIAN_POINT('Ctrl Pts',(-3.5130258966674,-15.5716312526235,-2.18405482802872));
#55454=CARTESIAN_POINT('Ctrl Pts',(-3.50560109950782,-15.572975951713,-2.18291707706032));
#55455=CARTESIAN_POINT('Ctrl Pts',(-3.49969582841781,-15.5740427847343,
-2.18201427674118));
#55456=CARTESIAN_POINT('Ctrl Pts',(-3.49074637726386,-15.5756527306545,
-2.1806514863284));
#55457=CARTESIAN_POINT('Ctrl Pts',(-3.18937218028059,-15.6298679166515,
-2.13475930151785));
#55458=CARTESIAN_POINT('Ctrl Pts',(-2.8863104354888,-15.6769573631538,-2.09449088189289));
#55459=CARTESIAN_POINT('Ctrl Pts',(-2.58189061930374,-15.7169297571031,
-2.06012185686861));
#55460=CARTESIAN_POINT('Ctrl Pts',(-2.45625178067274,-15.733426991797,-2.04593722052317));
#55461=CARTESIAN_POINT('Ctrl Pts',(-2.33038134326096,-15.7487114909266,
-2.03275775631289));
#55462=CARTESIAN_POINT('Ctrl Pts',(-2.20430144629838,-15.7627819152971,
-2.02060420803763));
#55463=CARTESIAN_POINT('Ctrl Pts',(-1.90245288183243,-15.7964679945211,
-1.99150733225939));
#55464=CARTESIAN_POINT('Ctrl Pts',(-1.59940460449395,-15.8231979990122,
-1.96828846747673));
#55465=CARTESIAN_POINT('Ctrl Pts',(-1.29555337158924,-15.842976677377,-1.95105143023668));
#55466=CARTESIAN_POINT('Ctrl Pts',(-0.993107503021079,-15.8626638759445,
-1.93389411726555));
#55467=CARTESIAN_POINT('Ctrl Pts',(-0.689865522197483,-15.875463913011,
-1.92266330219558));
#55468=CARTESIAN_POINT('Ctrl Pts',(-0.386210791332723,-15.881342888697,
-1.91749439950967));
#55469=CARTESIAN_POINT('Ctrl Pts',(-0.257555172826256,-15.883833754724,
-1.91530438465247));
#55470=CARTESIAN_POINT('Ctrl Pts',(-0.128825412042817,-15.8850817198573,
-1.91420298318698));
#55471=CARTESIAN_POINT('Ctrl Pts',(-5.06157679712277E-5,-15.8850820917059,
-1.91420238091613));
#55472=CARTESIAN_POINT('Ctrl Pts',(0.000256975117818086,-15.8850820925941,
-1.91420237947755));
#55473=CARTESIAN_POINT('Ctrl Pts',(0.000564565725845489,-15.885082086369,
-1.91420238427594));
#55474=CARTESIAN_POINT('Ctrl Pts',(0.000872156055743548,-15.8850820730305,
-1.91420239531148));
#55475=CARTESIAN_POINT('Ctrl Pts',(0.297675497334216,-15.8850692023486,
-1.91421304384406));
#55476=CARTESIAN_POINT('Ctrl Pts',(0.594220548053702,-15.8784364142884,
-1.9200281299929));
#55477=CARTESIAN_POINT('Ctrl Pts',(0.890169967705006,-15.8652261227378,
-1.93155600891819));
#55478=CARTESIAN_POINT('Ctrl Pts',(1.17953867129292,-15.8523095745503,-1.94282755452101));
#55479=CARTESIAN_POINT('Ctrl Pts',(1.46833837285049,-15.8331045734909,-1.95956096628514));
#55480=CARTESIAN_POINT('Ctrl Pts',(1.75624190641963,-15.8076155284317,-1.9817012282312));
#55481=CARTESIAN_POINT('Ctrl Pts',(1.90640216753209,-15.7943213475158,-1.99324880277364));
#55482=CARTESIAN_POINT('Ctrl Pts',(2.05632258772584,-15.7793184671638,-2.00625435834685));
#55483=CARTESIAN_POINT('Ctrl Pts',(2.20595339365679,-15.762605219908,-2.02070306900956));
#55484=CARTESIAN_POINT('Ctrl Pts',(2.34662518566424,-15.7468926637462,-2.03428667573061));
#55485=CARTESIAN_POINT('Ctrl Pts',(2.48704100784772,-15.7296684005041,-2.04914582503358));
#55486=CARTESIAN_POINT('Ctrl Pts',(2.62716943519071,-15.7109343642876,-2.06524908302113));
#55487=CARTESIAN_POINT('Ctrl Pts',(2.77176006676714,-15.6916037674924,-2.08186512793797));
#55488=CARTESIAN_POINT('Ctrl Pts',(2.91604212779795,-15.6706654399321,-2.09981011040458));
#55489=CARTESIAN_POINT('Ctrl Pts',(3.05997654759935,-15.6481199360848,-2.11905354500426));
#55490=CARTESIAN_POINT('Ctrl Pts',(3.13194375750006,-15.6368471841611,-2.12867526230409));
#55491=CARTESIAN_POINT('Ctrl Pts',(3.20382405485216,-15.6251726137908,-2.13862158957259));
#55492=CARTESIAN_POINT('Ctrl Pts',(3.27561263489304,-15.613096202853,-2.14888818338128));
#55493=CARTESIAN_POINT('Ctrl Pts',(3.31150692491348,-15.6070579973841,-2.15402148028563));
#55494=CARTESIAN_POINT('Ctrl Pts',(3.34737828542149,-15.6009193302214,-2.15923484362356));
#55495=CARTESIAN_POINT('Ctrl Pts',(3.38322611752088,-15.5946801907778,-2.16452771501257));
#55496=CARTESIAN_POINT('Ctrl Pts',(3.40115003357058,-15.591560621056,-2.16717415070707));
#55497=CARTESIAN_POINT('Ctrl Pts',(3.41906806750332,-15.5884159331665,-2.16984046340098));
#55498=CARTESIAN_POINT('Ctrl Pts',(3.43698014470371,-15.5852461253899,-2.17252658147989));
#55499=CARTESIAN_POINT('Ctrl Pts',(3.44593618330391,-15.5836612215015,-2.17386964051935));
#55500=CARTESIAN_POINT('Ctrl Pts',(3.45489073272004,-15.5820700376354,-2.17521765090421));
#55501=CARTESIAN_POINT('Ctrl Pts',(3.46384378364179,-15.5804725735521,-2.17657060356384));
#55502=CARTESIAN_POINT('Ctrl Pts',(3.47279683456355,-15.5788751094689,-2.17792355622348));
#55503=CARTESIAN_POINT('Ctrl Pts',(3.48327010629409,-15.5769976228693,-2.1795131641832));
#55504=CARTESIAN_POINT('Ctrl Pts',(3.49069843161647,-15.5756613403914,-2.18064427925889));
#55505=CARTESIAN_POINT('Ctrl Pts',(3.71882625272019,-15.5346233948462,-2.21538142477097));
#55506=CARTESIAN_POINT('Ctrl Pts',(3.94535648705172,-15.4896112321074,-2.25326998516031));
#55507=CARTESIAN_POINT('Ctrl Pts',(4.17013179886758,-15.4406820257936,-2.29412672109735));
#55508=CARTESIAN_POINT('Ctrl Pts',(4.49398044986303,-15.3701864836853,-2.35299172148549));
#55509=CARTESIAN_POINT('Ctrl Pts',(4.8141865358934,-15.2915616281918,-2.41801658538009));
#55510=CARTESIAN_POINT('Ctrl Pts',(5.13041264068862,-15.2049672772219,-2.48860252594909));
#55511=CARTESIAN_POINT('Ctrl Pts',(5.36770661560993,-15.1399874497005,-2.54156974831684));
#55512=CARTESIAN_POINT('Ctrl Pts',(5.60275959993477,-15.0705192344865,-2.5976691992491));
#55513=CARTESIAN_POINT('Ctrl Pts',(5.8354275471442,-14.9966156188503,-2.65666031041631));
#55514=CARTESIAN_POINT('Ctrl Pts',(5.97445995846876,-14.9524539798677,-2.69191087471044));
#55515=CARTESIAN_POINT('Ctrl Pts',(6.11264069900418,-14.9067083356646,-2.72819417249631));
#55516=CARTESIAN_POINT('Ctrl Pts',(6.24994470386048,-14.8593882189047,-2.76546244225239));
#55517=CARTESIAN_POINT('Ctrl Pts',(7.10495696060184,-15.2147787467643,5.08680107463094));
#55518=CARTESIAN_POINT('Ctrl Pts',(7.10596084475798,-15.2419087055295,5.00460205443588));
#55519=CARTESIAN_POINT('Ctrl Pts',(7.09052318662475,-15.3082820625518,4.81707696377181));
#55520=CARTESIAN_POINT('Ctrl Pts',(7.0043168782856,-15.4227062459899,4.53822716637853));
#55521=CARTESIAN_POINT('Ctrl Pts',(6.84418516995453,-15.5500445504962,4.27661325180109));
#55522=CARTESIAN_POINT('Ctrl Pts',(6.63017629479599,-15.673047448177,4.07076452833132));
#55523=CARTESIAN_POINT('Ctrl Pts',(6.42344282838547,-15.7648481127942,3.95589962337636));
#55524=CARTESIAN_POINT('Ctrl Pts',(6.29350100205884,-15.8132040931925,3.9133231394474));
#55525=CARTESIAN_POINT('Ctrl Pts',(6.25215637714488,-15.8277458920358,3.90246971967927));
#55526=CARTESIAN_POINT('Ctrl Pts',(6.81722694411318,-14.6678650098582,4.90248406328812));
#55527=CARTESIAN_POINT('Ctrl Pts',(6.81812715945108,-14.691775308277,4.83000073281271));
#55528=CARTESIAN_POINT('Ctrl Pts',(6.80424853975033,-14.7506252433578,4.66430263806235));
#55529=CARTESIAN_POINT('Ctrl Pts',(6.72648871389155,-14.8529185526735,4.41778502112603));
#55530=CARTESIAN_POINT('Ctrl Pts',(6.58227945968176,-14.9671735461734,4.18722534021326));
#55531=CARTESIAN_POINT('Ctrl Pts',(6.39031761580399,-15.0775057042662,4.00683702016848));
#55532=CARTESIAN_POINT('Ctrl Pts',(6.20591548437909,-15.159553132176,3.90697891677903));
#55533=CARTESIAN_POINT('Ctrl Pts',(6.09061389420951,-15.2025631711381,3.87022200760893));
#55534=CARTESIAN_POINT('Ctrl Pts',(6.05399099367591,-15.2154743878466,3.86087547311471));
#55535=CARTESIAN_POINT('Ctrl Pts',(7.05919742644666,-14.099365919639,4.71767508414311));
#55536=CARTESIAN_POINT('Ctrl Pts',(7.06038809058804,-14.1302863226927,4.62399558055472));
#55537=CARTESIAN_POINT('Ctrl Pts',(7.04218600841309,-14.205534883539,4.41132787330049));
#55538=CARTESIAN_POINT('Ctrl Pts',(6.94133832169349,-14.3347911618672,4.09585993930461));
#55539=CARTESIAN_POINT('Ctrl Pts',(6.75329582486237,-14.4793527715302,3.79837680263864));
#55540=CARTESIAN_POINT('Ctrl Pts',(6.49963210608973,-14.6206396718045,3.56192024772834));
#55541=CARTESIAN_POINT('Ctrl Pts',(6.25142152215052,-14.7279766140739,3.42816698756074));
#55542=CARTESIAN_POINT('Ctrl Pts',(6.09355729230462,-14.7855072753609,3.37811577971091));
#55543=CARTESIAN_POINT('Ctrl Pts',(6.04313356608242,-14.8029143472445,3.36532862725582));
#55544=CARTESIAN_POINT('Ctrl Pts',(7.66738224158263,-13.8935052574552,4.65727912036421));
#55545=CARTESIAN_POINT('Ctrl Pts',(7.66906120809273,-13.9369286846848,4.52581419290841));
#55546=CARTESIAN_POINT('Ctrl Pts',(7.64357464066956,-14.0414170913453,4.22911839576172));
#55547=CARTESIAN_POINT('Ctrl Pts',(7.50370581709582,-14.2185108259714,3.79000846918474));
#55548=CARTESIAN_POINT('Ctrl Pts',(7.24169365276974,-14.416290207258,3.37284545922798));
#55549=CARTESIAN_POINT('Ctrl Pts',(6.88427276433928,-14.6112405403477,3.03667830773213));
#55550=CARTESIAN_POINT('Ctrl Pts',(6.52923106880879,-14.7618210155054,2.84303151425121));
#55551=CARTESIAN_POINT('Ctrl Pts',(6.30036209622375,-14.8439269044745,2.76955534331772));
#55552=CARTESIAN_POINT('Ctrl Pts',(6.22694060282119,-14.8689183013122,2.75070496021726));
#55553=CARTESIAN_POINT('',(6.2638598901157,-15.8144313886664,3.90573722905719));
#55554=CARTESIAN_POINT('',(6.24994591741779,-14.8593874699437,2.76546569721984));
#55555=CARTESIAN_POINT('Ctrl Pts',(6.26385676107766,-15.8144315143033,3.90574866939898));
#55556=CARTESIAN_POINT('Ctrl Pts',(6.25434379880635,-15.7850266167952,3.90346982270102));
#55557=CARTESIAN_POINT('Ctrl Pts',(6.24500788984914,-15.7549953789465,3.89975105195181));
#55558=CARTESIAN_POINT('Ctrl Pts',(6.23595188136702,-15.7245103682235,3.8944427648052));
#55559=CARTESIAN_POINT('Ctrl Pts',(6.22712248221697,-15.6947881867238,3.88926730741544));
#55560=CARTESIAN_POINT('Ctrl Pts',(6.2185594413941,-15.664634965679,3.88258020830732));
#55561=CARTESIAN_POINT('Ctrl Pts',(6.21036401048873,-15.6342507943812,3.87427078583523));
#55562=CARTESIAN_POINT('Ctrl Pts',(6.20229493636841,-15.6043350848697,3.86608947766504));
#55563=CARTESIAN_POINT('Ctrl Pts',(6.19458254627921,-15.5741959424333,3.85633486755289));
#55564=CARTESIAN_POINT('Ctrl Pts',(6.18732480245288,-15.5440582729263,3.84493840162574));
#55565=CARTESIAN_POINT('Ctrl Pts',(6.18019462696393,-15.5144503289763,3.83374224976934));
#55566=CARTESIAN_POINT('Ctrl Pts',(6.17350358986061,-15.4848444425667,3.82096101904608));
#55567=CARTESIAN_POINT('Ctrl Pts',(6.16734101033035,-15.4554788128665,3.80657352922948));
#55568=CARTESIAN_POINT('Ctrl Pts',(6.16654374976043,-15.4516797448697,3.80471220179757));
#55569=CARTESIAN_POINT('Ctrl Pts',(6.16575532487597,-15.4478847246442,3.80282405647154));
#55570=CARTESIAN_POINT('Ctrl Pts',(6.16497592004,-15.4440942898146,3.80090910734589));
#55571=CARTESIAN_POINT('Ctrl Pts',(6.15904357729299,-15.4152438676313,3.78633371079701));
#55572=CARTESIAN_POINT('Ctrl Pts',(6.15363479800696,-15.3866584553602,3.77020145346772));
#55573=CARTESIAN_POINT('Ctrl Pts',(6.14882417024651,-15.3585810547484,3.75254629327471));
#55574=CARTESIAN_POINT('Ctrl Pts',(6.14407517199114,-15.3308633569425,3.73511731536792));
#55575=CARTESIAN_POINT('Ctrl Pts',(6.13990937017329,-15.3036415436826,3.71620422607133));
#55576=CARTESIAN_POINT('Ctrl Pts',(6.13638525666128,-15.2771503252054,3.69588866707889));
#55577=CARTESIAN_POINT('Ctrl Pts',(6.13288183768904,-15.2508146702685,3.67569240649792));
#55578=CARTESIAN_POINT('Ctrl Pts',(6.13001281258441,-15.2252018603058,3.65411031081203));
#55579=CARTESIAN_POINT('Ctrl Pts',(6.12781875017019,-15.2005313792643,3.6312696488277));
#55580=CARTESIAN_POINT('Ctrl Pts',(6.12563213271504,-15.1759446108464,3.60850649046963));
#55581=CARTESIAN_POINT('Ctrl Pts',(6.1241160438716,-15.1522945325966,3.5844937213183));
#55582=CARTESIAN_POINT('Ctrl Pts',(6.1232911028458,-15.1297756714056,3.55939941650749));
#55583=CARTESIAN_POINT('Ctrl Pts',(6.1224669045622,-15.1072770852501,3.53432770555339));
#55584=CARTESIAN_POINT('Ctrl Pts',(6.12233265472249,-15.0859083031204,3.50817702111357));
#55585=CARTESIAN_POINT('Ctrl Pts',(6.12288798583855,-15.0658302715291,3.48114923737607));
#55586=CARTESIAN_POINT('Ctrl Pts',(6.12344602286289,-15.0456544076528,3.45398975796753));
#55587=CARTESIAN_POINT('Ctrl Pts',(6.1247003340058,-15.0267823796104,3.42594536020585));
#55588=CARTESIAN_POINT('Ctrl Pts',(6.12662935671012,-15.009335720049,3.39724519948053));
#55589=CARTESIAN_POINT('Ctrl Pts',(6.12856584253839,-14.9918215617575,3.36843400177455));
#55590=CARTESIAN_POINT('Ctrl Pts',(6.13118211919576,-14.9757440612021,3.33896280103151));
#55591=CARTESIAN_POINT('Ctrl Pts',(6.13443655377272,-14.9611787464408,3.30907576756275));
#55592=CARTESIAN_POINT('Ctrl Pts',(6.13772838224608,-14.9464460742299,3.27884532801018));
#55593=CARTESIAN_POINT('Ctrl Pts',(6.14167289476094,-14.9332605876828,3.2481903112989));
#55594=CARTESIAN_POINT('Ctrl Pts',(6.14620958715487,-14.9216497189146,3.21736297478641));
#55595=CARTESIAN_POINT('Ctrl Pts',(6.14951384885931,-14.9131930404153,3.1949101438155));
#55596=CARTESIAN_POINT('Ctrl Pts',(6.15313186295512,-14.9055705611463,3.17236592052286));
#55597=CARTESIAN_POINT('Ctrl Pts',(6.15703571528297,-14.8987765659417,3.14982379446668));
#55598=CARTESIAN_POINT('Ctrl Pts',(6.16249126701368,-14.8892821001721,3.11832164620606));
#55599=CARTESIAN_POINT('Ctrl Pts',(6.16850504640394,-14.8814072953678,3.0868249131614));
#55600=CARTESIAN_POINT('Ctrl Pts',(6.17499163073684,-14.8750962878681,3.05556885520286));
#55601=CARTESIAN_POINT('Ctrl Pts',(6.18162661140325,-14.8686409007804,3.02359773918563));
#55602=CARTESIAN_POINT('Ctrl Pts',(6.18875592528047,-14.8638211729704,2.99187907491926));
#55603=CARTESIAN_POINT('Ctrl Pts',(6.19628251443661,-14.8605346123414,2.96063113067753));
#55604=CARTESIAN_POINT('Ctrl Pts',(6.20392059387846,-14.8571993683613,2.92892031511933));
#55605=CARTESIAN_POINT('Ctrl Pts',(6.21196745122266,-14.855442332926,2.8976946499334));
#55606=CARTESIAN_POINT('Ctrl Pts',(6.2203213744668,-14.8551224309158,2.86714030820995));
#55607=CARTESIAN_POINT('Ctrl Pts',(6.22887565822237,-14.8547948563751,2.83585315109482));
#55608=CARTESIAN_POINT('Ctrl Pts',(6.23775158600005,-14.8559734060631,2.80527012090917));
#55609=CARTESIAN_POINT('Ctrl Pts',(6.24684494550031,-14.8584827088845,2.77554272822559));
#55610=CARTESIAN_POINT('Ctrl Pts',(6.24787581205197,-14.8587671754061,2.7721726893764));
#55611=CARTESIAN_POINT('Ctrl Pts',(6.24890948106048,-14.8590687268172,2.76881359532572));
#55612=CARTESIAN_POINT('Ctrl Pts',(6.24994580734849,-14.8593870957008,2.76546562756306));
#55613=CARTESIAN_POINT('',(7.000000212767,-14.5427408801051,3.16613451323743));
#55614=CARTESIAN_POINT('Ctrl Pts',(7.00000061650467,-14.5427408381467,3.16613402467205));
#55615=CARTESIAN_POINT('Ctrl Pts',(6.9274660400329,-14.5808036624884,3.10292449647818));
#55616=CARTESIAN_POINT('Ctrl Pts',(6.77485267168808,-14.6548676519438,2.98919830046988));
#55617=CARTESIAN_POINT('Ctrl Pts',(6.523266472515,-14.7608743894712,2.85474660862042));
#55618=CARTESIAN_POINT('Ctrl Pts',(6.343316019062,-14.8272098476568,2.79080490252102));
#55619=CARTESIAN_POINT('Ctrl Pts',(6.249945936522,-14.8593875349017,2.76546570931229));
#55620=CARTESIAN_POINT('',(7.,-14.7967973072037,4.92969292433389));
#55621=CARTESIAN_POINT('Ctrl Pts',(7.,-14.7967973072037,4.92969292433389));
#55622=CARTESIAN_POINT('Ctrl Pts',(7.,-14.7447744258633,4.79864067714473));
#55623=CARTESIAN_POINT('Ctrl Pts',(7.,-14.7000166221108,4.67450080516981));
#55624=CARTESIAN_POINT('Ctrl Pts',(7.,-14.6625238959461,4.55727330840913));
#55625=CARTESIAN_POINT('Ctrl Pts',(7.,-14.6500263205578,4.51819747615557));
#55626=CARTESIAN_POINT('Ctrl Pts',(7.,-14.6389585887663,4.48203729950645));
#55627=CARTESIAN_POINT('Ctrl Pts',(7.,-14.6274528623107,4.44234993671987));
#55628=CARTESIAN_POINT('Ctrl Pts',(7.,-14.5814299564882,4.28360048557353));
#55629=CARTESIAN_POINT('Ctrl Pts',(7.,-14.5472852583712,4.12817676488021));
#55630=CARTESIAN_POINT('Ctrl Pts',(7.,-14.5257751444716,3.98124543293447));
#55631=CARTESIAN_POINT('Ctrl Pts',(7.,-14.4827549166725,3.687382769043));
#55632=CARTESIAN_POINT('Ctrl Pts',(7.,-14.4884099871871,3.41567923317487));
#55633=CARTESIAN_POINT('Ctrl Pts',(7.,-14.5427403560153,3.1661348253301));
#55634=CARTESIAN_POINT('Ctrl Pts',(6.99999343558281,-14.7967973069948,4.92969292493306));
#55635=CARTESIAN_POINT('Ctrl Pts',(6.99998714159524,-14.8239179309797,4.89270461052958));
#55636=CARTESIAN_POINT('Ctrl Pts',(6.9982547064127,-14.850757358501,4.85673485006274));
#55637=CARTESIAN_POINT('Ctrl Pts',(6.99505575114715,-14.8771900729887,4.82190106750212));
#55638=CARTESIAN_POINT('Ctrl Pts',(6.99209903435036,-14.9016211901575,4.78970504678811));
#55639=CARTESIAN_POINT('Ctrl Pts',(6.98788864163826,-14.9257052987112,4.75847903979292));
#55640=CARTESIAN_POINT('Ctrl Pts',(6.98260450667771,-14.9493619608291,4.72829169721352));
#55641=CARTESIAN_POINT('Ctrl Pts',(6.97647442545662,-14.9768058587017,4.69327161100413));
#55642=CARTESIAN_POINT('Ctrl Pts',(6.96890071874895,-15.0036742903436,4.65964911936404));
#55643=CARTESIAN_POINT('Ctrl Pts',(6.96018164214258,-15.029873005234,4.62746011075656));
#55644=CARTESIAN_POINT('Ctrl Pts',(6.95290685067125,-15.0517319928595,4.60060310102263));
#55645=CARTESIAN_POINT('Ctrl Pts',(6.94483369969458,-15.0731252847008,4.57474347357701));
#55646=CARTESIAN_POINT('Ctrl Pts',(6.93611472286893,-15.0940101584121,4.54988840293343));
#55647=CARTESIAN_POINT('Ctrl Pts',(6.92641726606428,-15.1172388198407,4.5222439924983));
#55648=CARTESIAN_POINT('Ctrl Pts',(6.9159209747684,-15.1398384368918,4.49584242419178));
#55649=CARTESIAN_POINT('Ctrl Pts',(6.90481356637586,-15.1617639785878,4.47067684408087));
#55650=CARTESIAN_POINT('Ctrl Pts',(6.89164887893216,-15.187750499769,4.44085017481732));
#55651=CARTESIAN_POINT('Ctrl Pts',(6.87762735375645,-15.2127898786367,4.41275936110785));
#55652=CARTESIAN_POINT('Ctrl Pts',(6.86305650501248,-15.2368326817435,4.38633881455129));
#55653=CARTESIAN_POINT('Ctrl Pts',(6.85386413204496,-15.2520006666169,4.36967077261212));
#55654=CARTESIAN_POINT('Ctrl Pts',(6.84445212298921,-15.2667724597872,4.35366711183038));
#55655=CARTESIAN_POINT('Ctrl Pts',(6.83488868064054,-15.2811396624472,4.33830772432577));
#55656=CARTESIAN_POINT('Ctrl Pts',(6.82863658643842,-15.2905322118218,4.32826653475569));
#55657=CARTESIAN_POINT('Ctrl Pts',(6.82231963531967,-15.2997519048661,4.31850064377616));
#55658=CARTESIAN_POINT('Ctrl Pts',(6.81595546454256,-15.3087970230533,4.30900383629424));
#55659=CARTESIAN_POINT('Ctrl Pts',(6.812773379154,-15.3133195821468,4.30425543255328));
#55660=CARTESIAN_POINT('Ctrl Pts',(6.80957948092657,-15.3177984978365,4.29957430535766));
#55661=CARTESIAN_POINT('Ctrl Pts',(6.80637586700466,-15.3222336059642,4.29495962197931));
#55662=CARTESIAN_POINT('Ctrl Pts',(6.8047740600437,-15.324451160028,4.29265228029014));
#55663=CARTESIAN_POINT('Ctrl Pts',(6.80316982367116,-15.3266577622202,4.29036154989132));
#55664=CARTESIAN_POINT('Ctrl Pts',(6.80156341558733,-15.3288533933844,4.28808732631316));
#55665=CARTESIAN_POINT('Ctrl Pts',(6.80017844998843,-15.3307463579809,4.28612660322439));
#55666=CARTESIAN_POINT('Ctrl Pts',(6.79918126657756,-15.3321039244195,4.28472268101543));
#55667=CARTESIAN_POINT('Ctrl Pts',(6.79756509623338,-15.3342897856083,4.2824669077432));
#55668=CARTESIAN_POINT('Ctrl Pts',(6.79730668636575,-15.334639283483,4.28210623160855));
#55669=CARTESIAN_POINT('Ctrl Pts',(6.79703237237366,-15.3350099512053,4.28172384280776));
#55670=CARTESIAN_POINT('Ctrl Pts',(6.7967379311547,-15.3354073554815,4.28131407143311));
#55671=CARTESIAN_POINT('Ctrl Pts',(6.78772434840391,-15.3475728951486,4.26876994392498));
#55672=CARTESIAN_POINT('Ctrl Pts',(6.77846784471264,-15.3596525050359,4.25648444123868));
#55673=CARTESIAN_POINT('Ctrl Pts',(6.76897945880369,-15.3716409411952,4.2444655704202));
#55674=CARTESIAN_POINT('Ctrl Pts',(6.73811526233739,-15.4106373998654,4.20537011268854));
#55675=CARTESIAN_POINT('Ctrl Pts',(6.7048017087282,-15.4486674809531,4.16909532298495));
#55676=CARTESIAN_POINT('Ctrl Pts',(6.66950284278148,-15.4855742727397,4.13580485241239));
#55677=CARTESIAN_POINT('Ctrl Pts',(6.64224200441824,-15.5140768905552,4.11009507072465));
#55678=CARTESIAN_POINT('Ctrl Pts',(6.61379575867552,-15.5419100335608,4.0861655014366));
#55679=CARTESIAN_POINT('Ctrl Pts',(6.58435873894976,-15.5690100258892,4.0640921555984));
#55680=CARTESIAN_POINT('Ctrl Pts',(6.54460852115848,-15.6056044436405,4.03428545938306));
#55681=CARTESIAN_POINT('Ctrl Pts',(6.50305392191834,-15.6408613873316,4.00786272879156));
#55682=CARTESIAN_POINT('Ctrl Pts',(6.46023258511493,-15.6746538066925,3.98488306639121));
#55683=CARTESIAN_POINT('Ctrl Pts',(6.42831606070949,-15.6998407031736,3.96775536766484));
#55684=CARTESIAN_POINT('Ctrl Pts',(6.39569462096411,-15.7242144403282,3.95254071434452));
#55685=CARTESIAN_POINT('Ctrl Pts',(6.36257366505378,-15.7477295054672,3.93926371625084));
#55686=CARTESIAN_POINT('Ctrl Pts',(6.33007871080959,-15.7708001247999,3.92623765967438));
#55687=CARTESIAN_POINT('Ctrl Pts',(6.2971030388051,-15.7930443446869,3.91507635689925));
#55688=CARTESIAN_POINT('Ctrl Pts',(6.26385676124029,-15.8144315141987,3.90574866944461));
#55689=CARTESIAN_POINT('Ctrl Pts',(6.99927539745615,-24.8232831402285,9.44704209109788));
#55690=CARTESIAN_POINT('Ctrl Pts',(6.99927539745615,-24.8010531575336,9.4162903362361));
#55691=CARTESIAN_POINT('Ctrl Pts',(6.99927539745615,-24.4365976663568,8.91758027915424));
#55692=CARTESIAN_POINT('Ctrl Pts',(6.99927539745615,-23.6477703264689,8.00909386847417));
#55693=CARTESIAN_POINT('Ctrl Pts',(6.99927539745615,-22.3080761741899,6.88883533571338));
#55694=CARTESIAN_POINT('Ctrl Pts',(6.99927539745615,-20.8057449101191,5.99308684816581));
#55695=CARTESIAN_POINT('Ctrl Pts',(6.99927539745615,-19.1796205257273,5.34745368361758));
#55696=CARTESIAN_POINT('Ctrl Pts',(6.99927539745615,-17.4733157461454,4.96741765649446));
#55697=CARTESIAN_POINT('Ctrl Pts',(6.99927539745615,-15.9617928931792,4.87762288481046));
#55698=CARTESIAN_POINT('Ctrl Pts',(6.99927539745615,-15.0339583706354,4.94001221664358));
#55699=CARTESIAN_POINT('Ctrl Pts',(6.99927539745615,-14.6874883923254,4.98003222191423));
#55700=CARTESIAN_POINT('Ctrl Pts',(7.01782517045299,-25.2179999147367,9.16177341463118));
#55701=CARTESIAN_POINT('Ctrl Pts',(7.01782517045299,-25.19478265848,9.12965654467665));
#55702=CARTESIAN_POINT('Ctrl Pts',(7.01782517045299,-24.8141504925113,8.60881700089838));
#55703=CARTESIAN_POINT('Ctrl Pts',(7.01782517045299,-23.9905674344651,7.66026544206334));
#55704=CARTESIAN_POINT('Ctrl Pts',(7.01782517045299,-22.5908623958162,6.48980066752073));
#55705=CARTESIAN_POINT('Ctrl Pts',(7.01782517045299,-21.0220249302349,5.55445248829491));
#55706=CARTESIAN_POINT('Ctrl Pts',(7.01782517045299,-19.3234985875938,4.88000520626589));
#55707=CARTESIAN_POINT('Ctrl Pts',(7.01782517045299,-17.5410927392784,4.48306759693387));
#55708=CARTESIAN_POINT('Ctrl Pts',(7.01782517045299,-15.962488194199,4.38928801747339));
#55709=CARTESIAN_POINT('Ctrl Pts',(7.01782517045299,-14.9935216292188,4.45442837118926));
#55710=CARTESIAN_POINT('Ctrl Pts',(7.01782517045299,-14.6315898189319,4.4962370680108));
#55711=CARTESIAN_POINT('Ctrl Pts',(6.7281872031432,-25.5366594111987,8.93147265552196));
#55712=CARTESIAN_POINT('Ctrl Pts',(6.7281872031432,-25.5126451173818,8.89825371210526));
#55713=CARTESIAN_POINT('Ctrl Pts',(6.7281872031432,-25.1189533315064,8.35954877332631));
#55714=CARTESIAN_POINT('Ctrl Pts',(6.7281872031432,-24.2673115732516,7.37865214896281));
#55715=CARTESIAN_POINT('Ctrl Pts',(6.7281872031432,-22.819159039915,6.16765528467975));
#55716=CARTESIAN_POINT('Ctrl Pts',(6.7281872031432,-21.1966303353074,5.20033780841415));
#55717=CARTESIAN_POINT('Ctrl Pts',(6.7281872031432,-19.4396530398759,4.50262855029769));
#55718=CARTESIAN_POINT('Ctrl Pts',(6.7281872031432,-17.5958099033305,4.09204609479212));
#55719=CARTESIAN_POINT('Ctrl Pts',(6.7281872031432,-15.9630495188911,3.99504953312507));
#55720=CARTESIAN_POINT('Ctrl Pts',(6.7281872031432,-14.9608765720764,4.06241081917415));
#55721=CARTESIAN_POINT('Ctrl Pts',(6.7281872031432,-14.5864622429053,4.10566354772994));
#55722=CARTESIAN_POINT('Ctrl Pts',(6.25506922963065,-25.6378135708472,8.85836678542715));
#55723=CARTESIAN_POINT('Ctrl Pts',(6.25506922963065,-25.6135462682048,8.82479800364957));
#55724=CARTESIAN_POINT('Ctrl Pts',(6.25506922963065,-25.2157088821168,8.28042193616291));
#55725=CARTESIAN_POINT('Ctrl Pts',(6.25506922963065,-24.3551602678926,7.28925780695488));
#55726=CARTESIAN_POINT('Ctrl Pts',(6.25506922963065,-22.8916287307343,6.06539457741163));
#55727=CARTESIAN_POINT('Ctrl Pts',(6.25506922963065,-21.2520564663921,5.08792887894081));
#55728=CARTESIAN_POINT('Ctrl Pts',(6.25506922963065,-19.4765247042674,4.38283542023071));
#55729=CARTESIAN_POINT('Ctrl Pts',(6.25506922963065,-17.6131791291381,3.96792159232686));
#55730=CARTESIAN_POINT('Ctrl Pts',(6.25506922963065,-15.9632277038415,3.8699038430408));
#55731=CARTESIAN_POINT('Ctrl Pts',(6.25506922963065,-14.9505138389429,3.93797013410656));
#55732=CARTESIAN_POINT('Ctrl Pts',(6.25506922963065,-14.5721371024931,3.9816812510631));
#55733=CARTESIAN_POINT('',(7.00000000000001,-24.7867247203242,9.3325097692458));
#55734=CARTESIAN_POINT('Ctrl Pts',(7.00000000000006,-24.7867247293774,9.3325097625576));
#55735=CARTESIAN_POINT('Ctrl Pts',(7.00000000000006,-24.6891841466124,9.20047771820845));
#55736=CARTESIAN_POINT('Ctrl Pts',(7.00000000006096,-24.5890317764085,9.07102172536068));
#55737=CARTESIAN_POINT('Ctrl Pts',(6.99999999867112,-24.4862334316389,8.94403929589311));
#55738=CARTESIAN_POINT('Ctrl Pts',(6.99999999727842,-24.3832240272285,8.81679615341495));
#55739=CARTESIAN_POINT('Ctrl Pts',(6.99999999421911,-24.2775574615185,8.69203640523486));
#55740=CARTESIAN_POINT('Ctrl Pts',(6.99999999313353,-24.1691581090645,8.56968917785705));
#55741=CARTESIAN_POINT('Ctrl Pts',(6.99999999205177,-24.0611403059592,8.44777259424111));
#55742=CARTESIAN_POINT('Ctrl Pts',(6.99999999470455,-23.9504086005632,8.3282512584488));
#55743=CARTESIAN_POINT('Ctrl Pts',(6.99999999802626,-23.8368520340605,8.21109188955697));
#55744=CARTESIAN_POINT('Ctrl Pts',(6.99999999906758,-23.8012536060717,8.17436403237392));
#55745=CARTESIAN_POINT('Ctrl Pts',(7.00000000000006,-23.7653773200082,8.13786858660161));
#55746=CARTESIAN_POINT('Ctrl Pts',(7.00000000000006,-23.7292190979857,8.10160535508103));
#55747=CARTESIAN_POINT('Ctrl Pts',(7.00000000000006,-23.7003753309043,8.07267782089671));
#55748=CARTESIAN_POINT('Ctrl Pts',(6.99999999938504,-23.6713554071327,8.04389419508844));
#55749=CARTESIAN_POINT('Ctrl Pts',(6.99999999847359,-23.6421621123814,8.01525903994437));
#55750=CARTESIAN_POINT('Ctrl Pts',(6.99999999415761,-23.5039224403086,7.8796623390377));
#55751=CARTESIAN_POINT('Ctrl Pts',(6.999999985704,-23.3617919491904,7.74739742263809));
#55752=CARTESIAN_POINT('Ctrl Pts',(6.99999998494287,-23.2160995784014,7.61883386487858));
#55753=CARTESIAN_POINT('Ctrl Pts',(6.99999998418013,-23.0700992502754,7.48999855582098));
#55754=CARTESIAN_POINT('Ctrl Pts',(6.99999998976671,-22.9205222589565,7.36488057062783));
#55755=CARTESIAN_POINT('Ctrl Pts',(6.9999999946827,-22.767738442797,7.24381675242766));
#55756=CARTESIAN_POINT('Ctrl Pts',(6.99999999757257,-22.6779242372364,7.17264919733506));
#55757=CARTESIAN_POINT('Ctrl Pts',(7.00000000000006,-22.5870025612902,7.10288195460848));
#55758=CARTESIAN_POINT('Ctrl Pts',(7.00000000000006,-22.4950541460765,7.03457718217675));
#55759=CARTESIAN_POINT('Ctrl Pts',(7.00000000000006,-22.4318690559121,6.98763952485299));
#55760=CARTESIAN_POINT('Ctrl Pts',(6.99999999889743,-22.3681959174977,6.94139789754036));
#55761=CARTESIAN_POINT('Ctrl Pts',(6.99999999756665,-22.304043965429,6.89585784795075));
#55762=CARTESIAN_POINT('Ctrl Pts',(6.99999999341031,-22.1036825049342,6.7536256858332));
#55763=CARTESIAN_POINT('Ctrl Pts',(6.99999998911108,-21.898652821419,6.61823403059507));
#55764=CARTESIAN_POINT('Ctrl Pts',(6.99999999137297,-21.6892902101513,6.48986655377202));
#55765=CARTESIAN_POINT('Ctrl Pts',(6.99999999340036,-21.5016335197964,6.37480772973475));
#55766=CARTESIAN_POINT('Ctrl Pts',(7.00000000000006,-21.3104950496311,6.26539244936196));
#55767=CARTESIAN_POINT('Ctrl Pts',(7.00000000000006,-21.1160970528281,6.16178294553015));
#55768=CARTESIAN_POINT('Ctrl Pts',(7.00000000000006,-21.0125348880333,6.10658677742867));
#55769=CARTESIAN_POINT('Ctrl Pts',(6.99999999798932,-20.9080532399373,6.05302326345818));
#55770=CARTESIAN_POINT('Ctrl Pts',(6.99999999626512,-20.8027183557833,6.00113756742284));
#55771=CARTESIAN_POINT('Ctrl Pts',(6.99999999250276,-20.5728669132141,5.88791769559971));
#55772=CARTESIAN_POINT('Ctrl Pts',(6.99999999167287,-20.3389511481081,5.78268995354166));
#55773=CARTESIAN_POINT('Ctrl Pts',(6.99999999476618,-20.1017155246842,5.68575103531911));
#55774=CARTESIAN_POINT('Ctrl Pts',(6.99999999683554,-19.943009495447,5.62090077983214));
#55775=CARTESIAN_POINT('Ctrl Pts',(7.00000000000006,-19.7828182918934,5.55975913888656));
#55776=CARTESIAN_POINT('Ctrl Pts',(7.00000000000006,-19.621370056996,5.50240303026548));
#55777=CARTESIAN_POINT('Ctrl Pts',(7.00000000000006,-19.4741199931052,5.45009096464057));
#55778=CARTESIAN_POINT('Ctrl Pts',(6.99999999705142,-19.325822246007,5.40094132587375));
#55779=CARTESIAN_POINT('Ctrl Pts',(6.99999999409848,-19.1765613925645,5.35498619481664));
#55780=CARTESIAN_POINT('Ctrl Pts',(6.99999998947438,-18.9428301888559,5.28302393645594));
#55781=CARTESIAN_POINT('Ctrl Pts',(6.99999998692793,-18.7067374602874,5.21889241441373));
#55782=CARTESIAN_POINT('Ctrl Pts',(6.99999999182273,-18.4686229513191,5.16272268300951));
#55783=CARTESIAN_POINT('Ctrl Pts',(6.99999999470013,-18.3286474621975,5.12970333588448));
#55784=CARTESIAN_POINT('Ctrl Pts',(7.00000000000006,-18.1879731692716,5.09943628849387));
#55785=CARTESIAN_POINT('Ctrl Pts',(7.00000000000006,-18.0466687179138,5.07195657342431));
#55786=CARTESIAN_POINT('Ctrl Pts',(7.00000000000006,-17.8556422214223,5.03480732834476));
#55787=CARTESIAN_POINT('Ctrl Pts',(6.99999998960242,-17.6634649798387,5.00268525153448));
#55788=CARTESIAN_POINT('Ctrl Pts',(6.99999998461919,-17.4706096574179,4.97570566154593));
#55789=CARTESIAN_POINT('Ctrl Pts',(6.99999997943812,-17.2700973511263,4.94765489404053));
#55790=CARTESIAN_POINT('Ctrl Pts',(6.99999998080614,-17.0688524595463,4.92516342212063));
#55791=CARTESIAN_POINT('Ctrl Pts',(6.99999998755749,-16.8674108909919,4.9082236915833));
#55792=CARTESIAN_POINT('Ctrl Pts',(6.99999999250501,-16.7197904556305,4.89580991614076));
#55793=CARTESIAN_POINT('Ctrl Pts',(7.00000000000006,-16.5720645451366,4.88637647464254));
#55794=CARTESIAN_POINT('Ctrl Pts',(7.00000000000006,-16.4244437708488,4.87990262774485));
#55795=CARTESIAN_POINT('Ctrl Pts',(7.00000000000006,-16.2585064874591,4.87262551805303));
#55796=CARTESIAN_POINT('Ctrl Pts',(6.99999999328001,-16.0927163640638,4.86916233119042));
#55797=CARTESIAN_POINT('Ctrl Pts',(6.9999999927155,-15.9269559837606,4.86945767505926));
#55798=CARTESIAN_POINT('Ctrl Pts',(6.9999999924927,-15.8615333271543,4.86957424200051));
#55799=CARTESIAN_POINT('Ctrl Pts',(6.99999999280525,-15.7961152191328,4.87027685618125));
#55800=CARTESIAN_POINT('Ctrl Pts',(6.9999999934186,-15.730694189542,4.87156433035057));
#55801=CARTESIAN_POINT('Ctrl Pts',(6.99999999496721,-15.5655165568815,4.87481499663831));
#55802=CARTESIAN_POINT('Ctrl Pts',(6.99999999795174,-15.4003202163135,4.8817904164755));
#55803=CARTESIAN_POINT('Ctrl Pts',(6.99999999909501,-15.2350196079666,4.89250633197123));
#55804=CARTESIAN_POINT('Ctrl Pts',(7.0000000001046,-15.0890457501804,4.90196935537002));
#55805=CARTESIAN_POINT('Ctrl Pts',(6.9999999999995,-14.9429903418779,4.91435004126209));
#55806=CARTESIAN_POINT('Ctrl Pts',(6.9999999999995,-14.7967973072039,4.92969292433615));
#55807=CARTESIAN_POINT('',(6.27159471697182,-25.5608579993274,8.76071062883475));
#55808=CARTESIAN_POINT('Origin',(5.999999877384,-24.7867246592848,9.33250977407517));
#55809=CARTESIAN_POINT('Ctrl Pts',(6.27159470456809,-25.5608577604391,8.76071047658128));
#55810=CARTESIAN_POINT('Ctrl Pts',(6.27193966902721,-25.4228903795494,8.57412214168591));
#55811=CARTESIAN_POINT('Ctrl Pts',(6.27225782571643,-25.2809102066271,8.39339828302729));
#55812=CARTESIAN_POINT('Ctrl Pts',(6.27254917034726,-25.1354917711551,8.21861676875514));
#55813=CARTESIAN_POINT('Ctrl Pts',(6.27284515826659,-24.987755737636,8.04104968403698));
#55814=CARTESIAN_POINT('Ctrl Pts',(6.27311347269038,-24.8364709624808,7.86961580871584));
#55815=CARTESIAN_POINT('Ctrl Pts',(6.2733541100562,-24.6822005684409,7.70435943122668));
#55816=CARTESIAN_POINT('Ctrl Pts',(6.27354178927972,-24.5618811506001,7.57547176449234));
#55817=CARTESIAN_POINT('Ctrl Pts',(6.27371263301604,-24.4397448251206,7.45034099904443));
#55818=CARTESIAN_POINT('Ctrl Pts',(6.27386663993444,-24.3160426977393,7.32897316278893));
#55819=CARTESIAN_POINT('Ctrl Pts',(6.27406868999589,-24.1537511416417,7.16974409031388));
#55820=CARTESIAN_POINT('Ctrl Pts',(6.27424176008809,-23.9887664762674,7.01699206659435));
#55821=CARTESIAN_POINT('Ctrl Pts',(6.27438584795811,-23.8216766750998,6.87061872315646));
#55822=CARTESIAN_POINT('Ctrl Pts',(6.27447252017228,-23.7211682629063,6.78257174342696));
#55823=CARTESIAN_POINT('Ctrl Pts',(6.2745487057562,-23.6198972280055,6.69683229111827));
#55824=CARTESIAN_POINT('Ctrl Pts',(6.2746144043585,-23.5179834667241,6.61337488456931));
#55825=CARTESIAN_POINT('Ctrl Pts',(6.27472591341892,-23.3450070659173,6.47172412392615));
#55826=CARTESIAN_POINT('Ctrl Pts',(6.27480721189808,-23.1701816572621,6.33664862667355));
#55827=CARTESIAN_POINT('Ctrl Pts',(6.27485829873449,-22.9940551698525,6.2080049654047));
#55828=CARTESIAN_POINT('Ctrl Pts',(6.27487121299898,-22.9495320753769,6.17548507604218));
#55829=CARTESIAN_POINT('Ctrl Pts',(6.27488219665249,-22.9049256033793,6.14337608661024));
#55830=CARTESIAN_POINT('Ctrl Pts',(6.27489124968589,-22.8602441341368,6.1116754534218));
#55831=CARTESIAN_POINT('Ctrl Pts',(6.27492812707301,-22.6782348822084,5.98254343001002));
#55832=CARTESIAN_POINT('Ctrl Pts',(6.27493296908659,-22.4949851869132,5.8601886507752));
#55833=CARTESIAN_POINT('Ctrl Pts',(6.27490577566025,-22.311038116279,5.74438505749212));
#55834=CARTESIAN_POINT('Ctrl Pts',(6.27488257629484,-22.1541084505275,5.64559022958816));
#55835=CARTESIAN_POINT('Ctrl Pts',(6.27483606089023,-21.9966702918831,5.55156316095694));
#55836=CARTESIAN_POINT('Ctrl Pts',(6.27476622991235,-21.8390323265443,5.46215438396946));
#55837=CARTESIAN_POINT('Ctrl Pts',(6.27472435194508,-21.7444960941419,5.40853551809573));
#55838=CARTESIAN_POINT('Ctrl Pts',(6.27467408870909,-21.6498875057298,5.35657744466591));
#55839=CARTESIAN_POINT('Ctrl Pts',(6.27461544171774,-21.5552687891301,5.30624659367549));
#55840=CARTESIAN_POINT('Ctrl Pts',(6.27458611822207,-21.5079594308303,5.28108116818028));
#55841=CARTESIAN_POINT('Ctrl Pts',(6.27455469615558,-21.4606475361946,5.25632255645321));
#55842=CARTESIAN_POINT('Ctrl Pts',(6.27452117896326,-21.4133405353867,5.23196644753487));
#55843=CARTESIAN_POINT('Ctrl Pts',(6.2745044203671,-21.3896870349827,5.2197883930757));
#55844=CARTESIAN_POINT('Ctrl Pts',(6.27448713781172,-21.3660347577391,5.20771096486579));
#55845=CARTESIAN_POINT('Ctrl Pts',(6.27446933129768,-21.3423846215274,5.19573362252721));
#55846=CARTESIAN_POINT('Ctrl Pts',(6.2744539194677,-21.3219150406985,5.18536703626652));
#55847=CARTESIAN_POINT('Ctrl Pts',(6.27443872981217,-21.3022173582447,5.17546074478448));
#55848=CARTESIAN_POINT('Ctrl Pts',(6.27442216608405,-21.2812921796582,5.16501365511446));
#55849=CARTESIAN_POINT('Ctrl Pts',(6.27441959241852,-21.2780408336758,5.16339039044863));
#55850=CARTESIAN_POINT('Ctrl Pts',(6.27441698557903,-21.2747598068533,5.16175416025187));
#55851=CARTESIAN_POINT('Ctrl Pts',(6.27441433957761,-21.2714415474909,5.16010131199954));
#55852=CARTESIAN_POINT('Ctrl Pts',(6.2744027961717,-21.2569653592138,5.15289062112795));
#55853=CARTESIAN_POINT('Ctrl Pts',(6.27439106289382,-21.2424654770366,5.14570487885345));
#55854=CARTESIAN_POINT('Ctrl Pts',(6.27437913974498,-21.2279419562817,5.13854426366239));
#55855=CARTESIAN_POINT('Ctrl Pts',(6.27420010632505,-21.0098623512413,5.03102321838198));
#55856=CARTESIAN_POINT('Ctrl Pts',(6.27397826279242,-20.7864492528495,4.92916545629279));
#55857=CARTESIAN_POINT('Ctrl Pts',(6.27371361342478,-20.557965514843,4.83351364503586));
#55858=CARTESIAN_POINT('Ctrl Pts',(6.27345238602023,-20.3324361119388,4.73909862859882));
#55859=CARTESIAN_POINT('Ctrl Pts',(6.27314945258748,-20.1019663004246,4.65073011011745));
#55860=CARTESIAN_POINT('Ctrl Pts',(6.27280481907884,-19.8668531444355,4.56895455785876));
#55861=CARTESIAN_POINT('Ctrl Pts',(6.27260797682087,-19.7325649706386,4.52224730522605));
#55862=CARTESIAN_POINT('Ctrl Pts',(6.27239753085122,-19.5967628237501,4.47769131674242));
#55863=CARTESIAN_POINT('Ctrl Pts',(6.27217348257728,-19.459508772695,4.43539209668543));
#55864=CARTESIAN_POINT('Ctrl Pts',(6.271770135294,-19.2124144852199,4.35924209921435));
#55865=CARTESIAN_POINT('Ctrl Pts',(6.27132270318547,-18.9606112060094,4.29040494719483));
#55866=CARTESIAN_POINT('Ctrl Pts',(6.27083119645392,-18.7045321058939,4.22947048310928));
#55867=CARTESIAN_POINT('Ctrl Pts',(6.27036732592469,-18.46285169733,4.17196221254298));
#55868=CARTESIAN_POINT('Ctrl Pts',(6.26986419915261,-18.2173631494559,4.12149308400121));
#55869=CARTESIAN_POINT('Ctrl Pts',(6.26932182605469,-17.9684785610763,4.07857896905072));
#55870=CARTESIAN_POINT('Ctrl Pts',(6.26905885374381,-17.8478056228359,4.05777184564955));
#55871=CARTESIAN_POINT('Ctrl Pts',(6.26878665527169,-17.7263350402975,4.03874108335308));
#55872=CARTESIAN_POINT('Ctrl Pts',(6.26850523199004,-17.6041178805849,4.02154717118703));
#55873=CARTESIAN_POINT('Ctrl Pts',(6.26791730977991,-17.3487936507139,3.98562731842176));
#55874=CARTESIAN_POINT('Ctrl Pts',(6.26728912705079,-17.090207808471,3.95772398693753));
#55875=CARTESIAN_POINT('Ctrl Pts',(6.26662069841196,-16.8288453305975,3.93824738933384));
#55876=CARTESIAN_POINT('Ctrl Pts',(6.26595958210327,-16.5703420490729,3.91898385757345));
#55877=CARTESIAN_POINT('Ctrl Pts',(6.26525909558954,-16.3091225019333,3.90796371089906));
#55878=CARTESIAN_POINT('Ctrl Pts',(6.2645192563654,-16.0457065940275,3.90559011833706));
#55879=CARTESIAN_POINT('Ctrl Pts',(6.26430324577284,-15.9687971460041,3.90489710136923));
#55880=CARTESIAN_POINT('Ctrl Pts',(6.26408388053192,-15.8917008014357,3.90494121137407));
#55881=CARTESIAN_POINT('Ctrl Pts',(6.26386116113799,-15.8144313373356,3.90573258303281));
#55882=CARTESIAN_POINT('Ctrl Pts',(6.99999999998952,-24.1259274559597,10.9278021978186));
#55883=CARTESIAN_POINT('Ctrl Pts',(6.99999999998952,-24.1259309536957,10.9277942568591));
#55884=CARTESIAN_POINT('Ctrl Pts',(6.99999999998951,-24.2426238189736,10.6628645501556));
#55885=CARTESIAN_POINT('Ctrl Pts',(6.99999999998952,-24.4687760835905,10.1334756387629));
#55886=CARTESIAN_POINT('Ctrl Pts',(6.99999999998952,-24.6831198888034,9.59921869200081));
#55887=CARTESIAN_POINT('Ctrl Pts',(6.99999999998952,-24.7867214499183,9.3325057406461));
#55888=CARTESIAN_POINT('Ctrl Pts',(7.00000270572098,-24.6668575634642,11.1660644378209));
#55889=CARTESIAN_POINT('Ctrl Pts',(7.00000270572098,-24.6668611143903,11.166056376103));
#55890=CARTESIAN_POINT('Ctrl Pts',(7.00000270572098,-24.7853285323176,10.8970978743295));
#55891=CARTESIAN_POINT('Ctrl Pts',(7.00000270572098,-25.0149163654532,10.3596666804281));
#55892=CARTESIAN_POINT('Ctrl Pts',(7.00000270572098,-25.2325164806272,9.81729343793396));
#55893=CARTESIAN_POINT('Ctrl Pts',(7.00000270572098,-25.3376935135448,9.54652457474008));
#55894=CARTESIAN_POINT('Ctrl Pts',(6.57967197783012,-25.0472372157093,11.3336093881579));
#55895=CARTESIAN_POINT('Ctrl Pts',(6.57967197783012,-25.0472408040386,11.3336012415232));
#55896=CARTESIAN_POINT('Ctrl Pts',(6.57967197783013,-25.1669560795239,11.0618097089269));
#55897=CARTESIAN_POINT('Ctrl Pts',(6.57967197783013,-25.3989597892029,10.5187232176258));
#55898=CARTESIAN_POINT('Ctrl Pts',(6.57967197783013,-25.6188497270954,9.97064263198274));
#55899=CARTESIAN_POINT('Ctrl Pts',(6.57967197783013,-25.725134624792,9.69702166956874));
#55900=CARTESIAN_POINT('Ctrl Pts',(5.98852435812812,-25.041028565088,11.3308746781035));
#55901=CARTESIAN_POINT('Ctrl Pts',(5.98852435812812,-25.0410321528068,11.3308665328549));
#55902=CARTESIAN_POINT('Ctrl Pts',(5.98852435812812,-25.1607270604577,11.0591212416852));
#55903=CARTESIAN_POINT('Ctrl Pts',(5.98852435812812,-25.3926913375983,10.5161270575494));
#55904=CARTESIAN_POINT('Ctrl Pts',(5.98852435812812,-25.612543900438,9.96813962856901));
#55905=CARTESIAN_POINT('Ctrl Pts',(5.98852435812812,-25.7188107152924,9.69456521882008));
#55906=CARTESIAN_POINT('',(6.99999999994034,-24.1259366382796,10.9277762174568));
#55907=CARTESIAN_POINT('',(5.98852583803503,-25.0410393004634,11.3308502321861));
#55908=CARTESIAN_POINT('Origin',(5.999999999061,-24.1259421376201,10.9277802195584));
#55909=CARTESIAN_POINT('',(5.98852581355429,-25.7188095579012,9.69456736137508));
#55910=CARTESIAN_POINT('Origin',(5.98846824183665,11.4751154476891,-4.75314848428435));
#55911=CARTESIAN_POINT('Origin',(6.,-24.7867247762541,9.33250981979305));
#55912=CARTESIAN_POINT('Origin',(6.99999997875368,11.466399700858,-4.74964867790657));
#55913=CARTESIAN_POINT('Origin',(5.999999877384,-24.7867246592848,9.33250977407517));
#55914=CARTESIAN_POINT('Origin',(5.99999764419348,-24.7867226422921,9.33250908124204));
#55915=CARTESIAN_POINT('Ctrl Pts',(-6.09469640311948,-25.6962418117966,
9.7551784065007));
#55916=CARTESIAN_POINT('Ctrl Pts',(-6.05660168697869,-25.7007415434035,
9.74233001812424));
#55917=CARTESIAN_POINT('Ctrl Pts',(-5.71257762314107,-25.7410984324824,
9.6273925641447));
#55918=CARTESIAN_POINT('Ctrl Pts',(-5.02644182509294,-25.8164780718308,
9.41768044975332));
#55919=CARTESIAN_POINT('Ctrl Pts',(-3.98600488143526,-25.9134384022202,
9.15524677412187));
#55920=CARTESIAN_POINT('Ctrl Pts',(-2.8123888149195,-25.9986878426019,8.92978553974035));
#55921=CARTESIAN_POINT('Ctrl Pts',(-1.5205631427427,-26.0604307224869,8.77036250541219));
#55922=CARTESIAN_POINT('Ctrl Pts',(-0.189421525835868,-26.0860723981169,
8.70665832164758));
#55923=CARTESIAN_POINT('Ctrl Pts',(1.08612112080106,-26.0718380483953,8.74173357669442));
#55924=CARTESIAN_POINT('Ctrl Pts',(2.24134091421009,-26.0285585011884,8.85233532810853));
#55925=CARTESIAN_POINT('Ctrl Pts',(3.27311180245308,-25.9668527571587,9.01365179906474));
#55926=CARTESIAN_POINT('Ctrl Pts',(4.20014655779273,-25.8939006521098,9.20794869621394));
#55927=CARTESIAN_POINT('Ctrl Pts',(5.05723014173037,-25.8125878936172,9.4287012924232));
#55928=CARTESIAN_POINT('Ctrl Pts',(5.68071122126434,-25.7446165392363,9.61762164998467));
#55929=CARTESIAN_POINT('Ctrl Pts',(6.02262167191654,-25.7047562746841,9.73086139421362));
#55930=CARTESIAN_POINT('Ctrl Pts',(6.09456166924508,-25.6962600629342,9.75512415601962));
#55931=CARTESIAN_POINT('Ctrl Pts',(-6.21867431498588,-25.8360125710361,
9.42697393428334));
#55932=CARTESIAN_POINT('Ctrl Pts',(-6.17985088714009,-25.8404824786046,
9.41383765250037));
#55933=CARTESIAN_POINT('Ctrl Pts',(-5.82924224916864,-25.8805416875889,
9.29631173738694));
#55934=CARTESIAN_POINT('Ctrl Pts',(-5.12989137233682,-25.9548390426123,
9.08164968448808));
#55935=CARTESIAN_POINT('Ctrl Pts',(-4.06887094891187,-26.0493410505566,
8.81251246578824));
#55936=CARTESIAN_POINT('Ctrl Pts',(-2.87132776045126,-26.1315203199728,
8.5808712554897));
#55937=CARTESIAN_POINT('Ctrl Pts',(-1.55248691671686,-26.1902927337396,
8.41678346782181));
#55938=CARTESIAN_POINT('Ctrl Pts',(-0.19335884440114,-26.2142179075024,
8.35106522395349));
#55939=CARTESIAN_POINT('Ctrl Pts',(1.108874349186,-26.2009903666146,8.38726562889104));
#55940=CARTESIAN_POINT('Ctrl Pts',(2.28838573698317,-26.1600181790614,8.50117758368943));
#55941=CARTESIAN_POINT('Ctrl Pts',(3.34148469930592,-26.100892207404,8.66706320406161));
#55942=CARTESIAN_POINT('Ctrl Pts',(4.2872641912706,-26.0303266009707,8.86657455129211));
#55943=CARTESIAN_POINT('Ctrl Pts',(5.16125575357753,-25.9509728497055,9.09291528453062));
#55944=CARTESIAN_POINT('Ctrl Pts',(5.79676396111412,-25.8840139145535,9.2863126503946));
#55945=CARTESIAN_POINT('Ctrl Pts',(6.14522058517763,-25.844468417588,9.40211094159923));
#55946=CARTESIAN_POINT('Ctrl Pts',(6.21853693462757,-25.8360280913984,9.42691729984634));
#55947=CARTESIAN_POINT('Ctrl Pts',(-6.32919761543151,-25.7772858661747,
9.07051004505295));
#55948=CARTESIAN_POINT('Ctrl Pts',(-6.28967065067404,-25.7817133140807,
9.05716267819206));
#55949=CARTESIAN_POINT('Ctrl Pts',(-5.93271715893866,-25.8213579419598,
8.9377585934402));
#55950=CARTESIAN_POINT('Ctrl Pts',(-5.22084676055086,-25.8942953190302,
8.71984047487983));
#55951=CARTESIAN_POINT('Ctrl Pts',(-4.14083391245333,-25.9858860937408,
8.4469072451494));
#55952=CARTESIAN_POINT('Ctrl Pts',(-2.9218247883032,-26.064533180692,8.21226132360347));
#55953=CARTESIAN_POINT('Ctrl Pts',(-1.57942699571631,-26.1199617139831,
8.04629578965705));
#55954=CARTESIAN_POINT('Ctrl Pts',(-0.19662764179811,-26.1419937501351,
7.98000626123406));
#55955=CARTESIAN_POINT('Ctrl Pts',(1.1279836696488,-26.1298735851424,8.01650033217842));
#55956=CARTESIAN_POINT('Ctrl Pts',(2.32846860320679,-26.0914804388835,8.13163211550858));
#55957=CARTESIAN_POINT('Ctrl Pts',(3.40040463577914,-26.0352882674276,8.2995525215612));
#55958=CARTESIAN_POINT('Ctrl Pts',(4.36313923323556,-25.9674885931878,8.50172441513352));
#55959=CARTESIAN_POINT('Ctrl Pts',(5.25277086508226,-25.8904646791243,8.73128493448436));
#55960=CARTESIAN_POINT('Ctrl Pts',(5.89966040962877,-25.8247715602233,8.92760803942481));
#55961=CARTESIAN_POINT('Ctrl Pts',(6.25441184426259,-25.7856590242105,9.0452475831158));
#55962=CARTESIAN_POINT('Ctrl Pts',(6.32905697510172,-25.7772984101985,9.07045271479765));
#55963=CARTESIAN_POINT('Ctrl Pts',(-6.39488356510505,-25.5363210851819,
8.78685862229896));
#55964=CARTESIAN_POINT('Ctrl Pts',(-6.35487788300617,-25.5407054580702,
8.77343701897817));
#55965=CARTESIAN_POINT('Ctrl Pts',(-5.99361978169661,-25.5799359843783,
8.6533993304153));
#55966=CARTESIAN_POINT('Ctrl Pts',(-5.27347862179922,-25.6516209548836,
8.43484619237215));
#55967=CARTESIAN_POINT('Ctrl Pts',(-4.18145578460061,-25.7406725883865,
8.16210729422091));
#55968=CARTESIAN_POINT('Ctrl Pts',(-2.94953678778058,-25.8163266294645,
7.92849078581892));
#55969=CARTESIAN_POINT('Ctrl Pts',(-1.59373038385119,-25.8689857738098,
7.76397286656282));
#55970=CARTESIAN_POINT('Ctrl Pts',(-0.198299206200063,-25.8894847637204,
7.69871982059602));
#55971=CARTESIAN_POINT('Ctrl Pts',(1.13802038687766,-25.878258581833,7.73459107892983));
#55972=CARTESIAN_POINT('Ctrl Pts',(2.35020389933381,-25.841985032254,7.84850202252168));
#55973=CARTESIAN_POINT('Ctrl Pts',(3.43313687205662,-25.7882490837982,8.01534045536797));
#55974=CARTESIAN_POINT('Ctrl Pts',(4.40622315056078,-25.7228108459456,8.21685902817043));
#55975=CARTESIAN_POINT('Ctrl Pts',(5.3057872814089,-25.6478273726657,8.44635273790059));
#55976=CARTESIAN_POINT('Ctrl Pts',(5.96018217347372,-25.5832948665882,8.64321714159226));
#55977=CARTESIAN_POINT('Ctrl Pts',(6.31919070575898,-25.5446108926227,8.76145682819641));
#55978=CARTESIAN_POINT('Ctrl Pts',(6.39473997492991,-25.5363312511989,8.78680248516681));
#55979=CARTESIAN_POINT('',(-5.98852245733359,-25.7188096065167,9.69456809190346));
#55980=CARTESIAN_POINT('Ctrl Pts',(-5.98852261948844,-25.7188097472697,
9.69456765143706));
#55981=CARTESIAN_POINT('Ctrl Pts',(-5.87205076808918,-25.7323508459181,
9.65601640935633));
#55982=CARTESIAN_POINT('Ctrl Pts',(-5.74888355778406,-25.746373594707,9.61637880011002));
#55983=CARTESIAN_POINT('Ctrl Pts',(-5.61901871697422,-25.7607490246833,
9.5760400312444));
#55984=CARTESIAN_POINT('Ctrl Pts',(-5.51146429426311,-25.7726547958118,
9.54263135056406));
#55985=CARTESIAN_POINT('Ctrl Pts',(-5.39931579746942,-25.7848021023116,
9.50874244458172));
#55986=CARTESIAN_POINT('Ctrl Pts',(-5.28257497451045,-25.7971025206909,
9.47461444800713));
#55987=CARTESIAN_POINT('Ctrl Pts',(-5.21037293139857,-25.8047101023029,
9.45350691237782));
#55988=CARTESIAN_POINT('Ctrl Pts',(-5.13641382824573,-25.8123749355037,
9.43231101177835));
#55989=CARTESIAN_POINT('Ctrl Pts',(-5.06069778882864,-25.8200705226206,
9.41109484794326));
#55990=CARTESIAN_POINT('Ctrl Pts',(-5.00129388444668,-25.8261081855091,
9.39444945843907));
#55991=CARTESIAN_POINT('Ctrl Pts',(-4.94080854949479,-25.8321647187785,
9.377791649925));
#55992=CARTESIAN_POINT('Ctrl Pts',(-4.87924165198486,-25.8382274288517,
9.36115618324037));
#55993=CARTESIAN_POINT('Ctrl Pts',(-4.8092217112253,-25.8451225399803,9.34223669177861));
#55994=CARTESIAN_POINT('Ctrl Pts',(-4.73780290849893,-25.8520255508772,
9.32334635625624));
#55995=CARTESIAN_POINT('Ctrl Pts',(-4.66498524299772,-25.8589160889116,
9.30453992876295));
#55996=CARTESIAN_POINT('Ctrl Pts',(-4.62857641024712,-25.8623613579288,
9.2951367150163));
#55997=CARTESIAN_POINT('Ctrl Pts',(-4.59181786184596,-25.8658035036575,
9.28575447631326));
#55998=CARTESIAN_POINT('Ctrl Pts',(-4.55470959785817,-25.8692398176418,
9.27640039284914));
#55999=CARTESIAN_POINT('Ctrl Pts',(-4.53615546586427,-25.8709579746339,
9.27172335111707));
#56000=CARTESIAN_POINT('Ctrl Pts',(-4.51751390497513,-25.8726746733591,
9.26705334806893));
#56001=CARTESIAN_POINT('Ctrl Pts',(-4.49878491520425,-25.8743895701679,
9.26239128860525));
#56002=CARTESIAN_POINT('Ctrl Pts',(-4.4894204203188,-25.8752470185724,9.26006025887341));
#56003=CARTESIAN_POINT('Ctrl Pts',(-4.48003406821296,-25.8761040164758,
9.25773121502947));
#56004=CARTESIAN_POINT('Ctrl Pts',(-4.47062585888851,-25.8769605203525,
9.25540427130754));
#56005=CARTESIAN_POINT('Ctrl Pts',(-4.46121764956405,-25.8778170242292,
9.25307732758562));
#56006=CARTESIAN_POINT('Ctrl Pts',(-4.45054315232633,-25.8787856647035,
9.25044668891445));
#56007=CARTESIAN_POINT('Ctrl Pts',(-4.44233565926112,-25.8795285061608,
9.24842985504751));
#56008=CARTESIAN_POINT('Ctrl Pts',(-4.30838925356762,-25.8916516895023,
9.21551509712931));
#56009=CARTESIAN_POINT('Ctrl Pts',(-4.17012435788879,-25.9037024484591,
9.18295084365975));
#56010=CARTESIAN_POINT('Ctrl Pts',(-4.02753309951194,-25.9155531876057,
9.15106007112726));
#56011=CARTESIAN_POINT('Ctrl Pts',(-3.8905339033088,-25.9269391712625,9.12041997261784));
#56012=CARTESIAN_POINT('Ctrl Pts',(-3.74954081454694,-25.9381402957922,
9.09040173486523));
#56013=CARTESIAN_POINT('Ctrl Pts',(-3.60456156897667,-25.9490391261433,
9.06130964661601));
#56014=CARTESIAN_POINT('Ctrl Pts',(-3.45662342664788,-25.960160391876,9.03162381486039));
#56015=CARTESIAN_POINT('Ctrl Pts',(-3.30453072157153,-25.9709665875444,
9.00290331842774));
#56016=CARTESIAN_POINT('Ctrl Pts',(-3.14828345387676,-25.9813235521379,
8.97548872364016));
#56017=CARTESIAN_POINT('Ctrl Pts',(-3.07015982002938,-25.9865020344347,
8.96178142624636));
#56018=CARTESIAN_POINT('Ctrl Pts',(-2.99099754541688,-25.9915680760911,
8.94840082530653));
#56019=CARTESIAN_POINT('Ctrl Pts',(-2.91079662918044,-25.9965041492459,
8.93539060519317));
#56020=CARTESIAN_POINT('Ctrl Pts',(-2.89466050088125,-25.997497268944,8.9327729969313));
#56021=CARTESIAN_POINT('Ctrl Pts',(-2.87848233137155,-25.998485127942,8.93017037799633));
#56022=CARTESIAN_POINT('Ctrl Pts',(-2.86226211536348,-25.9994675784444,
8.92758311470445));
#56023=CARTESIAN_POINT('Ctrl Pts',(-2.83817290394011,-26.0009266501271,
8.92374067928837));
#56024=CARTESIAN_POINT('Ctrl Pts',(-2.8139909532798,-26.0023737929314,8.91993211216811));
#56025=CARTESIAN_POINT('Ctrl Pts',(-2.78971627344246,-26.003808543257,8.91615858572895));
#56026=CARTESIAN_POINT('Ctrl Pts',(-2.76940638392122,-26.0050089554065,
8.91300139042923));
#56027=CARTESIAN_POINT('Ctrl Pts',(-2.74903157928846,-26.006200691413,8.90986872755713));
#56028=CARTESIAN_POINT('Ctrl Pts',(-2.72859185955307,-26.0073834764163,
8.90676129069268));
#56029=CARTESIAN_POINT('Ctrl Pts',(-2.71837199968538,-26.007974868918,8.90520757226045));
#56030=CARTESIAN_POINT('Ctrl Pts',(-2.70813591104199,-26.0085640236571,
8.90366016032589));
#56031=CARTESIAN_POINT('Ctrl Pts',(-2.69788359362411,-26.0091509061281,
8.90211914177612));
#56032=CARTESIAN_POINT('Ctrl Pts',(-2.68763127620623,-26.0097377885991,
8.90057812322635));
#56033=CARTESIAN_POINT('Ctrl Pts',(-2.67595577371932,-26.0104020578559,
8.89883444796471));
#56034=CARTESIAN_POINT('Ctrl Pts',(-2.66707795504813,-26.0109047021626,
8.8975153532073));
#56035=CARTESIAN_POINT('Ctrl Pts',(-2.48139215827501,-26.0214178599607,
8.8699255622776));
#56036=CARTESIAN_POINT('Ctrl Pts',(-2.29080876604695,-26.0311760156796,
8.84445328322325));
#56037=CARTESIAN_POINT('Ctrl Pts',(-2.09532194105447,-26.0399856650684,
8.82157126467362));
#56038=CARTESIAN_POINT('Ctrl Pts',(-1.9917234742176,-26.0446543488535,8.80944491273167));
#56039=CARTESIAN_POINT('Ctrl Pts',(-1.88674823703957,-26.0490562995372,
8.79804672030007));
#56040=CARTESIAN_POINT('Ctrl Pts',(-1.780397909139,-26.0531602706882,8.78745187647168));
#56041=CARTESIAN_POINT('Ctrl Pts',(-1.69972470653747,-26.0562733828212,
8.77941504198727));
#56042=CARTESIAN_POINT('Ctrl Pts',(-1.61826034686804,-26.0592154388561,
8.77183925424756));
#56043=CARTESIAN_POINT('Ctrl Pts',(-1.53600337413081,-26.0619732073235,
8.76475545687387));
#56044=CARTESIAN_POINT('Ctrl Pts',(-1.46173164277354,-26.0644632605304,
8.75835933168204));
#56045=CARTESIAN_POINT('Ctrl Pts',(-1.38681370638488,-26.0668030643981,
8.75236433646886));
#56046=CARTESIAN_POINT('Ctrl Pts',(-1.3112508292327,-26.0689820755537,8.7467928800968));
#56047=CARTESIAN_POINT('Ctrl Pts',(-1.231625923349,-26.071278223672,8.74092191930256));
#56048=CARTESIAN_POINT('Ctrl Pts',(-1.15128415269192,-26.0733958218917,
8.73552129254775));
#56049=CARTESIAN_POINT('Ctrl Pts',(-1.07022551571206,-26.0753224370171,
8.73061668494928));
#56050=CARTESIAN_POINT('Ctrl Pts',(-1.02969619722213,-26.0762857445798,
8.72816438115004));
#56051=CARTESIAN_POINT('Ctrl Pts',(-0.98898766215019,-26.0772013021562,
8.72583608075884));
#56052=CARTESIAN_POINT('Ctrl Pts',(-0.948099910399618,-26.0780675402656,
8.72363495437701));
#56053=CARTESIAN_POINT('Ctrl Pts',(-0.927656034524333,-26.0785006593203,
8.7225343911861));
#56054=CARTESIAN_POINT('Ctrl Pts',(-0.907167354479833,-26.0789214482325,
8.72146562140689));
#56055=CARTESIAN_POINT('Ctrl Pts',(-0.886633870263706,-26.0793297099792,
8.72042903833157));
#56056=CARTESIAN_POINT('Ctrl Pts',(-0.876367128155643,-26.0795338408526,
8.71991074679392));
#56057=CARTESIAN_POINT('Ctrl Pts',(-0.866089185004711,-26.079734839917,
8.71940050192643));
#56058=CARTESIAN_POINT('Ctrl Pts',(-0.855800040811281,-26.079932682501,
8.7188983526701));
#56059=CARTESIAN_POINT('Ctrl Pts',(-0.845510896617851,-26.0801305250849,
8.71839620341376));
#56060=CARTESIAN_POINT('Ctrl Pts',(-0.833523570718007,-26.0803565416018,
8.71782265449286));
#56061=CARTESIAN_POINT('Ctrl Pts',(-0.824899005104173,-26.0805167160892,
8.71741624059158));
#56062=CARTESIAN_POINT('Ctrl Pts',(-0.603175520651301,-26.0846345403429,
8.70696800350271));
#56063=CARTESIAN_POINT('Ctrl Pts',(-0.379356108570173,-26.0871465246656,
8.70066472775404));
#56064=CARTESIAN_POINT('Ctrl Pts',(-0.153436083497702,-26.0879151272826,
8.69871721344072));
#56065=CARTESIAN_POINT('Ctrl Pts',(-0.0981464446286718,-26.0881032281873,
8.69824059627036));
#56066=CARTESIAN_POINT('Ctrl Pts',(-0.0427310278451865,-26.0881867999571,
8.69802505275581));
#56067=CARTESIAN_POINT('Ctrl Pts',(0.0128096108926353,-26.0881656968573,
8.69807222268358));
#56068=CARTESIAN_POINT('Ctrl Pts',(0.154052750421511,-26.0881120304222,
8.69819217860849));
#56069=CARTESIAN_POINT('Ctrl Pts',(0.296108408152308,-26.0873798254852,
8.7000158483331));
#56070=CARTESIAN_POINT('Ctrl Pts',(0.438976598234224,-26.0859626567222,
8.70358283824473));
#56071=CARTESIAN_POINT('Ctrl Pts',(0.510410693275183,-26.0852540723408,
8.70536633320055));
#56072=CARTESIAN_POINT('Ctrl Pts',(0.582047920928446,-26.0843742507233,
8.70758565970145));
#56073=CARTESIAN_POINT('Ctrl Pts',(0.653888281158019,-26.0833228711942,
8.71024444189027));
#56074=CARTESIAN_POINT('Ctrl Pts',(0.689808461272805,-26.0827971814297,
8.71157383298468));
#56075=CARTESIAN_POINT('Ctrl Pts',(0.725779424517649,-26.0822286026698,
8.71301308815532));
#56076=CARTESIAN_POINT('Ctrl Pts',(0.761801170818189,-26.0816171119166,
8.71456262061539));
#56077=CARTESIAN_POINT('Ctrl Pts',(0.779812043968459,-26.0813113665399,
8.71533738684542));
#56078=CARTESIAN_POINT('Ctrl Pts',(0.797835612882008,-26.0809948932044,
8.71613972241004));
#56079=CARTESIAN_POINT('Ctrl Pts',(0.815871877547348,-26.080667690937,8.71696967412839));
#56080=CARTESIAN_POINT('Ctrl Pts',(0.833908142212687,-26.0803404886696,
8.71779962584674));
#56081=CARTESIAN_POINT('Ctrl Pts',(0.853574764293333,-26.0799713301349,
8.71873647825257));
#56082=CARTESIAN_POINT('Ctrl Pts',(0.870018758785876,-26.079653897058,8.71954242311313));
#56083=CARTESIAN_POINT('Ctrl Pts',(0.954872427155101,-26.078015891095,8.72370122880682));
#56084=CARTESIAN_POINT('Ctrl Pts',(1.0391059101382,-26.076156590501,8.72843204864025));
#56085=CARTESIAN_POINT('Ctrl Pts',(1.12271338003659,-26.0740881719382,8.73370882155194));
#56086=CARTESIAN_POINT('Ctrl Pts',(1.3402282305506,-26.0687069332157,8.74743697852737));
#56087=CARTESIAN_POINT('Ctrl Pts',(1.5535046430587,-26.0619120284224,8.76485717734693));
#56088=CARTESIAN_POINT('Ctrl Pts',(1.76254242009392,-26.0539162720016,8.78549732054007));
#56089=CARTESIAN_POINT('Ctrl Pts',(1.93919399353098,-26.0471592973887,8.80293968824389));
#56090=CARTESIAN_POINT('Ctrl Pts',(2.11281902545704,-26.0395442787905,8.82268239493087));
#56091=CARTESIAN_POINT('Ctrl Pts',(2.28342873011419,-26.0311868724098,8.84446388766023));
#56092=CARTESIAN_POINT('Ctrl Pts',(2.31456109991648,-26.0296618368524,8.84843851201034));
#56093=CARTESIAN_POINT('Ctrl Pts',(2.34559309142218,-26.0281120514085,8.85248107847408));
#56094=CARTESIAN_POINT('Ctrl Pts',(2.37652480038782,-26.0265381896921,8.85659000339911));
#56095=CARTESIAN_POINT('Ctrl Pts',(2.47723059023904,-26.0214140955968,8.86996761956882));
#56096=CARTESIAN_POINT('Ctrl Pts',(2.57774644974939,-26.0159915621639,8.88416101575656));
#56097=CARTESIAN_POINT('Ctrl Pts',(2.67730193160887,-26.0103253466226,8.89903408455566));
#56098=CARTESIAN_POINT('Ctrl Pts',(2.77899779894568,-26.0045373107131,8.91422691576128));
#56099=CARTESIAN_POINT('Ctrl Pts',(2.87969140145513,-25.9984950673453,8.93012887625942));
#56100=CARTESIAN_POINT('Ctrl Pts',(2.97857178122217,-25.9922749026816,8.94654430623396));
#56101=CARTESIAN_POINT('Ctrl Pts',(3.01268321850991,-25.990129090162,8.95220724878584));
#56102=CARTESIAN_POINT('Ctrl Pts',(3.04657896412302,-25.987962252216,8.95793087169091));
#56103=CARTESIAN_POINT('Ctrl Pts',(3.08022604339517,-25.9857779723932,8.96370583404467));
#56104=CARTESIAN_POINT('Ctrl Pts',(3.158836884694,-25.9806747634902,8.97719807940202));
#56105=CARTESIAN_POINT('Ctrl Pts',(3.23630489543888,-25.975463261375,8.99100506538785));
#56106=CARTESIAN_POINT('Ctrl Pts',(3.31262859492041,-25.970160982455,9.00508184636205));
#56107=CARTESIAN_POINT('Ctrl Pts',(3.45637318408933,-25.9601749111536,9.03159341631611));
#56108=CARTESIAN_POINT('Ctrl Pts',(3.59605850748064,-25.9498675873679,9.05906057616685));
#56109=CARTESIAN_POINT('Ctrl Pts',(3.73168881455355,-25.9393524808365,9.08719458139868));
#56110=CARTESIAN_POINT('Ctrl Pts',(3.83551160795134,-25.9313033378646,9.10873070467139));
#56111=CARTESIAN_POINT('Ctrl Pts',(3.93695723417314,-25.9231322695015,9.13065783474855));
#56112=CARTESIAN_POINT('Ctrl Pts',(4.03602569256835,-25.9148863293522,9.15285338040713));
#56113=CARTESIAN_POINT('Ctrl Pts',(4.06079280716715,-25.9128248443149,9.15840226682177));
#56114=CARTESIAN_POINT('Ctrl Pts',(4.08642489231271,-25.9106752273038,9.16419233880571));
#56115=CARTESIAN_POINT('Ctrl Pts',(4.1143843731552,-25.9083070134603,9.17057701734529));
#56116=CARTESIAN_POINT('Ctrl Pts',(4.14234385399768,-25.9059387996168,9.17696169588488));
#56117=CARTESIAN_POINT('Ctrl Pts',(4.17012474473776,-25.9035635175156,9.18337091410878));
#56118=CARTESIAN_POINT('Ctrl Pts',(4.19772704539506,-25.9011821865988,9.18980197274797));
#56119=CARTESIAN_POINT('Ctrl Pts',(4.20554193317243,-25.9005079734559,9.19162276305741));
#56120=CARTESIAN_POINT('Ctrl Pts',(4.21334250587241,-25.8998332751815,9.19344530470966));
#56121=CARTESIAN_POINT('Ctrl Pts',(4.22112876290821,-25.8991581142587,9.19526953801704));
#56122=CARTESIAN_POINT('Ctrl Pts',(4.26834485877105,-25.8950639182024,9.2063317434286));
#56123=CARTESIAN_POINT('Ctrl Pts',(4.31503452262567,-25.8909527255516,9.2174561272442));
#56124=CARTESIAN_POINT('Ctrl Pts',(4.36119776862006,-25.8868296951047,9.22862951527465));
#56125=CARTESIAN_POINT('Ctrl Pts',(4.51915676195424,-25.8727217240369,9.26686203310144));
#56126=CARTESIAN_POINT('Ctrl Pts',(4.6709530903513,-25.8584777221685,9.30566322163177));
#56127=CARTESIAN_POINT('Ctrl Pts',(4.81658449855443,-25.8442847881759,9.3445420794192));
#56128=CARTESIAN_POINT('Ctrl Pts',(4.86926930130758,-25.8391502369337,9.35860721124118));
#56129=CARTESIAN_POINT('Ctrl Pts',(4.92114738772172,-25.8340221297987,9.37268292895603));
#56130=CARTESIAN_POINT('Ctrl Pts',(4.97221904074658,-25.8289085328382,9.38674739646932));
#56131=CARTESIAN_POINT('Ctrl Pts',(5.00451866423531,-25.8256745028683,9.39564229174571));
#56132=CARTESIAN_POINT('Ctrl Pts',(5.03649568642666,-25.8224465977366,9.40453183293909));
#56133=CARTESIAN_POINT('Ctrl Pts',(5.06815007165425,-25.8192265494893,9.41341124437178));
#56134=CARTESIAN_POINT('Ctrl Pts',(5.21038871658686,-25.8047572967769,9.45331078564873));
#56135=CARTESIAN_POINT('Ctrl Pts',(5.34611257561003,-25.7904491258196,9.49300242145934));
#56136=CARTESIAN_POINT('Ctrl Pts',(5.47532119496024,-25.7764528364258,9.53208334850019));
#56137=CARTESIAN_POINT('Ctrl Pts',(5.60704624399722,-25.7621839593494,9.57192540436887));
#56138=CARTESIAN_POINT('Ctrl Pts',(5.73199999778889,-25.7482390388816,9.61113271254057));
#56139=CARTESIAN_POINT('Ctrl Pts',(5.8501840030794,-25.7347477749795,9.6493230303475));
#56140=CARTESIAN_POINT('Ctrl Pts',(5.86232336330077,-25.7333620095205,9.65324577796201));
#56141=CARTESIAN_POINT('Ctrl Pts',(5.87439129930585,-25.7319810062009,9.65715783398083));
#56142=CARTESIAN_POINT('Ctrl Pts',(5.8863878126649,-25.7306048893156,9.66105881025516));
#56143=CARTESIAN_POINT('Ctrl Pts',(5.92102951904501,-25.7266311483079,9.67232345612738));
#56144=CARTESIAN_POINT('Ctrl Pts',(5.9550756602132,-25.7226981692095,9.68349569974831));
#56145=CARTESIAN_POINT('Ctrl Pts',(5.9885258216116,-25.718808932825,9.6945670296885));
#56146=CARTESIAN_POINT('',(-6.27159361730913,-25.5608563036422,8.76070973783771));
#56147=CARTESIAN_POINT('Origin',(-5.9999949808,-24.7867195890602,9.33250914740362));
#56148=CARTESIAN_POINT('Ctrl Pts',(-6.27159386306998,-25.5608571679688,
8.76070927462923));
#56149=CARTESIAN_POINT('Ctrl Pts',(-6.19708063904679,-25.5689447885619,
8.73626652820671));
#56150=CARTESIAN_POINT('Ctrl Pts',(-6.11543892371899,-25.5777035217229,
8.70997409263041));
#56151=CARTESIAN_POINT('Ctrl Pts',(-6.02658468462762,-25.5870520421337,
8.68208172051963));
#56152=CARTESIAN_POINT('Ctrl Pts',(-5.93855991912608,-25.5963132920793,
8.65444972975093));
#56153=CARTESIAN_POINT('Ctrl Pts',(-5.84345650869302,-25.6061534766376,
8.62524745406809));
#56154=CARTESIAN_POINT('Ctrl Pts',(-5.74118377300316,-25.6164754174791,
8.59476439199516));
#56155=CARTESIAN_POINT('Ctrl Pts',(-5.6404952783399,-25.6266374677882,8.56475352338832));
#56156=CARTESIAN_POINT('Ctrl Pts',(-5.53285768058784,-25.637266563283,8.53350119440277));
#56157=CARTESIAN_POINT('Ctrl Pts',(-5.41817809549367,-25.6482508438218,
8.50132997441968));
#56158=CARTESIAN_POINT('Ctrl Pts',(-5.37925184358973,-25.6519792918353,
8.49040994002917));
#56159=CARTESIAN_POINT('Ctrl Pts',(-5.3395141985331,-25.655748491532,8.47938443645545));
#56160=CARTESIAN_POINT('Ctrl Pts',(-5.29896141203056,-25.6595535226999,
8.46826733717323));
#56161=CARTESIAN_POINT('Ctrl Pts',(-5.21821293618428,-25.6671300789331,
8.4461310328575));
#56162=CARTESIAN_POINT('Ctrl Pts',(-5.13423254664718,-25.6748489226137,
8.42363083556044));
#56163=CARTESIAN_POINT('Ctrl Pts',(-5.04699089785595,-25.6826701550035,
8.40088618117009));
#56164=CARTESIAN_POINT('Ctrl Pts',(-4.92201106411443,-25.6938746237093,
8.36830285470159));
#56165=CARTESIAN_POINT('Ctrl Pts',(-4.79033815562892,-25.705289985841,8.33521556942507));
#56166=CARTESIAN_POINT('Ctrl Pts',(-4.65188625538751,-25.7167847988647,
8.30201758529982));
#56167=CARTESIAN_POINT('Ctrl Pts',(-4.51343435514609,-25.7282796118884,
8.26881960117456));
#56168=CARTESIAN_POINT('Ctrl Pts',(-4.36820326559321,-25.7398539743359,
8.23551064667246));
#56169=CARTESIAN_POINT('Ctrl Pts',(-4.21611007769853,-25.7513585178058,
8.20253712861326));
#56170=CARTESIAN_POINT('Ctrl Pts',(-4.07082689961474,-25.7623479425188,
8.1710400079167));
#56171=CARTESIAN_POINT('Ctrl Pts',(-3.91928181453819,-25.7732734603624,
8.13984920306125));
#56172=CARTESIAN_POINT('Ctrl Pts',(-3.761419633208,-25.7839929667704,8.10939932611515));
#56173=CARTESIAN_POINT('Ctrl Pts',(-3.73054600125373,-25.7860894162986,
8.10344414238486));
#56174=CARTESIAN_POINT('Ctrl Pts',(-3.69943078308636,-25.788177940232,8.09751744688045));
#56175=CARTESIAN_POINT('Ctrl Pts',(-3.66807362121464,-25.7902574078211,
8.09162271016127));
#56176=CARTESIAN_POINT('Ctrl Pts',(-3.58017497496326,-25.7960864553211,
8.0750989131498));
#56177=CARTESIAN_POINT('Ctrl Pts',(-3.49037512908124,-25.801844445895,8.05882589710281));
#56178=CARTESIAN_POINT('Ctrl Pts',(-3.39866710983025,-25.807505523488,8.04288325215432));
#56179=CARTESIAN_POINT('Ctrl Pts',(-3.35281310020476,-25.8103360622845,
8.03491192968008));
#56180=CARTESIAN_POINT('Ctrl Pts',(-3.30648203828449,-25.8131423273748,
8.02702323602364));
#56181=CARTESIAN_POINT('Ctrl Pts',(-3.25967322258879,-25.815920977859,8.01922760763646));
#56182=CARTESIAN_POINT('Ctrl Pts',(-3.23626881474094,-25.8173103031012,
8.01532979344288));
#56183=CARTESIAN_POINT('Ctrl Pts',(-3.21274496785339,-25.8186927217834,
8.01145524786678));
#56184=CARTESIAN_POINT('Ctrl Pts',(-3.18910159820844,-25.8200678035715,
8.00760529749764));
#56185=CARTESIAN_POINT('Ctrl Pts',(-3.17727991338596,-25.8207553444655,
8.00568032231307));
#56186=CARTESIAN_POINT('Ctrl Pts',(-3.16542834783943,-25.8214410509499,
8.00376149607821));
#56187=CARTESIAN_POINT('Ctrl Pts',(-3.15354689173673,-25.8221248687264,
8.00184898647939));
#56188=CARTESIAN_POINT('Ctrl Pts',(-3.14166543563402,-25.8228086865028,
7.99993647688058));
#56189=CARTESIAN_POINT('Ctrl Pts',(-3.12814004787691,-25.8235825258922,
7.99777350945494));
#56190=CARTESIAN_POINT('Ctrl Pts',(-3.11781284205206,-25.8241706010689,
7.99613057617227));
#56191=CARTESIAN_POINT('Ctrl Pts',(-3.0766201969457,-25.8265162860935,7.98957732558404));
#56192=CARTESIAN_POINT('Ctrl Pts',(-3.03568681538845,-25.8288017557171,
7.98319650478659));
#56193=CARTESIAN_POINT('Ctrl Pts',(-2.99501443262273,-25.831028571739,7.97698351883132));
#56194=CARTESIAN_POINT('Ctrl Pts',(-2.79739857890957,-25.8418480546241,
7.94679633922273));
#56195=CARTESIAN_POINT('Ctrl Pts',(-2.60594810869286,-25.8512836540238,
7.92056972156591));
#56196=CARTESIAN_POINT('Ctrl Pts',(-2.42085607247106,-25.8595191508833,
7.89776586357605));
#56197=CARTESIAN_POINT('Ctrl Pts',(-2.23092812240802,-25.8679698172016,
7.87436620743766));
#56198=CARTESIAN_POINT('Ctrl Pts',(-2.04769488441589,-25.8751569357714,
7.85457014091518));
#56199=CARTESIAN_POINT('Ctrl Pts',(-1.87131612638337,-25.8812684573676,
7.83781972802053));
#56200=CARTESIAN_POINT('Ctrl Pts',(-1.78117029277795,-25.8843920092909,
7.82925872016184));
#56201=CARTESIAN_POINT('Ctrl Pts',(-1.69281421002091,-25.8872344221247,
7.82149368573478));
#56202=CARTESIAN_POINT('Ctrl Pts',(-1.60626489564927,-25.8898196497827,
7.81445284170412));
#56203=CARTESIAN_POINT('Ctrl Pts',(-1.43907111686404,-25.8948137272552,
7.80085151709666));
#56204=CARTESIAN_POINT('Ctrl Pts',(-1.27862185686045,-25.8988490684406,
7.78995019290348));
#56205=CARTESIAN_POINT('Ctrl Pts',(-1.12501667405839,-25.9020959959412,
7.78123961020363));
#56206=CARTESIAN_POINT('Ctrl Pts',(-0.969939764400389,-25.9053740330067,
7.77244556939216));
#56207=CARTESIAN_POINT('Ctrl Pts',(-0.821838316641244,-25.9078484881115,
7.76588428017098));
#56208=CARTESIAN_POINT('Ctrl Pts',(-0.680782402076676,-25.9096791063164,
7.76107122809345));
#56209=CARTESIAN_POINT('Ctrl Pts',(-0.538388127957247,-25.9115270936998,
7.75621250905998));
#56210=CARTESIAN_POINT('Ctrl Pts',(-0.403173335643225,-25.9127189872834,
7.75313518406329));
#56211=CARTESIAN_POINT('Ctrl Pts',(-0.275183173989101,-25.9134031475166,
7.75138353240064));
#56212=CARTESIAN_POINT('Ctrl Pts',(-0.236228034117317,-25.9136113788153,
7.75085039895786));
#56213=CARTESIAN_POINT('Ctrl Pts',(-0.1979419845857,-25.9137724639869,7.75044037647808));
#56214=CARTESIAN_POINT('Ctrl Pts',(-0.160325891522733,-25.9138902918349,
7.75014142876869));
#56215=CARTESIAN_POINT('Ctrl Pts',(-0.154008553609919,-25.9139100801296,
7.75009122276523));
#56216=CARTESIAN_POINT('Ctrl Pts',(-0.147710111200664,-25.9139286480524,
7.75004415046106));
#56217=CARTESIAN_POINT('Ctrl Pts',(-0.141430567613903,-25.913946013496,
7.75000015435446));
#56218=CARTESIAN_POINT('Ctrl Pts',(-0.103047981675466,-25.9140521566614,
7.74973123602959));
#56219=CARTESIAN_POINT('Ctrl Pts',(-0.0662560356263134,-25.914112617826,
7.74957970423149));
#56220=CARTESIAN_POINT('Ctrl Pts',(-0.0289815746365708,-25.9141334372774,
7.74952611540055));
#56221=CARTESIAN_POINT('Ctrl Pts',(-0.0185593623277894,-25.9141392585485,
7.74951113157091));
#56222=CARTESIAN_POINT('Ctrl Pts',(-0.00809942559603181,-25.9141418866517,
7.7495041020777));
#56223=CARTESIAN_POINT('Ctrl Pts',(0.00244355485639335,-25.9141412348339,
7.74950529306156));
#56224=CARTESIAN_POINT('Ctrl Pts',(0.127127988062576,-25.9141335262425,
7.74951937799214));
#56225=CARTESIAN_POINT('Ctrl Pts',(0.258986421343677,-25.9136690002263,
7.75068426010729));
#56226=CARTESIAN_POINT('Ctrl Pts',(0.397985636277575,-25.9126040409567,
7.75344426793973));
#56227=CARTESIAN_POINT('Ctrl Pts',(0.535666715031177,-25.9115491807465,
7.75617810248635));
#56228=CARTESIAN_POINT('Ctrl Pts',(0.680354109440456,-25.9099051999983,
7.7604770911692));
#56229=CARTESIAN_POINT('Ctrl Pts',(0.831993583507304,-25.9075172201685,
7.76681628057526));
#56230=CARTESIAN_POINT('Ctrl Pts',(0.942261577046938,-25.9057807478808,
7.77142596219527));
#56231=CARTESIAN_POINT('Ctrl Pts',(1.05620525649912,-25.9036505489341,7.77711535741795));
#56232=CARTESIAN_POINT('Ctrl Pts',(1.17379482852109,-25.9010619875873,7.78408109758496));
#56233=CARTESIAN_POINT('Ctrl Pts',(1.33435500102349,-25.8975274917197,7.79359231889132));
#56234=CARTESIAN_POINT('Ctrl Pts',(1.50171435131308,-25.8931388014668,7.80548239116508));
#56235=CARTESIAN_POINT('Ctrl Pts',(1.67576186882429,-25.8877241846894,7.82026642896838));
#56236=CARTESIAN_POINT('Ctrl Pts',(1.84377414670226,-25.8824973241652,7.83453781820211));
#56237=CARTESIAN_POINT('Ctrl Pts',(2.01801902803007,-25.8763143723798,7.85150627903865));
#56238=CARTESIAN_POINT('Ctrl Pts',(2.19835996516099,-25.8690099414244,7.87166085380236));
#56239=CARTESIAN_POINT('Ctrl Pts',(2.26108100385463,-25.8664695226827,7.87867044288246));
#56240=CARTESIAN_POINT('Ctrl Pts',(2.32453906477803,-25.863793357096,7.88606563249174));
#56241=CARTESIAN_POINT('Ctrl Pts',(2.38872722789465,-25.860974186408,7.89386765098496));
#56242=CARTESIAN_POINT('Ctrl Pts',(2.47499317077123,-25.8571853504963,7.90435320547007));
#56243=CARTESIAN_POINT('Ctrl Pts',(2.56257788935075,-25.8531382212515,7.91557357215087));
#56244=CARTESIAN_POINT('Ctrl Pts',(2.65146471499337,-25.8488156602481,7.92757932298422));
#56245=CARTESIAN_POINT('Ctrl Pts',(2.72897727348801,-25.8450462291744,7.93804877621325));
#56246=CARTESIAN_POINT('Ctrl Pts',(2.80748002606418,-25.8410673718969,7.94911553139678));
#56247=CARTESIAN_POINT('Ctrl Pts',(2.88696068428701,-25.8368674907817,7.96081345907223));
#56248=CARTESIAN_POINT('Ctrl Pts',(2.92670101339843,-25.8347675502241,7.96666242290996));
#56249=CARTESIAN_POINT('Ctrl Pts',(2.96668581773295,-25.8326123476695,7.97266918466076));
#56250=CARTESIAN_POINT('Ctrl Pts',(3.00691344022713,-25.8304004283776,7.97883801999785));
#56251=CARTESIAN_POINT('Ctrl Pts',(3.02702725147422,-25.8292944687317,7.98192243766639));
#56252=CARTESIAN_POINT('Ctrl Pts',(3.04720176720655,-25.8281743295397,7.98504737402185));
#56253=CARTESIAN_POINT('Ctrl Pts',(3.06743677570191,-25.8270398270069,7.98821336459234));
#56254=CARTESIAN_POINT('Ctrl Pts',(3.07755427994959,-25.8264725757405,7.98979635987758));
#56255=CARTESIAN_POINT('Ctrl Pts',(3.0876869073839,-25.8259017336162,7.99138961873463));
#56256=CARTESIAN_POINT('Ctrl Pts',(3.0978346310618,-25.8253272776051,7.99299320821095));
#56257=CARTESIAN_POINT('Ctrl Pts',(3.10798235473969,-25.824752821594,7.99459679768727));
#56258=CARTESIAN_POINT('Ctrl Pts',(3.11649244049615,-25.8242692120269,7.99594695329885));
#56259=CARTESIAN_POINT('Ctrl Pts',(3.12832306372715,-25.8235930448162,7.99783503561468));
#56260=CARTESIAN_POINT('Ctrl Pts',(3.2439668548878,-25.8169835418194,8.01629095232871));
#56261=CARTESIAN_POINT('Ctrl Pts',(3.35681912047297,-25.8101925839103,8.03535399059616));
#56262=CARTESIAN_POINT('Ctrl Pts',(3.4668879598088,-25.8032672596649,8.05487798524582));
#56263=CARTESIAN_POINT('Ctrl Pts',(3.63912660834516,-25.7924303280147,8.08542965157373));
#56264=CARTESIAN_POINT('Ctrl Pts',(3.80454906828157,-25.7812653381788,8.11710708630667));
#56265=CARTESIAN_POINT('Ctrl Pts',(3.96321157962074,-25.7699424992933,8.1493898816964));
#56266=CARTESIAN_POINT('Ctrl Pts',(4.12187409095991,-25.7586196604077,8.18167267708613));
#56267=CARTESIAN_POINT('Ctrl Pts',(4.27377692490459,-25.7471388839885,8.21456112151753));
#56268=CARTESIAN_POINT('Ctrl Pts',(4.41898858671655,-25.7356525460951,8.24759161726221));
#56269=CARTESIAN_POINT('Ctrl Pts',(4.5635182889215,-25.7242201516549,8.28046699141669));
#56270=CARTESIAN_POINT('Ctrl Pts',(4.70142003179067,-25.7127823131508,8.31348335264749));
#56271=CARTESIAN_POINT('Ctrl Pts',(4.83277463773686,-25.7014759066788,8.34623482767659));
#56272=CARTESIAN_POINT('Ctrl Pts',(4.90532346773847,-25.6952312336797,8.36432388650382));
#56273=CARTESIAN_POINT('Ctrl Pts',(4.97587516450272,-25.6890263399827,8.38233303919329));
#56274=CARTESIAN_POINT('Ctrl Pts',(5.04444364874705,-25.6828820642494,8.40020028894091));
#56275=CARTESIAN_POINT('Ctrl Pts',(5.1353882843271,-25.6747327092852,8.42389820985928));
#56276=CARTESIAN_POINT('Ctrl Pts',(5.22284415433159,-25.6666901439998,8.44734605381939));
#56277=CARTESIAN_POINT('Ctrl Pts',(5.30684382899499,-25.658798954923,8.47041084629138));
#56278=CARTESIAN_POINT('Ctrl Pts',(5.42689862195449,-25.6475206365889,8.50337572259565));
#56279=CARTESIAN_POINT('Ctrl Pts',(5.53989390952036,-25.6365524409084,8.53555627122668));
#56280=CARTESIAN_POINT('Ctrl Pts',(5.64592673883416,-25.6260119626618,8.566611887455));
#56281=CARTESIAN_POINT('Ctrl Pts',(5.75378604299005,-25.6152899187768,8.59820245405778));
#56282=CARTESIAN_POINT('Ctrl Pts',(5.85444110836096,-25.6050103706137,8.62862905272502));
#56283=CARTESIAN_POINT('Ctrl Pts',(5.94798673536669,-25.5952771856988,8.65758325353552));
#56284=CARTESIAN_POINT('Ctrl Pts',(6.02496391510624,-25.5872679056435,8.68140919592692));
#56285=CARTESIAN_POINT('Ctrl Pts',(6.09712691820323,-25.5796281937042,8.70423908336207));
#56286=CARTESIAN_POINT('Ctrl Pts',(6.16452391351832,-25.5724066904849,8.72592536702089));
#56287=CARTESIAN_POINT('Ctrl Pts',(6.20165874450665,-25.5684277400839,8.73787421540308));
#56288=CARTESIAN_POINT('Ctrl Pts',(6.23734659792339,-25.5645756329308,8.7494762901245));
#56289=CARTESIAN_POINT('Ctrl Pts',(6.27159479316358,-25.5608580129633,8.76071029005059));
#56290=CARTESIAN_POINT('Ctrl Pts',(-6.390311350308,-25.6807372937616,8.98426028603872));
#56291=CARTESIAN_POINT('Ctrl Pts',(-4.260207566872,-25.9287992192441,8.2768729736642));
#56292=CARTESIAN_POINT('Ctrl Pts',(0.0001663377217942,-26.1774671700566,
7.5688746106888));
#56293=CARTESIAN_POINT('Ctrl Pts',(4.260540242316,-25.9287798010101,8.27692826056537));
#56294=CARTESIAN_POINT('Ctrl Pts',(6.390810363473,-25.680679178753,8.98442601004882));
#56295=CARTESIAN_POINT('Ctrl Pts',(-6.390311350308,-25.114983911886,8.18394866803594));
#56296=CARTESIAN_POINT('Ctrl Pts',(-4.260207566872,-25.3660579697472,7.53598941987455));
#56297=CARTESIAN_POINT('Ctrl Pts',(0.0001663377217942,-25.6190368856695,
6.88615611385154));
#56298=CARTESIAN_POINT('Ctrl Pts',(4.260540242316,-25.3660382148685,7.53604016472075));
#56299=CARTESIAN_POINT('Ctrl Pts',(6.390810363473,-25.114925091227,8.18410046945239));
#56300=CARTESIAN_POINT('Ctrl Pts',(-6.390311350308,-23.7052292153387,6.63374483955243));
#56301=CARTESIAN_POINT('Ctrl Pts',(-4.260207566872,-23.9981327197181,6.09525946370173));
#56302=CARTESIAN_POINT('Ctrl Pts',(0.0001663377217942,-24.290056533388,
5.55782023498321));
#56303=CARTESIAN_POINT('Ctrl Pts',(4.260540242316,-23.9981099236694,6.09530143180341));
#56304=CARTESIAN_POINT('Ctrl Pts',(6.390810363473,-23.7051605950053,6.63387099387303));
#56305=CARTESIAN_POINT('Ctrl Pts',(-6.390311350308,-21.0044950488243,4.89945807532427));
#56306=CARTESIAN_POINT('Ctrl Pts',(-4.260207566872,-21.4424839271908,4.44478852897079));
#56307=CARTESIAN_POINT('Ctrl Pts',(0.0001663377217941,-21.8807691943046,
3.98943207393405));
#56308=CARTESIAN_POINT('Ctrl Pts',(4.260540242316,-21.4424497019158,4.44482408731423));
#56309=CARTESIAN_POINT('Ctrl Pts',(6.390810363473,-21.0043924384536,4.89956459357196));
#56310=CARTESIAN_POINT('Ctrl Pts',(-6.390311350308,-18.1257304172683,4.0264979364763));
#56311=CARTESIAN_POINT('Ctrl Pts',(-4.260207566872,-18.7393860755884,3.53810643694032));
#56312=CARTESIAN_POINT('Ctrl Pts',(0.0001663377217945,-19.353021691043,
3.05102696824815));
#56313=CARTESIAN_POINT('Ctrl Pts',(4.260540242316,-18.7393381573803,3.53814447249922));
#56314=CARTESIAN_POINT('Ctrl Pts',(6.390810363473,-18.1255866523452,4.02661235499138));
#56315=CARTESIAN_POINT('Ctrl Pts',(-6.390311350308,-16.240127474348,3.91822579691448));
#56316=CARTESIAN_POINT('Ctrl Pts',(-4.260207566872,-16.9589011884504,3.34432563173864));
#56317=CARTESIAN_POINT('Ctrl Pts',(0.0001663377217938,-17.6776846679344,
2.76847602232095));
#56318=CARTESIAN_POINT('Ctrl Pts',(4.260540242316,-16.9588450593473,3.34437059927322));
#56319=CARTESIAN_POINT('Ctrl Pts',(6.390810363473,-16.2399590827655,3.91836024805384));
#56320=CARTESIAN_POINT('Ctrl Pts',(-6.390311350308,-15.4599864582096,3.94962394700618));
#56321=CARTESIAN_POINT('Ctrl Pts',(-4.260207566872,-16.2180942529318,3.32898458305284));
#56322=CARTESIAN_POINT('Ctrl Pts',(0.0001663377217938,-16.9762230425391,
2.70679298590865));
#56323=CARTESIAN_POINT('Ctrl Pts',(4.260540242316,-16.2180350513886,3.32903316938923));
#56324=CARTESIAN_POINT('Ctrl Pts',(6.390810363473,-15.4598088515932,3.94976934802855));
#56325=CARTESIAN_POINT('',(-6.26385951335491,-15.8144217941401,3.90574150361402));
#56326=CARTESIAN_POINT('Ctrl Pts',(-6.27159552384235,-25.5608567088111,
8.76070944182656));
#56327=CARTESIAN_POINT('Ctrl Pts',(-6.27195777355281,-25.4158727838719,
8.5645940892268));
#56328=CARTESIAN_POINT('Ctrl Pts',(-6.27229031319814,-25.2662940547189,
8.37478239185605));
#56329=CARTESIAN_POINT('Ctrl Pts',(-6.2725931430244,-25.1127469377871,8.19135374058517));
#56330=CARTESIAN_POINT('Ctrl Pts',(-6.27289863568736,-24.957849653655,8.00631216845018));
#56331=CARTESIAN_POINT('Ctrl Pts',(-6.27317389374662,-24.7989138390075,
7.82776631099681));
#56332=CARTESIAN_POINT('Ctrl Pts',(-6.27341891745478,-24.6365421570524,
7.65576240833124));
#56333=CARTESIAN_POINT('Ctrl Pts',(-6.27366754260897,-24.4717838780882,
7.48123033083415));
#56334=CARTESIAN_POINT('Ctrl Pts',(-6.2738850380896,-24.3034879748336,7.31343388118491));
#56335=CARTESIAN_POINT('Ctrl Pts',(-6.27407140416057,-24.1322430218785,
7.15238617213097));
#56336=CARTESIAN_POINT('Ctrl Pts',(-6.27421804473799,-23.9975003691542,
7.02566713511055));
#56337=CARTESIAN_POINT('Ctrl Pts',(-6.27434541248456,-23.8609310705886,
6.90312565692038));
#56338=CARTESIAN_POINT('Ctrl Pts',(-6.27445350752884,-23.7228045339352,
6.78475354198177));
#56339=CARTESIAN_POINT('Ctrl Pts',(-6.27450262987442,-23.660034778736,6.73096091923787));
#56340=CARTESIAN_POINT('Ctrl Pts',(-6.2745477721635,-23.5969432430862,6.67802913642794));
#56341=CARTESIAN_POINT('Ctrl Pts',(-6.27458893440815,-23.5335576663087,
6.62595263407767));
#56342=CARTESIAN_POINT('Ctrl Pts',(-6.27470712620839,-23.3515545833113,
6.4764220237821));
#56343=CARTESIAN_POINT('Ctrl Pts',(-6.27479250322405,-23.1671310106694,
6.33394454568465));
#56344=CARTESIAN_POINT('Ctrl Pts',(-6.27484506545512,-22.9809083449876,
6.19837392603431));
#56345=CARTESIAN_POINT('Ctrl Pts',(-6.2748976276862,-22.7946856793058,6.06280330638397));
#56346=CARTESIAN_POINT('Ctrl Pts',(-6.2749173751327,-22.6066637586169,5.93413943825559));
#56347=CARTESIAN_POINT('Ctrl Pts',(-6.27490430779461,-22.4174135710649,
5.81221558765903));
#56348=CARTESIAN_POINT('Ctrl Pts',(-6.27489476769251,-22.2792472437393,
5.72320235671738));
#56349=CARTESIAN_POINT('Ctrl Pts',(-6.27486753880225,-22.1401747709447,
5.637625073071));
#56350=CARTESIAN_POINT('Ctrl Pts',(-6.27482283830957,-22.0006690425674,
5.55559585379084));
#56351=CARTESIAN_POINT('Ctrl Pts',(-6.27477792092454,-21.8604864150119,
5.47316861851682));
#56352=CARTESIAN_POINT('Ctrl Pts',(-6.27471536197696,-21.7198666589869,
5.3943240411735));
#56353=CARTESIAN_POINT('Ctrl Pts',(-6.2746353818294,-21.5793028330079,5.31912480394626));
#56354=CARTESIAN_POINT('Ctrl Pts',(-6.27457691192168,-21.476542908408,5.26415000588831));
#56355=CARTESIAN_POINT('Ctrl Pts',(-6.27450913139656,-21.373813168866,5.21112236044329));
#56356=CARTESIAN_POINT('Ctrl Pts',(-6.2744321263511,-21.2713091288939,5.16004897734718));
#56357=CARTESIAN_POINT('Ctrl Pts',(-6.27435635466394,-21.170446854181,5.10979361572676));
#56358=CARTESIAN_POINT('Ctrl Pts',(-6.2742702475298,-21.0681861058318,5.06062331003959));
#56359=CARTESIAN_POINT('Ctrl Pts',(-6.27417380494869,-20.9645377933661,
5.01262251508626));
#56360=CARTESIAN_POINT('Ctrl Pts',(-6.27399075533888,-20.7678115865775,
4.9215162144687));
#56361=CARTESIAN_POINT('Ctrl Pts',(-6.27377047262635,-20.5660839039866,
4.83462179089819));
#56362=CARTESIAN_POINT('Ctrl Pts',(-6.27351295681112,-20.3594970637805,
4.75246067873237));
#56363=CARTESIAN_POINT('Ctrl Pts',(-6.27325823314554,-20.1551501690056,
4.67119040940841));
#56364=CARTESIAN_POINT('Ctrl Pts',(-6.27296707940982,-19.9460488030888,
4.59455135335413));
#56365=CARTESIAN_POINT('Ctrl Pts',(-6.27263949560396,-19.7323748765706,
4.52307277276017));
#56366=CARTESIAN_POINT('Ctrl Pts',(-6.27231699897039,-19.5220191729321,
4.45270420996481));
#56367=CARTESIAN_POINT('Ctrl Pts',(-6.2719591949537,-19.3072317554042,4.38733709853277));
#56368=CARTESIAN_POINT('Ctrl Pts',(-6.2715660835539,-19.0882305285998,4.32750038765547));
#56369=CARTESIAN_POINT('Ctrl Pts',(-6.2713627519632,-18.9749550859819,4.29655065276892));
#56370=CARTESIAN_POINT('Ctrl Pts',(-6.27114997445887,-18.8605530428152,
4.26708087937792));
#56371=CARTESIAN_POINT('Ctrl Pts',(-6.27092775104091,-18.7450594169863,
4.23916682997619));
#56372=CARTESIAN_POINT('Ctrl Pts',(-6.27050608312226,-18.5259107904982,
4.18620004897671));
#56373=CARTESIAN_POINT('Ctrl Pts',(-6.27005040597021,-18.3028291636747,
4.13883321537287));
#56374=CARTESIAN_POINT('Ctrl Pts',(-6.26956071910113,-18.0760881657024,
4.0976017108142));
#56375=CARTESIAN_POINT('Ctrl Pts',(-6.26938505239444,-17.9947487488252,
4.08281062068157));
#56376=CARTESIAN_POINT('Ctrl Pts',(-6.26920500900548,-17.912938840527,4.06880930124582));
#56377=CARTESIAN_POINT('Ctrl Pts',(-6.26902058891192,-17.8306725394492,
4.05562321457882));
#56378=CARTESIAN_POINT('Ctrl Pts',(-6.26850854183986,-17.6022580658327,
4.01901171016394));
#56379=CARTESIAN_POINT('Ctrl Pts',(-6.26796275434394,-17.3703215097504,
3.98868445467322));
#56380=CARTESIAN_POINT('Ctrl Pts',(-6.26738322594624,-17.135214507519,3.96507788638757));
#56381=CARTESIAN_POINT('Ctrl Pts',(-6.26681231403247,-16.903603098796,3.94182230282831));
#56382=CARTESIAN_POINT('Ctrl Pts',(-6.26620865708409,-16.6689147740032,
3.92508906956263));
#56383=CARTESIAN_POINT('Ctrl Pts',(-6.26557225464421,-16.4315352528344,
3.91530352157058));
#56384=CARTESIAN_POINT('Ctrl Pts',(-6.26502584282964,-16.2277224344459,
3.90690170111903));
#56385=CARTESIAN_POINT('Ctrl Pts',(-6.26445529152988,-16.0219264392837,
3.90362174117236));
#56386=CARTESIAN_POINT('Ctrl Pts',(-6.26386060045574,-15.8144217505232,
3.90573752921543));
#56387=CARTESIAN_POINT('Ctrl Pts',(6.2638598901157,-15.8144313886664,3.90573722905719));
#56388=CARTESIAN_POINT('Ctrl Pts',(5.97578930821615,-15.9102534412013,3.8258770779521));
#56389=CARTESIAN_POINT('Ctrl Pts',(5.68589879838239,-15.9988220577541,3.75096628482656));
#56390=CARTESIAN_POINT('Ctrl Pts',(5.39467502935807,-16.0802283700764,3.68127561885453));
#56391=CARTESIAN_POINT('Ctrl Pts',(5.12105868788167,-16.1567128460013,3.61579845975379));
#56392=CARTESIAN_POINT('Ctrl Pts',(4.84626543163589,-16.2268745751674,3.55492987257316));
#56393=CARTESIAN_POINT('Ctrl Pts',(4.57069888658429,-16.2908266780865,3.49887279692821));
#56394=CARTESIAN_POINT('Ctrl Pts',(4.31440697190754,-16.3503056213728,3.44673665955517));
#56395=CARTESIAN_POINT('Ctrl Pts',(4.05744616130298,-16.4044131426885,3.39876274702718));
#56396=CARTESIAN_POINT('Ctrl Pts',(3.80014117125608,-16.4532764068686,3.35508947292147));
#56397=CARTESIAN_POINT('Ctrl Pts',(3.57897012726198,-16.4952776877209,3.31754933960792));
#56398=CARTESIAN_POINT('Ctrl Pts',(3.35754478403803,-16.5334046032886,3.28318655458352));
#56399=CARTESIAN_POINT('Ctrl Pts',(3.1360713681052,-16.5677626949941,3.25207046795645));
#56400=CARTESIAN_POINT('Ctrl Pts',(2.89295359977274,-16.6054785650656,3.21791344054009));
#56401=CARTESIAN_POINT('Ctrl Pts',(2.64979796567082,-16.6386697226143,3.18767332756024));
#56402=CARTESIAN_POINT('Ctrl Pts',(2.40684647802523,-16.6673707732513,3.16139952179199));
#56403=CARTESIAN_POINT('Ctrl Pts',(2.16745577474301,-16.6956511709698,3.13551079436861));
#56404=CARTESIAN_POINT('Ctrl Pts',(1.92826327768186,-16.719572102414,3.1134730048344));
#56405=CARTESIAN_POINT('Ctrl Pts',(1.68950051321017,-16.7392056546265,3.09530109367423));
#56406=CARTESIAN_POINT('Ctrl Pts',(1.45234022335468,-16.7587074347468,3.0772511446903));
#56407=CARTESIAN_POINT('Ctrl Pts',(1.21560391707957,-16.7739791516685,3.06301541739025));
#56408=CARTESIAN_POINT('Ctrl Pts',(0.979518490249757,-16.7851306663667,
3.05257560488626));
#56409=CARTESIAN_POINT('Ctrl Pts',(0.745119696576639,-16.796202512808,3.04221037612153));
#56410=CARTESIAN_POINT('Ctrl Pts',(0.511362515589295,-16.8032128024522,
3.03558705246871));
#56411=CARTESIAN_POINT('Ctrl Pts',(0.278469014867348,-16.8063082581637,
3.03265442154118));
#56412=CARTESIAN_POINT('Ctrl Pts',(0.185645823208615,-16.8075419983836,
3.03148557757684));
#56413=CARTESIAN_POINT('Ctrl Pts',(0.0929598306468264,-16.8081542912968,
3.03090263974755));
#56414=CARTESIAN_POINT('Ctrl Pts',(0.000425097092084769,-16.8081561849884,
3.03090086182255));
#56415=CARTESIAN_POINT('Ctrl Pts',(0.000283398425769262,-16.8081561878882,
3.0309008591));
#56416=CARTESIAN_POINT('Ctrl Pts',(0.000141699394583094,-16.808156189357,
3.03090085774004));
#56417=CARTESIAN_POINT('Ctrl Pts',(-1.42137912181577E-12,-16.8081561893948,
3.03090085774268));
#56418=CARTESIAN_POINT('Ctrl Pts',(-0.229739891951006,-16.8081562505921,
3.03090086201527));
#56419=CARTESIAN_POINT('Ctrl Pts',(-0.46043877177314,-16.8043912206802,
3.03448552365188));
#56420=CARTESIAN_POINT('Ctrl Pts',(-0.691871120056919,-16.7967011224477,
3.04171955588636));
#56421=CARTESIAN_POINT('Ctrl Pts',(-0.925120551421554,-16.7889506456748,
3.04901038587482));
#56422=CARTESIAN_POINT('Ctrl Pts',(-1.15911501406741,-16.7772132199962,
3.0600081021688));
#56423=CARTESIAN_POINT('Ctrl Pts',(-1.39362363479407,-16.76136551204,3.07474453732183));
#56424=CARTESIAN_POINT('Ctrl Pts',(-1.629597578966,-16.7454187799286,3.08957305285921));
#56425=CARTESIAN_POINT('Ctrl Pts',(-1.86609212671074,-16.7253102698,3.10818710540346));
#56426=CARTESIAN_POINT('Ctrl Pts',(-2.10287204990648,-16.7009548892184,
3.13058492596091));
#56427=CARTESIAN_POINT('Ctrl Pts',(-2.34248173396402,-16.6763084370722,
3.15325042325018));
#56428=CARTESIAN_POINT('Ctrl Pts',(-2.58238365528549,-16.6473130159242,
3.17979062465384));
#56429=CARTESIAN_POINT('Ctrl Pts',(-2.82233405091119,-16.613921555402,3.21016945217466));
#56430=CARTESIAN_POINT('Ctrl Pts',(-2.92685480744949,-16.5993764628357,
3.22340226234338));
#56431=CARTESIAN_POINT('Ctrl Pts',(-3.03138476157114,-16.5839977804036,
3.23736298770903));
#56432=CARTESIAN_POINT('Ctrl Pts',(-3.1359037662506,-16.567783992341,3.25204669131969));
#56433=CARTESIAN_POINT('Ctrl Pts',(-3.3986955157854,-16.5270177245736,3.28896587337018));
#56434=CARTESIAN_POINT('Ctrl Pts',(-3.66141401515956,-16.4809448942829,
3.33045628489074));
#56435=CARTESIAN_POINT('Ctrl Pts',(-3.92371507449025,-16.4293937238543,
3.37639868267872));
#56436=CARTESIAN_POINT('Ctrl Pts',(-4.19322219386227,-16.3764263150382,
3.4236032319721));
#56437=CARTESIAN_POINT('Ctrl Pts',(-4.46228862190867,-16.3176757932309,
3.47550729074249));
#56438=CARTESIAN_POINT('Ctrl Pts',(-4.73054101504463,-16.2530046079271,
3.53194531634852));
#56439=CARTESIAN_POINT('Ctrl Pts',(-5.02397088259713,-16.1822635527727,
3.59368046877308));
#56440=CARTESIAN_POINT('Ctrl Pts',(-5.31642673781812,-16.1044383297438,
3.66084025775089));
#56441=CARTESIAN_POINT('Ctrl Pts',(-5.60741993866506,-16.0194038470247,
3.73317123771322));
#56442=CARTESIAN_POINT('Ctrl Pts',(-5.82713749210776,-15.9551976441069,
3.78778552392052));
#56443=CARTESIAN_POINT('Ctrl Pts',(-6.0460211617445,-15.8868825856208,3.84534709603784));
#56444=CARTESIAN_POINT('Ctrl Pts',(-6.26386060045575,-15.8144217505232,
3.90573752921543));
#56445=CARTESIAN_POINT('Ctrl Pts',(6.38290978637461,-15.7742583800757,3.93905205217285));
#56446=CARTESIAN_POINT('Ctrl Pts',(6.3333020539761,-15.7921071431687,3.92502738225168));
#56447=CARTESIAN_POINT('Ctrl Pts',(5.70273749003655,-16.0157853682326,3.74884667445043));
#56448=CARTESIAN_POINT('Ctrl Pts',(4.37427082963316,-16.4041108648871,3.43234872788488));
#56449=CARTESIAN_POINT('Ctrl Pts',(2.28459432793093,-16.7764308999776,3.1131849942996));
#56450=CARTESIAN_POINT('Ctrl Pts',(0.00159936025366462,-16.9132852594445,
2.99188131777531));
#56451=CARTESIAN_POINT('Ctrl Pts',(-2.28164217664832,-16.7767952240661,
3.11286535847525));
#56452=CARTESIAN_POINT('Ctrl Pts',(-4.37189098414695,-16.4046868752343,
3.43186693184216));
#56453=CARTESIAN_POINT('Ctrl Pts',(-5.70139586193533,-16.0162274050497,
3.74849394120053));
#56454=CARTESIAN_POINT('Ctrl Pts',(-6.33273158044223,-15.7923124119726,
3.92486608374166));
#56455=CARTESIAN_POINT('Ctrl Pts',(-6.38291250185657,-15.7742574063264,
3.93905280639695));
#56456=CARTESIAN_POINT('Ctrl Pts',(6.17912845842874,-15.1595937752886,3.89098583450951));
#56457=CARTESIAN_POINT('Ctrl Pts',(6.13107889153985,-15.1768762735422,3.87759665383682));
#56458=CARTESIAN_POINT('Ctrl Pts',(5.52032715675414,-15.393459716353,3.70939428322624));
#56459=CARTESIAN_POINT('Ctrl Pts',(4.23379427768671,-15.7694977771825,3.40711733970962));
#56460=CARTESIAN_POINT('Ctrl Pts',(2.21086559757556,-16.1300032036696,3.10222422277282));
#56461=CARTESIAN_POINT('Ctrl Pts',(0.00154762091081913,-16.2624919144746,
2.98634703116607));
#56462=CARTESIAN_POINT('Ctrl Pts',(-2.20800828847039,-16.1303559293748,
3.10191887675622));
#56463=CARTESIAN_POINT('Ctrl Pts',(-4.23148992251726,-15.7700555537294,
3.40665711311912));
#56464=CARTESIAN_POINT('Ctrl Pts',(-5.51902775455387,-15.3938877517215,
3.7090574686422));
#56465=CARTESIAN_POINT('Ctrl Pts',(-6.13052633629179,-15.1770750297593,
3.87744266458973));
#56466=CARTESIAN_POINT('Ctrl Pts',(-6.17913108867696,-15.1595928319861,
3.89098655522151));
#56467=CARTESIAN_POINT('Ctrl Pts',(6.17606315768169,-14.7496965076852,3.38896273183938));
#56468=CARTESIAN_POINT('Ctrl Pts',(6.12814754427055,-14.7667722774024,3.37574158733111));
#56469=CARTESIAN_POINT('Ctrl Pts',(5.51906854398708,-14.9807801088444,3.20963583670899));
#56470=CARTESIAN_POINT('Ctrl Pts',(4.23523288067283,-15.3527406605511,2.91075424990737));
#56471=CARTESIAN_POINT('Ctrl Pts',(2.21316745047304,-15.7100780789674,2.60855283602971));
#56472=CARTESIAN_POINT('Ctrl Pts',(0.00154976796005158,-15.8416245753242,
2.49347245636735));
#56473=CARTESIAN_POINT('Ctrl Pts',(-2.21030901582472,-15.7104281020419,
2.60824978737707));
#56474=CARTESIAN_POINT('Ctrl Pts',(-4.23293177008851,-15.3532929275836,
2.91029867561449));
#56475=CARTESIAN_POINT('Ctrl Pts',(-5.51777239596502,-14.9812032134454,
3.20930307427043));
#56476=CARTESIAN_POINT('Ctrl Pts',(-6.12759653002278,-14.766968655442,3.37558952923473));
#56477=CARTESIAN_POINT('Ctrl Pts',(-6.17606578034696,-14.749695575192,3.38896344151997));
#56478=CARTESIAN_POINT('Ctrl Pts',(6.37402533240034,-14.8205647331695,2.77721315208895));
#56479=CARTESIAN_POINT('Ctrl Pts',(6.32474120702746,-14.8379302534618,2.7635828203485));
#56480=CARTESIAN_POINT('Ctrl Pts',(5.69822078925919,-15.0555874524055,2.59232277986186));
#56481=CARTESIAN_POINT('Ctrl Pts',(4.3763630139826,-15.4343716381957,2.28380501669291));
#56482=CARTESIAN_POINT('Ctrl Pts',(2.28927089645763,-15.7992586270626,1.97099402057018));
#56483=CARTESIAN_POINT('Ctrl Pts',(0.00160387216188493,-15.9338947894004,
1.85158149042877));
#56484=CARTESIAN_POINT('Ctrl Pts',(-2.28631697573182,-15.7996165966553,
1.97067982535358));
#56485=CARTESIAN_POINT('Ctrl Pts',(-4.37399133895244,-15.4349347419952,
2.28333417339121));
#56486=CARTESIAN_POINT('Ctrl Pts',(-5.69688706113254,-15.0560179588341,
2.59197956119757));
#56487=CARTESIAN_POINT('Ctrl Pts',(-6.32417445620707,-14.8381299631328,
2.76342605380414));
#56488=CARTESIAN_POINT('Ctrl Pts',(-6.37402802959059,-14.8205637846944,
2.77721388049884));
#56489=CARTESIAN_POINT('',(-6.24994617571413,-14.8593872446902,2.7654678483052));
#56490=CARTESIAN_POINT('Ctrl Pts',(-6.26386065059659,-15.8144217484621,
3.90573734578416));
#56491=CARTESIAN_POINT('Ctrl Pts',(-6.25434443086836,-15.785019022528,3.90345726758071));
#56492=CARTESIAN_POINT('Ctrl Pts',(-6.24500662918812,-15.7549893140376,
3.89973771704937));
#56493=CARTESIAN_POINT('Ctrl Pts',(-6.23594957548642,-15.7245054308269,
3.89442892418346));
#56494=CARTESIAN_POINT('Ctrl Pts',(-6.22712015926251,-15.694787721089,3.88925356104624));
#56495=CARTESIAN_POINT('Ctrl Pts',(-6.21855785026409,-15.6646386876711,
3.88256716093373));
#56496=CARTESIAN_POINT('Ctrl Pts',(-6.21036353205397,-15.6342585338879,
3.87425897704415));
#56497=CARTESIAN_POINT('Ctrl Pts',(-6.20229552087963,-15.6043466591088,
3.86607885531336));
#56498=CARTESIAN_POINT('Ctrl Pts',(-6.19458457012074,-15.5742111835533,
3.85632594327575));
#56499=CARTESIAN_POINT('Ctrl Pts',(-6.18732837413158,-15.5440770840101,
3.84493165751364));
#56500=CARTESIAN_POINT('Ctrl Pts',(-6.180199674674,-15.5144724620581,3.83373757746767));
#56501=CARTESIAN_POINT('Ctrl Pts',(-6.17351022859021,-15.484869802774,3.82095886554755));
#56502=CARTESIAN_POINT('Ctrl Pts',(-6.16734911575842,-15.4555073561589,
3.80657432514532));
#56503=CARTESIAN_POINT('Ctrl Pts',(-6.16654991777089,-15.4516985623769,
3.80470841292217));
#56504=CARTESIAN_POINT('Ctrl Pts',(-6.16575960055991,-15.4478938372451,
3.80281554671202));
#56505=CARTESIAN_POINT('Ctrl Pts',(-6.16497834939201,-15.4440937228137,
3.80089574069978));
#56506=CARTESIAN_POINT('Ctrl Pts',(-6.15904704790929,-15.4152430467601,
3.78632046873251));
#56507=CARTESIAN_POINT('Ctrl Pts',(-6.15363922157741,-15.3866574221223,
3.7701883034186));
#56508=CARTESIAN_POINT('Ctrl Pts',(-6.14882946602223,-15.3585798462333,
3.75253320668798));
#56509=CARTESIAN_POINT('Ctrl Pts',(-6.14408132815942,-15.3308619716668,
3.73510428908576));
#56510=CARTESIAN_POINT('Ctrl Pts',(-6.13991630821544,-15.3036400179101,
3.71619123188256));
#56511=CARTESIAN_POINT('Ctrl Pts',(-6.13639290835345,-15.277148689417,3.69587568153761));
#56512=CARTESIAN_POINT('Ctrl Pts',(-6.13289019776972,-15.2508129170595,
3.67567942337934));
#56513=CARTESIAN_POINT('Ctrl Pts',(-6.13002181404631,-15.225200020221,3.65409730611276));
#56514=CARTESIAN_POINT('Ctrl Pts',(-6.1278283387891,-15.2005294760176,3.63125660399451));
#56515=CARTESIAN_POINT('Ctrl Pts',(-6.1256423054971,-15.1759426333883,3.60849339521025));
#56516=CARTESIAN_POINT('Ctrl Pts',(-6.12412674761708,-15.1522925053128,
3.58448055607693));
#56517=CARTESIAN_POINT('Ctrl Pts',(-6.12330229910817,-15.1297736111913,
3.55938616778094));
#56518=CARTESIAN_POINT('Ctrl Pts',(-6.12247859245493,-15.1072749800319,
3.53431435992954));
#56519=CARTESIAN_POINT('Ctrl Pts',(-6.12234479666278,-15.085906170951,3.50816356397118));
#56520=CARTESIAN_POINT('Ctrl Pts',(-6.12290056030017,-15.0658281226386,
3.48113566064486));
#56521=CARTESIAN_POINT('Ctrl Pts',(-6.12345903224633,-15.0456522313754,
3.45397604681679));
#56522=CARTESIAN_POINT('Ctrl Pts',(-6.12471375736229,-15.0267801876162,
3.4259315055787));
#56523=CARTESIAN_POINT('Ctrl Pts',(-6.12664318986121,-15.009333516031,3.39723119924967));
#56524=CARTESIAN_POINT('Ctrl Pts',(-6.12858008763558,-14.9918193405507,
3.36841984695647));
#56525=CARTESIAN_POINT('Ctrl Pts',(-6.13119677248217,-14.9757418273395,
3.33894848911829));
#56526=CARTESIAN_POINT('Ctrl Pts',(-6.13445162804978,-14.9611764966025,
3.30906130288997));
#56527=CARTESIAN_POINT('Ctrl Pts',(-6.13774388041001,-14.9464438169181,
3.27883072664567));
#56528=CARTESIAN_POINT('Ctrl Pts',(-6.1416888291907,-14.9332583176426,3.24817557819826));
#56529=CARTESIAN_POINT('Ctrl Pts',(-6.146225986249,-14.9216474232892,3.21734812083878));
#56530=CARTESIAN_POINT('Ctrl Pts',(-6.14952974350501,-14.9131928831496,
3.1949009287696));
#56531=CARTESIAN_POINT('Ctrl Pts',(-6.15314710801936,-14.9055721093889,
3.17236239654086));
#56532=CARTESIAN_POINT('Ctrl Pts',(-6.15705019295712,-14.8987793902855,
3.1498259448202));
#56533=CARTESIAN_POINT('Ctrl Pts',(-6.16250603101395,-14.8892843431664,
3.11832388095944));
#56534=CARTESIAN_POINT('Ctrl Pts',(-6.16852029995459,-14.8814088706154,
3.08682723960827));
#56535=CARTESIAN_POINT('Ctrl Pts',(-6.17500715596895,-14.8750972650963,
3.05557116825302));
#56536=CARTESIAN_POINT('Ctrl Pts',(-6.18164240267732,-14.8686412778426,
3.0236000956537));
#56537=CARTESIAN_POINT('Ctrl Pts',(-6.18877175292211,-14.8638210169963,
2.9918813640031));
#56538=CARTESIAN_POINT('Ctrl Pts',(-6.19629782114769,-14.8605341134556,
2.96063315662886));
#56539=CARTESIAN_POINT('Ctrl Pts',(-6.20393536255677,-14.8571985255834,
2.92892211300998));
#56540=CARTESIAN_POINT('Ctrl Pts',(-6.21198110770334,-14.8554413379348,
2.89769601725007));
#56541=CARTESIAN_POINT('Ctrl Pts',(-6.22033312083788,-14.8551215609014,
2.86714098770769));
#56542=CARTESIAN_POINT('Ctrl Pts',(-6.22888542845216,-14.8547941151091,
2.8358532002485));
#56543=CARTESIAN_POINT('Ctrl Pts',(-6.23775854302413,-14.855973076702,2.80526926701399));
#56544=CARTESIAN_POINT('Ctrl Pts',(-6.2468481217032,-14.8584831269518,2.77554067017534));
#56545=CARTESIAN_POINT('Ctrl Pts',(-6.24787807581803,-14.8587675445991,
2.77217207722695));
#56546=CARTESIAN_POINT('Ctrl Pts',(-6.24891081743635,-14.8590690353655,
2.76881441496404));
#56547=CARTESIAN_POINT('Ctrl Pts',(-6.2499462014697,-14.8593873322588,2.76546786460251));
#56548=CARTESIAN_POINT('Ctrl Pts',(6.24994600838289,-14.8593877792286,2.76546575478416));
#56549=CARTESIAN_POINT('Ctrl Pts',(6.23977984081587,-14.8628913778696,2.76270639179577));
#56550=CARTESIAN_POINT('Ctrl Pts',(6.22960745928517,-14.8663868331761,2.75995200693042));
#56551=CARTESIAN_POINT('Ctrl Pts',(6.21942887054227,-14.8698741336584,2.75720262586154));
#56552=CARTESIAN_POINT('Ctrl Pts',(5.94045907762464,-14.9654523634053,2.68184893127683));
#56553=CARTESIAN_POINT('Ctrl Pts',(5.65682493353885,-15.0549072042649,2.61025085701354));
#56554=CARTESIAN_POINT('Ctrl Pts',(5.36871986923688,-15.1379883804168,2.54298737950022));
#56555=CARTESIAN_POINT('Ctrl Pts',(5.20701903870747,-15.1846182278223,2.50523531774958));
#56556=CARTESIAN_POINT('Ctrl Pts',(5.043910181019,-15.2292398216681,2.46884935482955));
#56557=CARTESIAN_POINT('Ctrl Pts',(4.87943057404617,-15.271805068122,2.43393717671929));
#56558=CARTESIAN_POINT('Ctrl Pts',(4.73516526186832,-15.3091391101994,2.40331565246725));
#56559=CARTESIAN_POINT('Ctrl Pts',(4.58984788654057,-15.3448914601748,2.37382281843847));
#56560=CARTESIAN_POINT('Ctrl Pts',(4.44350430295742,-15.3790302121371,2.34551947111766));
#56561=CARTESIAN_POINT('Ctrl Pts',(4.35236115826965,-15.4002919110334,2.32789207662009));
#56562=CARTESIAN_POINT('Ctrl Pts',(4.26081996602347,-15.4209276863025,2.31072611327243));
#56563=CARTESIAN_POINT('Ctrl Pts',(4.1688902167991,-15.4409299318026,2.29403520550717));
#56564=CARTESIAN_POINT('Ctrl Pts',(4.04912204636317,-15.4669893126708,2.27228991083569));
#56565=CARTESIAN_POINT('Ctrl Pts',(3.92869265731007,-15.4919737044677,2.25135119194118));
#56566=CARTESIAN_POINT('Ctrl Pts',(3.80762011138965,-15.5158663514278,2.23124760392297));
#56567=CARTESIAN_POINT('Ctrl Pts',(3.74708383842945,-15.5278126749079,2.22119580991386));
#56568=CARTESIAN_POINT('Ctrl Pts',(3.68638677338942,-15.5394860495579,2.21135279662547));
#56569=CARTESIAN_POINT('Ctrl Pts',(3.62553130145798,-15.5508843162348,2.20172186897067));
#56570=CARTESIAN_POINT('Ctrl Pts',(3.59510356549227,-15.5565834495732,2.19690640514328));
#56571=CARTESIAN_POINT('Ctrl Pts',(3.56463622765007,-15.5622138051242,2.19214396260718));
#56572=CARTESIAN_POINT('Ctrl Pts',(3.53412958926692,-15.5677751085979,2.18743494614879));
#56573=CARTESIAN_POINT('Ctrl Pts',(3.51887627007534,-15.5705557603347,2.18508043791959));
#56574=CARTESIAN_POINT('Ctrl Pts',(3.50361312574009,-15.5733191490016,2.18273928620272));
#56575=CARTESIAN_POINT('Ctrl Pts',(3.48834019436521,-15.5760652400543,2.18041154067411));
#56576=CARTESIAN_POINT('Ctrl Pts',(3.48070372867777,-15.5774382855807,2.1792476679098));
#56577=CARTESIAN_POINT('Ctrl Pts',(3.47306481622993,-15.5788070067004,2.17808714669213));
#56578=CARTESIAN_POINT('Ctrl Pts',(3.46542346181371,-15.5801713990796,2.17692998316942));
#56579=CARTESIAN_POINT('Ctrl Pts',(3.4577821073975,-15.5815357914587,2.17577281964672));
#56580=CARTESIAN_POINT('Ctrl Pts',(3.45127968407358,-15.5826934816899,2.17479074328016));
#56581=CARTESIAN_POINT('Ctrl Pts',(3.44249207745967,-15.5842515856498,2.17346857181511));
#56582=CARTESIAN_POINT('Ctrl Pts',(3.14525419878888,-15.6369539352363,2.12874656060334));
#56583=CARTESIAN_POINT('Ctrl Pts',(2.84604223011535,-15.6827939421746,2.0894683825547));
#56584=CARTESIAN_POINT('Ctrl Pts',(2.54514472779552,-15.721727079666,2.05594698807718));
#56585=CARTESIAN_POINT('Ctrl Pts',(2.4748534034894,-15.7308220763761,2.04811620453046));
#56586=CARTESIAN_POINT('Ctrl Pts',(2.40447003318719,-15.7395399859309,2.04059970994486));
#56587=CARTESIAN_POINT('Ctrl Pts',(2.33399818954889,-15.747879930087,2.03340174451536));
#56588=CARTESIAN_POINT('Ctrl Pts',(2.03519724903146,-15.7832413315922,2.00288233805301));
#56589=CARTESIAN_POINT('Ctrl Pts',(1.73480624879659,-15.8118108685873,1.97808668568234));
#56590=CARTESIAN_POINT('Ctrl Pts',(1.43320004594516,-15.8335486239916,1.9591558973543));
#56591=CARTESIAN_POINT('Ctrl Pts',(1.13568028278521,-15.8549918561875,1.94048160084931));
#56592=CARTESIAN_POINT('Ctrl Pts',(0.836977493414725,-15.8697871517185,
1.92751422946157));
#56593=CARTESIAN_POINT('Ctrl Pts',(0.537450111638287,-15.8778586274268,
1.9204227314522));
#56594=CARTESIAN_POINT('Ctrl Pts',(0.359128834569043,-15.8826639171722,
1.91620086374227));
#56595=CARTESIAN_POINT('Ctrl Pts',(0.180515305473063,-15.8850853530742,
1.91406224079188));
#56596=CARTESIAN_POINT('Ctrl Pts',(0.00168608937214161,-15.8851005062438,
1.91404848768711));
#56597=CARTESIAN_POINT('Ctrl Pts',(0.00126561777193262,-15.8851005418727,
1.91404845535017));
#56598=CARTESIAN_POINT('Ctrl Pts',(0.000845144979868073,-15.8851005641965,
1.9140484347624));
#56599=CARTESIAN_POINT('Ctrl Pts',(0.0004246709969564,-15.8851005732151,
1.91404842592356));
#56600=CARTESIAN_POINT('Ctrl Pts',(-0.295959203807716,-15.8851069302863,
1.91404219559918));
#56601=CARTESIAN_POINT('Ctrl Pts',(-0.591744559536345,-15.8785138703217,
1.91980287342502));
#56602=CARTESIAN_POINT('Ctrl Pts',(-0.88659911326893,-15.865406775067,1.93122579775579));
#56603=CARTESIAN_POINT('Ctrl Pts',(-1.17043855201861,-15.8527893319457,
1.94222198685946));
#56604=CARTESIAN_POINT('Ctrl Pts',(-1.45341579891742,-15.8341351371654,
1.9584656897086));
#56605=CARTESIAN_POINT('Ctrl Pts',(-1.73522496589225,-15.8094873093356,
1.97989352216698));
#56606=CARTESIAN_POINT('Ctrl Pts',(-1.93441571348076,-15.7920655224414,
1.9950393245992));
#56607=CARTESIAN_POINT('Ctrl Pts',(-2.13302831950087,-15.7716507168188,
2.01275505402788));
#56608=CARTESIAN_POINT('Ctrl Pts',(-2.33095462708823,-15.7482542956345,
2.03297954855697));
#56609=CARTESIAN_POINT('Ctrl Pts',(-2.41848204551205,-15.737907877457,2.04192327017052));
#56610=CARTESIAN_POINT('Ctrl Pts',(-2.5058752686069,-15.7269782738699,2.05135769349964));
#56611=CARTESIAN_POINT('Ctrl Pts',(-2.59312769529722,-15.7154672816487,
2.06127283737851));
#56612=CARTESIAN_POINT('Ctrl Pts',(-2.73540614215869,-15.6966968456026,
2.07744099825386));
#56613=CARTESIAN_POINT('Ctrl Pts',(-2.8773069640955,-15.6763802934088,2.09489214436736));
#56614=CARTESIAN_POINT('Ctrl Pts',(-3.01879388031371,-15.654524164203,2.11359109983342));
#56615=CARTESIAN_POINT('Ctrl Pts',(-3.08953733842282,-15.6435960996002,
2.12294057756645));
#56616=CARTESIAN_POINT('Ctrl Pts',(-3.16017731874909,-15.6322831201713,
2.13260200512541));
#56617=CARTESIAN_POINT('Ctrl Pts',(-3.23070939172754,-15.6205859822879,
2.14257039117694));
#56618=CARTESIAN_POINT('Ctrl Pts',(-3.26597542821676,-15.6147374133462,
2.14755458420271));
#56619=CARTESIAN_POINT('Ctrl Pts',(-3.30121448775136,-15.6087928035061,
2.15261551669182));
#56620=CARTESIAN_POINT('Ctrl Pts',(-3.33642601923097,-15.6027522412624,
2.15775254825432));
#56621=CARTESIAN_POINT('Ctrl Pts',(-3.35403178497077,-15.5997319601406,
2.16032106403558));
#56622=CARTESIAN_POINT('Ctrl Pts',(-3.37163066868688,-15.5966876908382,
2.16290860457476));
#56623=CARTESIAN_POINT('Ctrl Pts',(-3.38922260183242,-15.5936194441472,
2.16551508782531));
#56624=CARTESIAN_POINT('Ctrl Pts',(-3.39801856840519,-15.5920853208017,
2.16681832945058));
#56625=CARTESIAN_POINT('Ctrl Pts',(-3.40681279733464,-15.5905452031042,
2.16812630675302));
#56626=CARTESIAN_POINT('Ctrl Pts',(-3.41560528007505,-15.5889990923873,
2.16943900934683));
#56627=CARTESIAN_POINT('Ctrl Pts',(-3.42439776281546,-15.5874529816703,
2.17075171194064));
#56628=CARTESIAN_POINT('Ctrl Pts',(-3.43433010001144,-15.5856984969522,
2.17224087292842));
#56629=CARTESIAN_POINT('Ctrl Pts',(-3.44197748118868,-15.5843427824956,
2.17339128257614));
#56630=CARTESIAN_POINT('Ctrl Pts',(-3.7396863674353,-15.5315654680661,2.21817617913244));
#56631=CARTESIAN_POINT('Ctrl Pts',(-4.03372618068042,-15.4722068983851,
2.26813399437449));
#56632=CARTESIAN_POINT('Ctrl Pts',(-4.32379161088466,-15.4065298160674,
2.32277245567381));
#56633=CARTESIAN_POINT('Ctrl Pts',(-4.36297511470441,-15.3976578239653,
2.33015329507794));
#56634=CARTESIAN_POINT('Ctrl Pts',(-4.40208612349489,-15.3886704891556,
2.33761960458001));
#56635=CARTESIAN_POINT('Ctrl Pts',(-4.44112391129496,-15.3795684196056,
2.34517022409203));
#56636=CARTESIAN_POINT('Ctrl Pts',(-4.74647716824373,-15.3083721060159,
2.40423110817141));
#56637=CARTESIAN_POINT('Ctrl Pts',(-5.04734945831461,-15.2301587791586,
2.46844652844401));
#56638=CARTESIAN_POINT('Ctrl Pts',(-5.34351993333399,-15.1452169653489,
2.53722993612569));
#56639=CARTESIAN_POINT('Ctrl Pts',(-5.63969040835337,-15.0602751515392,
2.60601334380737));
#56640=CARTESIAN_POINT('Ctrl Pts',(-5.93115934890157,-14.9686047302175,
2.67936508447682));
#56641=CARTESIAN_POINT('Ctrl Pts',(-6.21771626963549,-14.8704603665138,
2.75674241330942));
#56642=CARTESIAN_POINT('Ctrl Pts',(-6.22846649522594,-14.8667784660818,
2.75964523533308));
#56643=CARTESIAN_POINT('Ctrl Pts',(-6.23920980862789,-14.8630874504706,
2.76255372768559));
#56644=CARTESIAN_POINT('Ctrl Pts',(-6.2499462014697,-14.8593873322588,2.76546786460251));
#56645=CARTESIAN_POINT('Ctrl Pts',(-6.25110470371109,-15.8289287536332,
3.90218662864265));
#56646=CARTESIAN_POINT('Ctrl Pts',(-6.29476787337534,-15.8135896688474,
3.91359102765067));
#56647=CARTESIAN_POINT('Ctrl Pts',(-6.42720364559721,-15.7642107597959,
3.95728968749399));
#56648=CARTESIAN_POINT('Ctrl Pts',(-6.63601152178557,-15.6709885974876,
4.07488311644954));
#56649=CARTESIAN_POINT('Ctrl Pts',(-6.84944948528204,-15.5474618085486,
4.28281049117623));
#56650=CARTESIAN_POINT('Ctrl Pts',(-7.00820034346764,-15.4198890442991,
4.54620357973042));
#56651=CARTESIAN_POINT('Ctrl Pts',(-7.09186675915703,-15.3065623348527,
4.82366122629296));
#56652=CARTESIAN_POINT('Ctrl Pts',(-7.10635949500348,-15.2412500255453,
5.00871313350102));
#56653=CARTESIAN_POINT('Ctrl Pts',(-7.10529849916785,-15.2149614744649,
5.08843009648874));
#56654=CARTESIAN_POINT('Ctrl Pts',(-6.05286305785348,-15.2163005098727,
3.8610994146941));
#56655=CARTESIAN_POINT('Ctrl Pts',(-6.09151808910752,-15.2026886082459,
3.87091449473368));
#56656=CARTESIAN_POINT('Ctrl Pts',(-6.20897986088989,-15.1587870717599,
3.90862214879026));
#56657=CARTESIAN_POINT('Ctrl Pts',(-6.39516878893685,-15.0754962562282,
4.01082172167384));
#56658=CARTESIAN_POINT('Ctrl Pts',(-6.58655600753875,-14.9647336461454,
4.19297762573022));
#56659=CARTESIAN_POINT('Ctrl Pts',(-6.72947207118409,-14.8503179692945,
4.42503188515894));
#56660=CARTESIAN_POINT('Ctrl Pts',(-6.80490807319583,-14.7490641911142,
4.67022341605911));
#56661=CARTESIAN_POINT('Ctrl Pts',(-6.81792929536288,-14.6911932840215,
4.83365326926337));
#56662=CARTESIAN_POINT('Ctrl Pts',(-6.81697819600131,-14.6680366840076,
4.90391474801704));
#56663=CARTESIAN_POINT('Ctrl Pts',(-6.04143776493508,-14.8034131353335,
3.36534479494879));
#56664=CARTESIAN_POINT('Ctrl Pts',(-6.09466994263046,-14.7850570925795,
3.37877528165601));
#56665=CARTESIAN_POINT('Ctrl Pts',(-6.25547105388986,-14.7263459526608,
3.43011952370043));
#56666=CARTESIAN_POINT('Ctrl Pts',(-6.5059867483565,-14.6174407821712,3.56694282528));
#56667=CARTESIAN_POINT('Ctrl Pts',(-6.75879992208355,-14.4756583694627,
3.80561255232722));
#56668=CARTESIAN_POINT('Ctrl Pts',(-6.94511346013031,-14.3309179928438,
4.10493100761516));
#56669=CARTESIAN_POINT('Ctrl Pts',(-7.04295606862131,-14.2029509252661,
4.4186870668889));
#56670=CARTESIAN_POINT('Ctrl Pts',(-7.0600439880215,-14.1289188698671,4.6285048841726));
#56671=CARTESIAN_POINT('Ctrl Pts',(-7.05878639808624,-14.0989674529702,
4.71932477573061));
#56672=CARTESIAN_POINT('Ctrl Pts',(-6.22464327430951,-14.869698639165,2.75012280382206));
#56673=CARTESIAN_POINT('Ctrl Pts',(-6.3021844915154,-14.8433338792577,2.76992975345015));
#56674=CARTESIAN_POINT('Ctrl Pts',(-6.53534318406533,-14.7595365042026,
2.84532114539174));
#56675=CARTESIAN_POINT('Ctrl Pts',(-6.89365005061659,-14.6067847346553,
3.04338350732949));
#56676=CARTESIAN_POINT('Ctrl Pts',(-7.24984556193816,-14.4111653547389,
3.38265482800274));
#56677=CARTESIAN_POINT('Ctrl Pts',(-7.50945482979155,-14.2131151686788,
3.80237713753254));
#56678=CARTESIAN_POINT('Ctrl Pts',(-7.64519560700152,-14.0377040723409,
4.23918626315073));
#56679=CARTESIAN_POINT('Ctrl Pts',(-7.66913959269001,-13.9348315572258,
4.53204878917508));
#56680=CARTESIAN_POINT('Ctrl Pts',(-7.66736629471592,-13.8927511366881,
4.65954565759216));
#56681=CARTESIAN_POINT('',(-7.00000834771932,-14.7967990237358,4.92966193756367));
#56682=CARTESIAN_POINT('',(-7.00000024832194,-14.5427415422438,3.16613142102349));
#56683=CARTESIAN_POINT('Ctrl Pts',(-7.,-14.7967990237703,4.92966193770567));
#56684=CARTESIAN_POINT('Ctrl Pts',(-7.,-14.7557808111679,4.82629817381466));
#56685=CARTESIAN_POINT('Ctrl Pts',(-7.,-14.7211382308601,4.73284571088999));
#56686=CARTESIAN_POINT('Ctrl Pts',(-7.,-14.6931996139855,4.65100396188635));
#56687=CARTESIAN_POINT('Ctrl Pts',(-7.,-14.6792303055482,4.61008308738453));
#56688=CARTESIAN_POINT('Ctrl Pts',(-7.,-14.6668893039443,4.57207807978592));
#56689=CARTESIAN_POINT('Ctrl Pts',(-7.,-14.6560069105721,4.53722371941572));
#56690=CARTESIAN_POINT('Ctrl Pts',(-7.,-14.650565713886,4.51979653923062));
#56691=CARTESIAN_POINT('Ctrl Pts',(-7.,-14.6454875640803,4.50315711223306));
#56692=CARTESIAN_POINT('Ctrl Pts',(-7.,-14.6407442198345,4.48733398590899));
#56693=CARTESIAN_POINT('Ctrl Pts',(-7.,-14.6383725477116,4.47942242274696));
#56694=CARTESIAN_POINT('Ctrl Pts',(-7.,-14.6360845769787,4.47171493475331));
#56695=CARTESIAN_POINT('Ctrl Pts',(-7.,-14.6338764851935,4.46421491609655));
#56696=CARTESIAN_POINT('Ctrl Pts',(-7.,-14.6327724393009,4.46046490676816));
#56697=CARTESIAN_POINT('Ctrl Pts',(-7.,-14.6316883631452,4.45676676477401));
#56698=CARTESIAN_POINT('Ctrl Pts',(-7.,-14.6306237806622,4.45312090459993));
#56699=CARTESIAN_POINT('Ctrl Pts',(-7.,-14.6295591981792,4.44947504442585));
#56700=CARTESIAN_POINT('Ctrl Pts',(-7.,-14.6289879217431,4.44751654562367));
#56701=CARTESIAN_POINT('Ctrl Pts',(-7.,-14.6274880358216,4.44234058010723));
#56702=CARTESIAN_POINT('Ctrl Pts',(-7.,-14.6034898610781,4.35952513184433));
#56703=CARTESIAN_POINT('Ctrl Pts',(-7.,-14.5830030031066,4.27925663787387));
#56704=CARTESIAN_POINT('Ctrl Pts',(-7.,-14.5661061896712,4.20216723805092));
#56705=CARTESIAN_POINT('Ctrl Pts',(-7.,-14.5492093762358,4.12507783822797));
#56706=CARTESIAN_POINT('Ctrl Pts',(-7.,-14.536122312737,4.05276435033893));
#56707=CARTESIAN_POINT('Ctrl Pts',(-7.,-14.5256426270648,3.98124825300832));
#56708=CARTESIAN_POINT('Ctrl Pts',(-7.,-14.5046832557203,3.8382160583471));
#56709=CARTESIAN_POINT('Ctrl Pts',(-7.,-14.4945097492703,3.69572700311663));
#56710=CARTESIAN_POINT('Ctrl Pts',(-7.,-14.4974000293464,3.55811099350387));
#56711=CARTESIAN_POINT('Ctrl Pts',(-7.,-14.5002903094225,3.4204949838911));
#56712=CARTESIAN_POINT('Ctrl Pts',(-7.,-14.5162124657349,3.28797540399407));
#56713=CARTESIAN_POINT('Ctrl Pts',(-7.,-14.5427409643167,3.16613181594226));
#56714=CARTESIAN_POINT('Ctrl Pts',(-6.249946124203,-14.8593870695528,2.7654678157106));
#56715=CARTESIAN_POINT('Ctrl Pts',(-6.343283744982,-14.8272204162322,2.79079893610273));
#56716=CARTESIAN_POINT('Ctrl Pts',(-6.523195179618,-14.7609017514799,2.85471778320166));
#56717=CARTESIAN_POINT('Ctrl Pts',(-6.77477936719767,-14.6549005700431,
2.9891531637239));
#56718=CARTESIAN_POINT('Ctrl Pts',(-6.92743954945432,-14.5808182851627,
3.10289863010712));
#56719=CARTESIAN_POINT('Ctrl Pts',(-7.00000073074686,-14.5427415372861,
3.166130864439));
#56720=CARTESIAN_POINT('Ctrl Pts',(-6.26385620203836,-15.8144219269702,
3.90575361027663));
#56721=CARTESIAN_POINT('Ctrl Pts',(-6.29878849880756,-15.7919498083394,
3.9155545662544));
#56722=CARTESIAN_POINT('Ctrl Pts',(-6.33342137746813,-15.7685324070384,
3.92737928356594));
#56723=CARTESIAN_POINT('Ctrl Pts',(-6.36751124742063,-15.7442057457572,
3.94126218049215));
#56724=CARTESIAN_POINT('Ctrl Pts',(-6.41221172875109,-15.7123073117078,
3.95946618583823));
#56725=CARTESIAN_POINT('Ctrl Pts',(-6.45597990026991,-15.6788445993522,
3.98120981151469));
#56726=CARTESIAN_POINT('Ctrl Pts',(-6.49830303351248,-15.6439338049921,
4.00642789449063));
#56727=CARTESIAN_POINT('Ctrl Pts',(-6.51773444154521,-15.6279055519308,
4.01800602735948));
#56728=CARTESIAN_POINT('Ctrl Pts',(-6.53686061955037,-15.6115723297184,
4.03031648655404));
#56729=CARTESIAN_POINT('Ctrl Pts',(-6.55562848922986,-15.5949468145626,
4.04335300963381));
#56730=CARTESIAN_POINT('Ctrl Pts',(-6.56693295578168,-15.5849327541927,
4.05120530942191));
#56731=CARTESIAN_POINT('Ctrl Pts',(-6.5781074009999,-15.5748126648585,4.05932104211864));
#56732=CARTESIAN_POINT('Ctrl Pts',(-6.58913980261017,-15.564589480158,4.06769890657097));
#56733=CARTESIAN_POINT('Ctrl Pts',(-6.6224247220355,-15.5337459801617,4.09297504798636));
#56734=CARTESIAN_POINT('Ctrl Pts',(-6.65441844741923,-15.5019631749137,
4.12063740177302));
#56735=CARTESIAN_POINT('Ctrl Pts',(-6.68483583877449,-15.4693356416747,
4.1505725029576));
#56736=CARTESIAN_POINT('Ctrl Pts',(-6.70508550921129,-15.4476146207122,
4.17050109993688));
#56737=CARTESIAN_POINT('Ctrl Pts',(-6.72463611746707,-15.425519458277,4.19143689346209));
#56738=CARTESIAN_POINT('Ctrl Pts',(-6.74339683172981,-15.4030811212164,
4.21334656021343));
#56739=CARTESIAN_POINT('Ctrl Pts',(-6.75277718886118,-15.3918619526861,
4.22430139358911));
#56740=CARTESIAN_POINT('Ctrl Pts',(-6.76196001583808,-15.380556992843,4.2354997441859));
#56741=CARTESIAN_POINT('Ctrl Pts',(-6.77093332222585,-15.3691703979231,
4.24693746861905));
#56742=CARTESIAN_POINT('Ctrl Pts',(-6.77168679657353,-15.3682142835536,
4.24789787625296));
#56743=CARTESIAN_POINT('Ctrl Pts',(-6.77243879339467,-15.3672575937706,
4.24885997164811));
#56744=CARTESIAN_POINT('Ctrl Pts',(-6.77318930549531,-15.3663003310321,
4.24982375242268));
#56745=CARTESIAN_POINT('Ctrl Pts',(-6.77690780753395,-15.3615574582103,
4.2545989196345));
#56746=CARTESIAN_POINT('Ctrl Pts',(-6.7805898630739,-15.3568005199061,4.2594154600463));
#56747=CARTESIAN_POINT('Ctrl Pts',(-6.78423480615889,-15.3520298334718,
4.26427287788366));
#56748=CARTESIAN_POINT('Ctrl Pts',(-6.78642511048231,-15.3491630520492,
4.26719177758709));
#56749=CARTESIAN_POINT('Ctrl Pts',(-6.78860201371202,-15.3462913058629,
4.27012543865483));
#56750=CARTESIAN_POINT('Ctrl Pts',(-6.79076536854309,-15.3434146664145,
4.27307375201837));
#56751=CARTESIAN_POINT('Ctrl Pts',(-6.79256527438427,-15.3410213095449,
4.27552674140709));
#56752=CARTESIAN_POINT('Ctrl Pts',(-6.79472129741818,-15.3381328046024,
4.27849606180966));
#56753=CARTESIAN_POINT('Ctrl Pts',(-6.79632073241739,-15.3359765995829,
4.28071849115757));
#56754=CARTESIAN_POINT('Ctrl Pts',(-6.79664370099805,-15.335541204287,4.28116725891148));
#56755=CARTESIAN_POINT('Ctrl Pts',(-6.79694411509937,-15.3351356778824,
4.28158545805962));
#56756=CARTESIAN_POINT('Ctrl Pts',(-6.79721464032234,-15.3347701387616,
4.28196254138343));
#56757=CARTESIAN_POINT('Ctrl Pts',(-6.813641421115,-15.3125739422593,4.30485972277292));
#56758=CARTESIAN_POINT('Ctrl Pts',(-6.8298628224892,-15.2892413668964,4.32945828123986));
#56759=CARTESIAN_POINT('Ctrl Pts',(-6.84559240418816,-15.264799690596,4.35586039075551));
#56760=CARTESIAN_POINT('Ctrl Pts',(-6.86049447053488,-15.2416438630078,
4.38087351540342));
#56761=CARTESIAN_POINT('Ctrl Pts',(-6.87495525595165,-15.217492469619,4.40750543899532));
#56762=CARTESIAN_POINT('Ctrl Pts',(-6.88869160911252,-15.1923864352567,
4.43582616937284));
#56763=CARTESIAN_POINT('Ctrl Pts',(-6.89525615325614,-15.1803883693281,
4.44936052471195));
#56764=CARTESIAN_POINT('Ctrl Pts',(-6.9016546372832,-15.168172554529,4.46328032005208));
#56765=CARTESIAN_POINT('Ctrl Pts',(-6.90785249150635,-15.1557451069306,
4.47759170963739));
#56766=CARTESIAN_POINT('Ctrl Pts',(-6.91793699586261,-15.1355244555679,
4.50087771563573));
#56767=CARTESIAN_POINT('Ctrl Pts',(-6.927490981232,-15.114742987979,4.52520121964848));
#56768=CARTESIAN_POINT('Ctrl Pts',(-6.93637014188753,-15.0934359688446,
4.55056606232792));
#56769=CARTESIAN_POINT('Ctrl Pts',(-6.94680888543516,-15.0683864718102,
4.58038612056639));
#56770=CARTESIAN_POINT('Ctrl Pts',(-6.95631603183839,-15.0426099666793,
4.61164611650852));
#56771=CARTESIAN_POINT('Ctrl Pts',(-6.96462796028164,-15.0161820172215,
4.64433003797493));
#56772=CARTESIAN_POINT('Ctrl Pts',(-6.97210085492414,-14.9924217931937,
4.67371473531559));
#56773=CARTESIAN_POINT('Ctrl Pts',(-6.97860757742105,-14.9681351353331,
4.70425016069309));
#56774=CARTESIAN_POINT('Ctrl Pts',(-6.98392953768413,-14.9433927148096,
4.73590672977319));
#56775=CARTESIAN_POINT('Ctrl Pts',(-6.9894513026938,-14.9177213784697,4.76875179565718));
#56776=CARTESIAN_POINT('Ctrl Pts',(-6.99369738134614,-14.8915589743126,
4.80280473163056));
#56777=CARTESIAN_POINT('Ctrl Pts',(-6.99643896516185,-14.8650099262391,
4.83797412724184));
#56778=CARTESIAN_POINT('Ctrl Pts',(-6.99876094637331,-14.8425242409736,
4.86776080578873));
#56779=CARTESIAN_POINT('Ctrl Pts',(-7.00000353949097,-14.8197614873671,
4.89834788628858));
#56780=CARTESIAN_POINT('Ctrl Pts',(-7.0000090556196,-14.7967990238705,4.92966193753773));
#56781=CARTESIAN_POINT('Ctrl Pts',(-6.23412951824369,-25.6421123574084,
8.85535208221471));
#56782=CARTESIAN_POINT('Ctrl Pts',(-6.23490481866159,-25.3447917649169,
8.44426386352628));
#56783=CARTESIAN_POINT('Ctrl Pts',(-6.23649261565224,-24.5993905992671,
7.54006472228264));
#56784=CARTESIAN_POINT('Ctrl Pts',(-6.23803947015578,-23.2351584307484,
6.3068279708346));
#56785=CARTESIAN_POINT('Ctrl Pts',(-6.23759227455821,-21.5545925361952,
5.23225202843968));
#56786=CARTESIAN_POINT('Ctrl Pts',(-6.23570310449509,-19.7179594361743,
4.44990383975616));
#56787=CARTESIAN_POINT('Ctrl Pts',(-6.23204929482609,-17.7794287558552,
3.98190995592453));
#56788=CARTESIAN_POINT('Ctrl Pts',(-6.22726074605045,-16.0460358301738,
3.85975953085696));
#56789=CARTESIAN_POINT('Ctrl Pts',(-6.22400119816621,-14.9771498623589,
3.9271878537008));
#56790=CARTESIAN_POINT('Ctrl Pts',(-6.2226656607601,-14.5714122496638,3.9737494255116));
#56791=CARTESIAN_POINT('Ctrl Pts',(-6.72598973094391,-25.5461080305609,
8.92473407566849));
#56792=CARTESIAN_POINT('Ctrl Pts',(-6.726682888266,-25.2514056837406,8.51794194318656));
#56793=CARTESIAN_POINT('Ctrl Pts',(-6.72805115220009,-24.5127390076592,
7.6231901818145));
#56794=CARTESIAN_POINT('Ctrl Pts',(-6.72941870118895,-23.1617868482333,
6.40302824892384));
#56795=CARTESIAN_POINT('Ctrl Pts',(-6.72902370101902,-21.4982080380591,
5.33903634346242));
#56796=CARTESIAN_POINT('Ctrl Pts',(-6.72736764457739,-19.6804284777096,
4.56367588073428));
#56797=CARTESIAN_POINT('Ctrl Pts',(-6.72416397934811,-17.7615746380771,
4.09849087757912));
#56798=CARTESIAN_POINT('Ctrl Pts',(-6.71993311440092,-16.0451960532337,
3.97507643032026));
#56799=CARTESIAN_POINT('Ctrl Pts',(-6.71707859590867,-14.9863242428538,
4.04021097259499));
#56800=CARTESIAN_POINT('Ctrl Pts',(-6.71588986670998,-14.5843406118397,
4.08565752022343));
#56801=CARTESIAN_POINT('Ctrl Pts',(-7.02718519799001,-25.2169072632673,
9.16264676213727));
#56802=CARTESIAN_POINT('Ctrl Pts',(-7.02756389243507,-24.9320799770197,
8.76993802976445));
#56803=CARTESIAN_POINT('Ctrl Pts',(-7.02824880449839,-24.2181494335702,
7.90599874558347));
#56804=CARTESIAN_POINT('Ctrl Pts',(-7.02897712669706,-22.9136314295433,
6.72847692729127));
#56805=CARTESIAN_POINT('Ctrl Pts',(-7.02876720163468,-21.3070953687618,
5.70076837624308));
#56806=CARTESIAN_POINT('Ctrl Pts',(-7.02790266440921,-19.5522398659708,
4.95159468384772));
#56807=CARTESIAN_POINT('Ctrl Pts',(-7.02622931287819,-17.699530350317,4.50113364131783));
#56808=CARTESIAN_POINT('Ctrl Pts',(-7.02397928601801,-16.0419249094978,
4.38032070770886));
#56809=CARTESIAN_POINT('Ctrl Pts',(-7.02249260484221,-15.0188815943411,
4.44215073383211));
#56810=CARTESIAN_POINT('Ctrl Pts',(-7.0218496413372,-14.6305434261105,4.48559561596503));
#56811=CARTESIAN_POINT('Ctrl Pts',(-6.99838063007145,-24.8079471174881,
9.45820150662415));
#56812=CARTESIAN_POINT('Ctrl Pts',(-6.99835913456694,-24.5356483643624,
9.0827998521431));
#56813=CARTESIAN_POINT('Ctrl Pts',(-6.99821532660071,-23.8529250977185,
8.25667796475706));
#56814=CARTESIAN_POINT('Ctrl Pts',(-6.99814245616926,-22.6063522384878,
7.13148910279274));
#56815=CARTESIAN_POINT('Ctrl Pts',(-6.99816421969244,-21.0703284717052,
6.1488519358181));
#56816=CARTESIAN_POINT('Ctrl Pts',(-6.99828069431127,-19.3931405999627,
5.43285699124196));
#56817=CARTESIAN_POINT('Ctrl Pts',(-6.99850457242363,-17.6222147137414,
5.00216844902164));
#56818=CARTESIAN_POINT('Ctrl Pts',(-6.99873523795064,-16.0377473415385,
4.88660477570714));
#56819=CARTESIAN_POINT('Ctrl Pts',(-6.99894168314433,-15.0596464417134,
4.94565629804127));
#56820=CARTESIAN_POINT('Ctrl Pts',(-6.99898903502728,-14.6884846235588,
4.98714444975514));
#56821=CARTESIAN_POINT('',(-7.00000308919771,-24.7867179209035,9.33251796322023));
#56822=CARTESIAN_POINT('Origin',(-5.99998370363654,-24.7867138051394,9.33252808558063));
#56823=CARTESIAN_POINT('Ctrl Pts',(-7.00001101651462,-24.7867134185486,
9.33251828870258));
#56824=CARTESIAN_POINT('Ctrl Pts',(-7.00001786889336,-24.6735525617516,
9.17932101458571));
#56825=CARTESIAN_POINT('Ctrl Pts',(-7.00001802523742,-24.5580142816453,
9.03121151943847));
#56826=CARTESIAN_POINT('Ctrl Pts',(-7.00001556840049,-24.4406110956016,
8.88816527848438));
#56827=CARTESIAN_POINT('Ctrl Pts',(-7.00001306418049,-24.3209436477261,
8.74236021850253));
#56828=CARTESIAN_POINT('Ctrl Pts',(-7.00000784357216,-24.1993386409877,
8.60181549568451));
#56829=CARTESIAN_POINT('Ctrl Pts',(-7.00000354839216,-24.0762963462373,
8.4664716215797));
#56830=CARTESIAN_POINT('Ctrl Pts',(-7.00000225631055,-24.039282603626,8.42575730192));
#56831=CARTESIAN_POINT('Ctrl Pts',(-7.00000104345735,-24.0021385108519,
8.38551340481799));
#56832=CARTESIAN_POINT('Ctrl Pts',(-6.99999999753998,-23.9648769610003,
8.34573775584444));
#56833=CARTESIAN_POINT('Ctrl Pts',(-6.99999887666308,-23.9249449244552,
8.30311143797125));
#56834=CARTESIAN_POINT('Ctrl Pts',(-6.99999794690458,-23.8848779940374,
8.26102288192524));
#56835=CARTESIAN_POINT('Ctrl Pts',(-6.99999718086705,-23.8446913250953,
8.21946685878418));
#56836=CARTESIAN_POINT('Ctrl Pts',(-6.99999462214246,-23.7104594977578,
8.08066110379241));
#56837=CARTESIAN_POINT('Ctrl Pts',(-6.99999387750223,-23.5748954425034,
7.94779834684371));
#56838=CARTESIAN_POINT('Ctrl Pts',(-6.99999403434674,-23.4385318409074,
7.82067014042885));
#56839=CARTESIAN_POINT('Ctrl Pts',(-6.99999406716637,-23.4099978376986,
7.79406863821478));
#56840=CARTESIAN_POINT('Ctrl Pts',(-6.99999414003187,-23.3814286575789,
7.76771815577077));
#56841=CARTESIAN_POINT('Ctrl Pts',(-6.99999424548609,-23.3528289165217,
7.74161667605472));
#56842=CARTESIAN_POINT('Ctrl Pts',(-6.9999943242214,-23.3314754878549,7.72212852460256));
#56843=CARTESIAN_POINT('Ctrl Pts',(-6.99999441863055,-23.3106151793539,
7.70323910621462));
#56844=CARTESIAN_POINT('Ctrl Pts',(-6.99999453138906,-23.2890698214933,
7.68388256127447));
#56845=CARTESIAN_POINT('Ctrl Pts',(-6.99999463682087,-23.268924416221,7.66578374643865));
#56846=CARTESIAN_POINT('Ctrl Pts',(-6.99999475847195,-23.2481799802744,
7.64727659129448));
#56847=CARTESIAN_POINT('Ctrl Pts',(-6.99999490350867,-23.2258462584489,
7.62752046795438));
#56848=CARTESIAN_POINT('Ctrl Pts',(-6.99999520366107,-23.1796267908374,
7.58663532082214));
#56849=CARTESIAN_POINT('Ctrl Pts',(-6.99999556265701,-23.1331495398512,
7.5462152702438));
#56850=CARTESIAN_POINT('Ctrl Pts',(-6.99999595370187,-23.086424366087,7.50626141913471));
#56851=CARTESIAN_POINT('Ctrl Pts',(-6.99999673579158,-22.9929740185586,
7.42635371691654));
#56852=CARTESIAN_POINT('Ctrl Pts',(-6.99999764537285,-22.8985319799185,
7.34831081257529));
#56853=CARTESIAN_POINT('Ctrl Pts',(-6.9999984763219,-22.803174991709,7.27213995952607));
#56854=CARTESIAN_POINT('Ctrl Pts',(-6.99999902465916,-22.7402496061458,
7.22187536553239));
#56855=CARTESIAN_POINT('Ctrl Pts',(-6.99999953898004,-22.6769257511323,
7.17242593768393));
#56856=CARTESIAN_POINT('Ctrl Pts',(-6.99999996276703,-22.6132249339512,
7.123793362472));
#56857=CARTESIAN_POINT('Ctrl Pts',(-7.00000126736887,-22.4171259390615,
6.97408101120292));
#56858=CARTESIAN_POINT('Ctrl Pts',(-7.00000171385138,-22.2174580789129,
6.83211162083866));
#56859=CARTESIAN_POINT('Ctrl Pts',(-7.00000170643233,-22.0149140870436,
6.69789048236768));
#56860=CARTESIAN_POINT('Ctrl Pts',(-7.00000169893394,-21.8102044420194,
6.56223421649901));
#56861=CARTESIAN_POINT('Ctrl Pts',(-7.00000122940959,-21.6025568059502,
6.43449274577891));
#56862=CARTESIAN_POINT('Ctrl Pts',(-7.00000072342098,-21.3926392985623,
6.31464641178277));
#56863=CARTESIAN_POINT('Ctrl Pts',(-7.00000046988466,-21.2874556815005,
6.25459486554357));
#56864=CARTESIAN_POINT('Ctrl Pts',(-7.00000020716533,-21.181701431279,6.19652518159974));
#56865=CARTESIAN_POINT('Ctrl Pts',(-6.99999998766531,-21.0754562644221,
6.14043259863199));
#56866=CARTESIAN_POINT('Ctrl Pts',(-6.99999993929023,-21.0520411488934,
6.12807048984769));
#56867=CARTESIAN_POINT('Ctrl Pts',(-6.99999989300831,-21.0286021782591,
6.11580440433564));
#56868=CARTESIAN_POINT('Ctrl Pts',(-6.99999984878695,-21.0051402164893,
6.10363414171722));
#56869=CARTESIAN_POINT('Ctrl Pts',(-6.99999965374734,-20.9016605318255,
6.04995683415067));
#56870=CARTESIAN_POINT('Ctrl Pts',(-6.9999994986378,-20.7977338128376,5.99814360645079));
#56871=CARTESIAN_POINT('Ctrl Pts',(-6.99999938184552,-20.6934325505225,
5.94817680192591));
#56872=CARTESIAN_POINT('Ctrl Pts',(-6.99999932344938,-20.6412819193649,
5.92319339966347));
#56873=CARTESIAN_POINT('Ctrl Pts',(-6.99999927466388,-20.5890376523755,
5.89867160319478));
#56874=CARTESIAN_POINT('Ctrl Pts',(-6.99999923547139,-20.5367085182238,
5.8746091226682));
#56875=CARTESIAN_POINT('Ctrl Pts',(-6.99999921587514,-20.5105439511479,
5.86257788240491));
#56876=CARTESIAN_POINT('Ctrl Pts',(-6.99999919867917,-20.4843581672814,
5.85066147112715));
#56877=CARTESIAN_POINT('Ctrl Pts',(-6.99999918389325,-20.4581522540645,
5.83885960020213));
#56878=CARTESIAN_POINT('Ctrl Pts',(-6.99999917282793,-20.4385405914925,
5.83002745959391));
#56879=CARTESIAN_POINT('Ctrl Pts',(-6.99999916268469,-20.4179924212598,
5.82084773391597));
#56880=CARTESIAN_POINT('Ctrl Pts',(-6.99999915445603,-20.3985849927827,
5.8122457053959));
#56881=CARTESIAN_POINT('Ctrl Pts',(-6.99999915168922,-20.3920594140724,
5.80935334826356));
#56882=CARTESIAN_POINT('Ctrl Pts',(-6.99999914912883,-20.3856629887566,
5.80652589257862));
#56883=CARTESIAN_POINT('Ctrl Pts',(-6.99999914678339,-20.3794752088658,
5.80379731846812));
#56884=CARTESIAN_POINT('Ctrl Pts',(-6.9999990752884,-20.1908565965901,5.72062372934665));
#56885=CARTESIAN_POINT('Ctrl Pts',(-6.99999912491181,-19.9974675950207,
5.64168486729232));
#56886=CARTESIAN_POINT('Ctrl Pts',(-6.99999933315404,-19.7994486766844,
5.56752055257987));
#56887=CARTESIAN_POINT('Ctrl Pts',(-6.99999947285256,-19.6666084304028,
5.51776770111255));
#56888=CARTESIAN_POINT('Ctrl Pts',(-6.99999968442926,-19.5316854129743,
5.47016413546951));
#56889=CARTESIAN_POINT('Ctrl Pts',(-6.99999998816764,-19.3947330689576,
5.42488006668253));
#56890=CARTESIAN_POINT('Ctrl Pts',(-7.00000042904106,-19.1959480205455,
5.35915066372301));
#56891=CARTESIAN_POINT('Ctrl Pts',(-7.0000010678187,-18.9928853289915,5.29830714986745));
#56892=CARTESIAN_POINT('Ctrl Pts',(-7.00000153332806,-18.7857678324651,
5.24286449209894));
#56893=CARTESIAN_POINT('Ctrl Pts',(-7.00000199136829,-18.5819735465795,
5.18831141456069));
#56894=CARTESIAN_POINT('Ctrl Pts',(-7.0000022813417,-18.3742534735699,5.1389872835667));
#56895=CARTESIAN_POINT('Ctrl Pts',(-7.00000202664213,-18.1628647433994,
5.09540490049247));
#56896=CARTESIAN_POINT('Ctrl Pts',(-7.00000181210257,-17.9848069480198,
5.0586944143595));
#56897=CARTESIAN_POINT('Ctrl Pts',(-7.00000121063512,-17.80414691375,5.02605811832913));
#56898=CARTESIAN_POINT('Ctrl Pts',(-6.99999998662393,-17.6210641954966,
4.99781497974106));
#56899=CARTESIAN_POINT('Ctrl Pts',(-6.99999852879723,-17.4030082841283,
4.96417672385608));
#56900=CARTESIAN_POINT('Ctrl Pts',(-6.99999617282082,-17.1815143987631,
4.93677080855326));
#56901=CARTESIAN_POINT('Ctrl Pts',(-6.99999449839284,-16.9569257604897,
4.91605443614732));
#56902=CARTESIAN_POINT('Ctrl Pts',(-6.99999284818756,-16.7355860789202,
4.89563775208504));
#56903=CARTESIAN_POINT('Ctrl Pts',(-6.99999186150308,-16.5112404840694,
4.88171848973955));
#56904=CARTESIAN_POINT('Ctrl Pts',(-6.9999932006316,-16.2842668363519,4.87474450554359));
#56905=CARTESIAN_POINT('Ctrl Pts',(-6.99999413392928,-16.1260788998259,
4.8698840286538));
#56906=CARTESIAN_POINT('Ctrl Pts',(-6.99999620010592,-15.9666154533927,
4.86839729985613));
#56907=CARTESIAN_POINT('Ctrl Pts',(-6.99999999965515,-15.8060191439725,
4.87043884530665));
#56908=CARTESIAN_POINT('Ctrl Pts',(-7.00000506889193,-15.5917566964629,
4.87316260979731));
#56909=CARTESIAN_POINT('Ctrl Pts',(-7.00001329864027,-15.3754753370598,
4.88216671427478));
#56910=CARTESIAN_POINT('Ctrl Pts',(-7.00001657745847,-15.1576383201127,
4.89779557471497));
#56911=CARTESIAN_POINT('Ctrl Pts',(-7.00001838122166,-15.0378005094032,
4.90639341747505));
#56912=CARTESIAN_POINT('Ctrl Pts',(-7.00001867169788,-14.9174927908483,
4.91699624309555));
#56913=CARTESIAN_POINT('Ctrl Pts',(-7.00001598753836,-14.7967990235774,
4.92966193743282));
#56914=CARTESIAN_POINT('Origin',(-5.9999949808,-24.7867195890602,9.33250914740362));
#56915=CARTESIAN_POINT('Origin',(-6.,-24.7867243677925,9.33251101143268));
#56916=CARTESIAN_POINT('Ctrl Pts',(-7.10781849754849,-14.3668282424248,
7.15238423961458));
#56917=CARTESIAN_POINT('Ctrl Pts',(-7.10965591494416,-14.3272645751604,
7.23049518234384));
#56918=CARTESIAN_POINT('Ctrl Pts',(-7.09650767034188,-14.24557459556,7.40084939111339));
#56919=CARTESIAN_POINT('Ctrl Pts',(-7.01932069946779,-14.1324746587623,
7.66783513591697));
#56920=CARTESIAN_POINT('Ctrl Pts',(-6.87393093371095,-14.0363207135332,
7.93731276018294));
#56921=CARTESIAN_POINT('Ctrl Pts',(-6.66554647804556,-13.9714533100044,
8.17907214581632));
#56922=CARTESIAN_POINT('Ctrl Pts',(-6.44497304084988,-13.9492960538378,
8.34416343581852));
#56923=CARTESIAN_POINT('Ctrl Pts',(-6.29831086878765,-13.953178773167,8.41811502993441));
#56924=CARTESIAN_POINT('Ctrl Pts',(-6.24287185695061,-13.9569870722888,
8.44159546966128));
#56925=CARTESIAN_POINT('Ctrl Pts',(-6.81486607622036,-13.8484436165447,
6.89720921192514));
#56926=CARTESIAN_POINT('Ctrl Pts',(-6.81651062161729,-13.8136823565901,
6.96578564019607));
#56927=CARTESIAN_POINT('Ctrl Pts',(-6.80473712754382,-13.741909218052,7.11584392961594));
#56928=CARTESIAN_POINT('Ctrl Pts',(-6.7353831908826,-13.643029562488,7.35172242011219));
#56929=CARTESIAN_POINT('Ctrl Pts',(-6.60489822284063,-13.5599007723076,
7.58977897617138));
#56930=CARTESIAN_POINT('Ctrl Pts',(-6.41858681323947,-13.505035812957,7.80278611967251));
#56931=CARTESIAN_POINT('Ctrl Pts',(-6.22251417761433,-13.4875789839717,
7.94757981332609));
#56932=CARTESIAN_POINT('Ctrl Pts',(-6.09292712352008,-13.4919494706142,
8.01216517570182));
#56933=CARTESIAN_POINT('Ctrl Pts',(-6.04406306240266,-13.4955820115897,
8.0326475226799));
#56934=CARTESIAN_POINT('Ctrl Pts',(-7.05538134256208,-13.3135799379892,
6.62096627384063));
#56935=CARTESIAN_POINT('Ctrl Pts',(-7.05754284225227,-13.2686353298782,
6.70971021341623));
#56936=CARTESIAN_POINT('Ctrl Pts',(-7.04209110909695,-13.1762830686347,
6.90226166240641));
#56937=CARTESIAN_POINT('Ctrl Pts',(-6.9520659029282,-13.0486741093228,7.20315705962764));
#56938=CARTESIAN_POINT('Ctrl Pts',(-6.78206031637936,-12.9397227967065,
7.50801065543884));
#56939=CARTESIAN_POINT('Ctrl Pts',(-6.53634723568671,-12.8656252761574,
7.78417451392731));
#56940=CARTESIAN_POINT('Ctrl Pts',(-6.27298557965835,-12.8402907688676,
7.9756085032952));
#56941=CARTESIAN_POINT('Ctrl Pts',(-6.09561262360936,-12.8453667962591,
8.062709846792));
#56942=CARTESIAN_POINT('Ctrl Pts',(-6.02821754662008,-12.8501126777228,
8.09054371314276));
#56943=CARTESIAN_POINT('Ctrl Pts',(-7.66703304794012,-13.1269739075718,
6.51199213102435));
#56944=CARTESIAN_POINT('Ctrl Pts',(-7.67007102305416,-13.0637575588475,
6.63694586878494));
#56945=CARTESIAN_POINT('Ctrl Pts',(-7.64838054872756,-12.9342681399641,
6.90599900256435));
#56946=CARTESIAN_POINT('Ctrl Pts',(-7.52318691258873,-12.7544370130884,
7.32399978402674));
#56947=CARTESIAN_POINT('Ctrl Pts',(-7.28601524548368,-12.5983028452235,
7.74862544742454));
#56948=CARTESIAN_POINT('Ctrl Pts',(-6.93967858002702,-12.4887613326707,
8.13707451048743));
#56949=CARTESIAN_POINT('Ctrl Pts',(-6.56283725787951,-12.4483035827522,
8.41049095674551));
#56950=CARTESIAN_POINT('Ctrl Pts',(-6.30520108143084,-12.4538224255438,
8.53673601561792));
#56951=CARTESIAN_POINT('Ctrl Pts',(-6.20672732870885,-12.4602155439728,
8.57729019941276));
#56952=CARTESIAN_POINT('',(-6.26386059986259,-13.9442583573832,8.42071137118441));
#56953=CARTESIAN_POINT('',(-6.24994545432675,-12.4626524975511,8.55169100423493));
#56954=CARTESIAN_POINT('Origin',(-6.52772494237969,-13.2547636785371,9.09519306561096));
#56955=CARTESIAN_POINT('',(-7.00000135336109,-12.5220631623039,8.04447892959546));
#56956=CARTESIAN_POINT('Ctrl Pts',(-7.00000153557987,-12.5220620192528,
8.04447883033673));
#56957=CARTESIAN_POINT('Ctrl Pts',(-6.9736472239779,-12.5156013106946,8.0704984015701));
#56958=CARTESIAN_POINT('Ctrl Pts',(-6.94679742848067,-12.5096416804742,
8.09581844410209));
#56959=CARTESIAN_POINT('Ctrl Pts',(-6.91946610248342,-12.5041754138501,
8.12045448285676));
#56960=CARTESIAN_POINT('Ctrl Pts',(-6.87663070275667,-12.495608331672,8.15906565627172));
#56961=CARTESIAN_POINT('Ctrl Pts',(-6.83261494727981,-12.4882516839534,
8.19599819466153));
#56962=CARTESIAN_POINT('Ctrl Pts',(-6.78747035871098,-12.4820825574771,
8.23129874241077));
#56963=CARTESIAN_POINT('Ctrl Pts',(-6.74232577014216,-12.4759134310009,
8.26659929016002));
#56964=CARTESIAN_POINT('Ctrl Pts',(-6.69605167293783,-12.4709316730476,
8.30026835769235));
#56965=CARTESIAN_POINT('Ctrl Pts',(-6.64865479374424,-12.4671424045176,
8.33232175516477));
#56966=CARTESIAN_POINT('Ctrl Pts',(-6.60367902495548,-12.4635466980453,
8.36273781246942));
#56967=CARTESIAN_POINT('Ctrl Pts',(-6.55771208302904,-12.4610209442456,
8.39169360394873));
#56968=CARTESIAN_POINT('Ctrl Pts',(-6.51072389279704,-12.4595935857182,
8.41917670458322));
#56969=CARTESIAN_POINT('Ctrl Pts',(-6.50378457842987,-12.4593827904207,
8.42323546645818));
#56970=CARTESIAN_POINT('Ctrl Pts',(-6.49682294524356,-12.4591959993429,
8.42726204404947));
#56971=CARTESIAN_POINT('Ctrl Pts',(-6.48983885120465,-12.4590333548863,
8.43125632799246));
#56972=CARTESIAN_POINT('Ctrl Pts',(-6.44329072590013,-12.4579493496445,
8.45787773779083));
#56973=CARTESIAN_POINT('Ctrl Pts',(-6.39574619449289,-12.4579357605457,
8.48306789533459));
#56974=CARTESIAN_POINT('Ctrl Pts',(-6.34718929544507,-12.4590305456602,
8.50678437708271));
#56975=CARTESIAN_POINT('Ctrl Pts',(-6.31521661803976,-12.4597514156494,
8.52240068362187));
#56976=CARTESIAN_POINT('Ctrl Pts',(-6.28280462400267,-12.4609533800672,
8.53737727819511));
#56977=CARTESIAN_POINT('Ctrl Pts',(-6.24994591358957,-12.4626538072098,
8.55169190289375));
#56978=CARTESIAN_POINT('',(-7.000010673963,-13.9487142990898,6.9771195274227));
#56979=CARTESIAN_POINT('Ctrl Pts',(-7.000010673963,-13.9487142990898,6.9771195274227));
#56980=CARTESIAN_POINT('Ctrl Pts',(-7.,-13.8626205647626,7.0142375300983));
#56981=CARTESIAN_POINT('Ctrl Pts',(-7.,-13.7400113857744,7.0701796840634));
#56982=CARTESIAN_POINT('Ctrl Pts',(-7.,-13.62719934054,7.12651956295606));
#56983=CARTESIAN_POINT('Ctrl Pts',(-7.,-13.554168451218,7.16416786553508));
#56984=CARTESIAN_POINT('Ctrl Pts',(-7.,-13.5206011121911,7.18201203080913));
#56985=CARTESIAN_POINT('Ctrl Pts',(-7.,-13.3396119169715,7.28169559221322));
#56986=CARTESIAN_POINT('Ctrl Pts',(-7.,-13.2055602061295,7.36747030450435));
#56987=CARTESIAN_POINT('Ctrl Pts',(-7.,-12.8482282269687,7.63349452399642));
#56988=CARTESIAN_POINT('Ctrl Pts',(-7.,-12.6600994729296,7.82960565015868));
#56989=CARTESIAN_POINT('Ctrl Pts',(-7.000002992026,-12.522063284292,8.04447842282183));
#56990=CARTESIAN_POINT('Ctrl Pts',(-7.00001531395507,-13.9487142989349,
6.97711952775229));
#56991=CARTESIAN_POINT('Ctrl Pts',(-7.00001196725436,-13.9419375604996,
7.02105067161363));
#56992=CARTESIAN_POINT('Ctrl Pts',(-6.99838322763679,-13.9356769258173,
7.06398945097686));
#56993=CARTESIAN_POINT('Ctrl Pts',(-6.99539547590856,-13.9299187481022,
7.105781119514));
#56994=CARTESIAN_POINT('Ctrl Pts',(-6.99268063142182,-13.9246865339005,
7.14375545314008));
#56995=CARTESIAN_POINT('Ctrl Pts',(-6.98884285794656,-13.9198691503561,
7.18078335947894));
#56996=CARTESIAN_POINT('Ctrl Pts',(-6.98405836629357,-13.915452598832,7.21677715725527));
#56997=CARTESIAN_POINT('Ctrl Pts',(-6.97840508132026,-13.9102340665039,
7.25930689935957));
#56998=CARTESIAN_POINT('Ctrl Pts',(-6.97143142900756,-13.9055749039963,
7.30039272111852));
#56999=CARTESIAN_POINT('Ctrl Pts',(-6.96343342004341,-13.9014293624605,
7.3399541376309));
#57000=CARTESIAN_POINT('Ctrl Pts',(-6.95719888813531,-13.8981978693356,
7.37079267690755));
#57001=CARTESIAN_POINT('Ctrl Pts',(-6.95034090819598,-13.8952784336576,
7.40070575569444));
#57002=CARTESIAN_POINT('Ctrl Pts',(-6.94298357137251,-13.8926482456883,
7.42966983265612));
#57003=CARTESIAN_POINT('Ctrl Pts',(-6.93534013200227,-13.8899157783895,
7.45976022697728));
#57004=CARTESIAN_POINT('Ctrl Pts',(-6.92715768677458,-13.8874955281492,
7.488826375215));
#57005=CARTESIAN_POINT('Ctrl Pts',(-6.91856207099106,-13.8853606243187,
7.51685480666478));
#57006=CARTESIAN_POINT('Ctrl Pts',(-6.90689557450206,-13.8824630020109,
7.55489671143773));
#57007=CARTESIAN_POINT('Ctrl Pts',(-6.89447015028134,-13.880090679705,7.59102645975311));
#57008=CARTESIAN_POINT('Ctrl Pts',(-6.88159132787961,-13.8781602348909,
7.62525966990753));
#57009=CARTESIAN_POINT('Ctrl Pts',(-6.87269851637784,-13.87682726505,7.64889766067311));
#57010=CARTESIAN_POINT('Ctrl Pts',(-6.86358844439265,-13.8757050158038,
7.67163205004271));
#57011=CARTESIAN_POINT('Ctrl Pts',(-6.85434935575237,-13.8747664057238,
7.69347522038107));
#57012=CARTESIAN_POINT('Ctrl Pts',(-6.84893640315561,-13.8742164973868,
7.7062725914431));
#57013=CARTESIAN_POINT('Ctrl Pts',(-6.8434789870505,-13.8737296282504,7.71876415637358));
#57014=CARTESIAN_POINT('Ctrl Pts',(-6.83799343682602,-13.8733003913515,
7.73095321827998));
#57015=CARTESIAN_POINT('Ctrl Pts',(-6.83525066171379,-13.8730857729021,
7.73704774923319));
#57016=CARTESIAN_POINT('Ctrl Pts',(-6.83250084470304,-13.8728855666253,
7.74306665076591));
#57017=CARTESIAN_POINT('Ctrl Pts',(-6.82974592766377,-13.872699095121,7.74901040061493));
#57018=CARTESIAN_POINT('Ctrl Pts',(-6.82836846914414,-13.8726058593689,
7.75198227553944));
#57019=CARTESIAN_POINT('Ctrl Pts',(-6.82698973509903,-13.872516057556,7.75493536232424));
#57020=CARTESIAN_POINT('Ctrl Pts',(-6.82560996394253,-13.872429605776,7.75786972160125));
#57021=CARTESIAN_POINT('Ctrl Pts',(-6.82452960945506,-13.8723619144287,
7.76016731145725));
#57022=CARTESIAN_POINT('Ctrl Pts',(-6.82391452016856,-13.8723244082979,
7.76147074725261));
#57023=CARTESIAN_POINT('Ctrl Pts',(-6.82267100507654,-13.8722506715508,
7.76408867684986));
#57024=CARTESIAN_POINT('Ctrl Pts',(-6.8223263689862,-13.8722302356555,7.76481422736948));
#57025=CARTESIAN_POINT('Ctrl Pts',(-6.82193326623848,-13.8722071152214,
7.76564063362551));
#57026=CARTESIAN_POINT('Ctrl Pts',(-6.82146777483655,-13.8721802171765,
7.76661667804998));
#57027=CARTESIAN_POINT('Ctrl Pts',(-6.81268227350425,-13.8716725540741,
7.78503815598937));
#57028=CARTESIAN_POINT('Ctrl Pts',(-6.80362642075091,-13.8712922492689,
7.80321393195674));
#57029=CARTESIAN_POINT('Ctrl Pts',(-6.79431175107884,-13.8710418067265,
7.82113300705971));
#57030=CARTESIAN_POINT('Ctrl Pts',(-6.76482339153055,-13.8702489563092,
7.87786117327623));
#57031=CARTESIAN_POINT('Ctrl Pts',(-6.73274529262462,-13.8707559817329,
7.93201589777643));
#57032=CARTESIAN_POINT('Ctrl Pts',(-6.69853355487696,-13.8725797524819,
7.98334468488858));
#57033=CARTESIAN_POINT('Ctrl Pts',(-6.67146133661983,-13.8740229273399,
8.02396185955019));
#57034=CARTESIAN_POINT('Ctrl Pts',(-6.64305173670006,-13.8762911892378,
8.06280960604313));
#57035=CARTESIAN_POINT('Ctrl Pts',(-6.61350999833252,-13.8794004662696,
8.09976844127926));
#57036=CARTESIAN_POINT('Ctrl Pts',(-6.57430865524071,-13.8835264196638,
8.14881213540246));
#57037=CARTESIAN_POINT('Ctrl Pts',(-6.53311592434715,-13.8891322960673,
8.19452984729646));
#57038=CARTESIAN_POINT('Ctrl Pts',(-6.49047916504889,-13.8961820066511,
8.23675918782889));
#57039=CARTESIAN_POINT('Ctrl Pts',(-6.45748241493318,-13.9016378044732,
8.26944063501282));
#57040=CARTESIAN_POINT('Ctrl Pts',(-6.42361956793115,-13.9079589374026,
8.30003283848111));
#57041=CARTESIAN_POINT('Ctrl Pts',(-6.38912483192341,-13.9151350828458,
8.3284657400435));
#57042=CARTESIAN_POINT('Ctrl Pts',(-6.34811702764754,-13.923666180684,8.36226715432317));
#57043=CARTESIAN_POINT('Ctrl Pts',(-6.3062172665435,-13.9334050780639,8.39301733581296));
#57044=CARTESIAN_POINT('Ctrl Pts',(-6.26385533693063,-13.944272110215,8.42069791742242));
#57045=CARTESIAN_POINT('Ctrl Pts',(-6.22266624523242,-13.1134067202412,
7.49367548860228));
#57046=CARTESIAN_POINT('Ctrl Pts',(-6.22400178812049,-13.3673833259686,
7.81350053545753));
#57047=CARTESIAN_POINT('Ctrl Pts',(-6.22726137937113,-14.0755222713343,
8.61699794739643));
#57048=CARTESIAN_POINT('Ctrl Pts',(-6.23204990885402,-15.3875902517813,
9.75631894437));
#57049=CARTESIAN_POINT('Ctrl Pts',(-6.23570372463157,-17.0892601163741,
10.7961455412244));
#57050=CARTESIAN_POINT('Ctrl Pts',(-6.23759289250501,-18.9411594552768,
11.5416374931887));
#57051=CARTESIAN_POINT('Ctrl Pts',(-6.23804008865557,-20.8893388524382,
11.9701371034134));
#57052=CARTESIAN_POINT('Ctrl Pts',(-6.23649323743614,-22.7260228677799,
12.0627646689595));
#57053=CARTESIAN_POINT('Ctrl Pts',(-6.23490544880393,-23.8924620062907,
11.9504784886639));
#57054=CARTESIAN_POINT('Ctrl Pts',(-6.23413015604773,-24.3933788481534,
11.8700337879013));
#57055=CARTESIAN_POINT('Ctrl Pts',(-6.71588929286535,-13.2016794929268,
7.4236862634343));
#57056=CARTESIAN_POINT('Ctrl Pts',(-6.7170780227433,-13.4537900664687,7.74006838987067));
#57057=CARTESIAN_POINT('Ctrl Pts',(-6.71993255761527,-14.1564698677512,
8.53486272988918));
#57058=CARTESIAN_POINT('Ctrl Pts',(-6.72416341759993,-15.4574006729724,
9.66125897962087));
#57059=CARTESIAN_POINT('Ctrl Pts',(-6.72736708396084,-17.1431707229581,
10.6891581223397));
#57060=CARTESIAN_POINT('Ctrl Pts',(-6.72902314017145,-18.9767975202637,
11.4262596780397));
#57061=CARTESIAN_POINT('Ctrl Pts',(-6.729418137548,-20.9054811851494,11.8502316486358));
#57062=CARTESIAN_POINT('Ctrl Pts',(-6.72805060186563,-22.7235295527145,
11.9427141202896));
#57063=CARTESIAN_POINT('Ctrl Pts',(-6.72668232438883,-23.8785264249907,
11.8323462288572));
#57064=CARTESIAN_POINT('Ctrl Pts',(-6.72598917760879,-24.3745541293715,
11.7530879245913));
#57065=CARTESIAN_POINT('Ctrl Pts',(-7.02184873732211,-13.5171480157836,
7.17355847929394));
#57066=CARTESIAN_POINT('Ctrl Pts',(-7.02249169755403,-13.761025178858,7.47887640233898));
#57067=CARTESIAN_POINT('Ctrl Pts',(-7.02397836398706,-14.4407070320375,
8.24599948969163));
#57068=CARTESIAN_POINT('Ctrl Pts',(-7.02622840850876,-15.6982395182498,
9.33267651195289));
#57069=CARTESIAN_POINT('Ctrl Pts',(-7.02790175945528,-17.3268272034312,
10.324216053706));
#57070=CARTESIAN_POINT('Ctrl Pts',(-7.02876630077243,-19.0974433038976,
11.0353404974063));
#57071=CARTESIAN_POINT('Ctrl Pts',(-7.02897622079789,-20.9601356307836,
11.4446333981564));
#57072=CARTESIAN_POINT('Ctrl Pts',(-7.02824791678565,-22.715199269257,11.5344330888327));
#57073=CARTESIAN_POINT('Ctrl Pts',(-7.02756296992534,-23.8309176176107,
11.428361781308));
#57074=CARTESIAN_POINT('Ctrl Pts',(-7.02718428486759,-24.3100043035356,
11.3520791719536));
#57075=CARTESIAN_POINT('Ctrl Pts',(-6.99898915412488,-13.9127665915938,
6.85988131050602));
#57076=CARTESIAN_POINT('Ctrl Pts',(-6.99894179668946,-14.145881846675,7.15167007590343));
#57077=CARTESIAN_POINT('Ctrl Pts',(-6.99873531343826,-14.7957492487078,
7.88504931885052));
#57078=CARTESIAN_POINT('Ctrl Pts',(-6.99850468231058,-15.9978536408711,
8.92372179840947));
#57079=CARTESIAN_POINT('Ctrl Pts',(-6.99828080313005,-17.5546304272577,
9.87141292198114));
#57080=CARTESIAN_POINT('Ctrl Pts',(-6.99816433581835,-19.2468664594383,
10.5510790379293));
#57081=CARTESIAN_POINT('Ctrl Pts',(-6.99814256681603,-21.0278289481731,
10.9423825331985));
#57082=CARTESIAN_POINT('Ctrl Pts',(-6.99821545410145,-22.7049144947482,
11.0282138212458));
#57083=CARTESIAN_POINT('Ctrl Pts',(-6.99835921777661,-23.7718253340107,
10.9268165340741));
#57084=CARTESIAN_POINT('Ctrl Pts',(-6.99838071860773,-24.2298152555024,
10.8539128099021));
#57085=CARTESIAN_POINT('',(-7.00000355772208,-24.1259406808709,10.9277699403668));
#57086=CARTESIAN_POINT('Ctrl Pts',(-7.00001601661638,-13.9487142989383,
6.97711952757068));
#57087=CARTESIAN_POINT('Ctrl Pts',(-7.0000208899967,-14.0875641914622,7.14852817466841));
#57088=CARTESIAN_POINT('Ctrl Pts',(-7.00001598309392,-14.2303294492748,
7.31421349415626));
#57089=CARTESIAN_POINT('Ctrl Pts',(-7.00000988157693,-14.3764171187408,
7.47407283197781));
#57090=CARTESIAN_POINT('Ctrl Pts',(-7.00000652467739,-14.4567908408787,
7.56202337596396));
#57091=CARTESIAN_POINT('Ctrl Pts',(-7.00000279094487,-14.5381709421536,
7.64821104957978));
#57092=CARTESIAN_POINT('Ctrl Pts',(-6.99999999965532,-14.6204637846073,
7.73262309097843));
#57093=CARTESIAN_POINT('Ctrl Pts',(-6.99999455422719,-14.7810059823021,
7.89729955899171));
#57094=CARTESIAN_POINT('Ctrl Pts',(-6.99999266080992,-14.945019436017,8.05521668450506));
#57095=CARTESIAN_POINT('Ctrl Pts',(-6.99999257345228,-15.1118937759786,
8.20640356290913));
#57096=CARTESIAN_POINT('Ctrl Pts',(-6.9999924848297,-15.2811844415535,8.35977961387709));
#57097=CARTESIAN_POINT('Ctrl Pts',(-6.99999425319344,-15.4534194630651,
8.50622915340521));
#57098=CARTESIAN_POINT('Ctrl Pts',(-6.99999619757815,-15.6280064747247,
8.64581249887252));
#57099=CARTESIAN_POINT('Ctrl Pts',(-6.99999754424659,-15.748924324796,8.74248703313042));
#57100=CARTESIAN_POINT('Ctrl Pts',(-6.99999897835357,-15.8709713329882,
8.83586857884188));
#57101=CARTESIAN_POINT('Ctrl Pts',(-6.99999998662269,-15.9939629279854,
8.9259851708091));
#57102=CARTESIAN_POINT('Ctrl Pts',(-7.00000143709205,-16.1708953932809,
9.05562452365383));
#57103=CARTESIAN_POINT('Ctrl Pts',(-7.00000201442324,-16.3497802017751,
9.17850669010871));
#57104=CARTESIAN_POINT('Ctrl Pts',(-7.00000210876028,-16.5300360475593,
9.29479664869584));
#57105=CARTESIAN_POINT('Ctrl Pts',(-7.00000220461145,-16.7131850374667,
9.41295308550352));
#57106=CARTESIAN_POINT('Ctrl Pts',(-7.00000180216989,-16.8977494586252,
9.52430405378974));
#57107=CARTESIAN_POINT('Ctrl Pts',(-7.00000129011899,-17.0831708595521,
9.62904042803331));
#57108=CARTESIAN_POINT('Ctrl Pts',(-7.00000086166997,-17.2383187546504,
9.71667663357862));
#57109=CARTESIAN_POINT('Ctrl Pts',(-7.00000035619232,-17.3940675908991,
9.79968217694013));
#57110=CARTESIAN_POINT('Ctrl Pts',(-6.99999998816673,-17.5501167583814,
9.87817778675338));
#57111=CARTESIAN_POINT('Ctrl Pts',(-6.99999970373341,-17.6707213695673,
9.93884413091956));
#57112=CARTESIAN_POINT('Ctrl Pts',(-6.99999950019767,-17.7915058619037,
9.99681685260602));
#57113=CARTESIAN_POINT('Ctrl Pts',(-6.99999936067302,-17.9123403031843,
10.0521635783821));
#57114=CARTESIAN_POINT('Ctrl Pts',(-6.99999924478736,-18.012702337443,10.0981331705744));
#57115=CARTESIAN_POINT('Ctrl Pts',(-6.99999917321303,-18.113098981996,10.1422912426454));
#57116=CARTESIAN_POINT('Ctrl Pts',(-6.99999913936356,-18.2134600364446,
10.1846774364508));
#57117=CARTESIAN_POINT('Ctrl Pts',(-6.99999912243883,-18.263640563669,10.2058705333535));
#57118=CARTESIAN_POINT('Ctrl Pts',(-6.99999911498667,-18.3138121933672,
10.2266206606898));
#57119=CARTESIAN_POINT('Ctrl Pts',(-6.99999911640001,-18.363966570749,10.2469328594148));
#57120=CARTESIAN_POINT('Ctrl Pts',(-6.99999911710669,-18.38904375944,10.2570889587773));
#57121=CARTESIAN_POINT('Ctrl Pts',(-6.99999912003194,-18.4141166350518,
10.267135575987));
#57122=CARTESIAN_POINT('Ctrl Pts',(-6.99999912511209,-18.4391841642749,
10.2770733432481));
#57123=CARTESIAN_POINT('Ctrl Pts',(-6.99999912765217,-18.4517179288864,
10.2820422268787));
#57124=CARTESIAN_POINT('Ctrl Pts',(-6.9999991307311,-18.4642503569007,10.2869838980222));
#57125=CARTESIAN_POINT('Ctrl Pts',(-6.99999913434161,-18.4767813206209,
10.2918984359962));
#57126=CARTESIAN_POINT('Ctrl Pts',(-6.99999913749792,-18.4877358923424,
10.2961947263628));
#57127=CARTESIAN_POINT('Ctrl Pts',(-6.99999914056844,-18.4972872792251,
10.2999248791717));
#57128=CARTESIAN_POINT('Ctrl Pts',(-6.99999914483372,-18.5091123692525,
10.304519538847));
#57129=CARTESIAN_POINT('Ctrl Pts',(-6.99999914544751,-18.51081403115,10.3051807225913));
#57130=CARTESIAN_POINT('Ctrl Pts',(-6.99999914608798,-18.5125628082469,
10.3058597278899));
#57131=CARTESIAN_POINT('Ctrl Pts',(-6.99999914676108,-18.5143696916372,
10.3065607298132));
#57132=CARTESIAN_POINT('Ctrl Pts',(-6.99999923697285,-18.7565377825937,
10.4005127238446));
#57133=CARTESIAN_POINT('Ctrl Pts',(-6.99999952144574,-19.0001638637106,
10.4851669222284));
#57134=CARTESIAN_POINT('Ctrl Pts',(-6.99999999018471,-19.244534524912,10.5606726979753));
#57135=CARTESIAN_POINT('Ctrl Pts',(-7.00000044364542,-19.4809400670551,
10.6337174070357));
#57136=CARTESIAN_POINT('Ctrl Pts',(-7.00000106797163,-19.7180423326575,
10.6982012217175));
#57137=CARTESIAN_POINT('Ctrl Pts',(-7.0000014259335,-19.9551820387299,10.7543686705225));
#57138=CARTESIAN_POINT('Ctrl Pts',(-7.00000178765883,-20.1948149383802,
10.8111266417876));
#57139=CARTESIAN_POINT('Ctrl Pts',(-7.00000187627607,-20.434486106489,10.8593924797692));
#57140=CARTESIAN_POINT('Ctrl Pts',(-7.00000131559751,-20.6735682031901,
10.8994248121704));
#57141=CARTESIAN_POINT('Ctrl Pts',(-7.0000010387385,-20.7916252129104,10.9191924882977));
#57142=CARTESIAN_POINT('Ctrl Pts',(-7.00000060481346,-20.9095393943468,
10.9369526723741));
#57143=CARTESIAN_POINT('Ctrl Pts',(-6.99999997635832,-21.0272398537476,
10.9527370359073));
#57144=CARTESIAN_POINT('Ctrl Pts',(-6.9999988792805,-21.232706487677,10.980291389224));
#57145=CARTESIAN_POINT('Ctrl Pts',(-6.99999719586413,-21.4375204945477,
11.0018248526799));
#57146=CARTESIAN_POINT('Ctrl Pts',(-6.99999590263476,-21.6413538432379,
11.0175572522402));
#57147=CARTESIAN_POINT('Ctrl Pts',(-6.9999956817133,-21.6761745497693,11.0202448069099));
#57148=CARTESIAN_POINT('Ctrl Pts',(-6.99999546002091,-21.7128790072846,
11.0229065232472));
#57149=CARTESIAN_POINT('Ctrl Pts',(-6.99999525388523,-21.7501370397694,
11.0254108052772));
#57150=CARTESIAN_POINT('Ctrl Pts',(-6.99999512029735,-21.774282404631,11.0270337252034));
#57151=CARTESIAN_POINT('Ctrl Pts',(-6.9999949932366,-21.7986601648793,11.0285915128656));
#57152=CARTESIAN_POINT('Ctrl Pts',(-6.99999487630705,-21.8229073894779,
11.030060139636));
#57153=CARTESIAN_POINT('Ctrl Pts',(-6.99999457894682,-21.8845698234527,
11.0337949630133));
#57154=CARTESIAN_POINT('Ctrl Pts',(-6.99999434327587,-21.9460668090055,
11.0369990881757));
#57155=CARTESIAN_POINT('Ctrl Pts',(-6.99999419420496,-22.0073890961152,
11.0396820791216));
#57156=CARTESIAN_POINT('Ctrl Pts',(-6.99999365475099,-22.2293006052878,
11.0493912174785));
#57157=CARTESIAN_POINT('Ctrl Pts',(-6.99999426200478,-22.448925295387,11.0522756893275));
#57158=CARTESIAN_POINT('Ctrl Pts',(-6.99999708872338,-22.6658896614926,
11.048779376235));
#57159=CARTESIAN_POINT('Ctrl Pts',(-6.99999738650878,-22.6887461356942,
11.0484110512818));
#57160=CARTESIAN_POINT('Ctrl Pts',(-6.9999977087728,-22.7115731328884,11.0479719059811));
#57161=CARTESIAN_POINT('Ctrl Pts',(-6.99999805666166,-22.7343702493888,
11.0474624543948));
#57162=CARTESIAN_POINT('Ctrl Pts',(-6.99999863110505,-22.7720134588844,
11.0466212342873));
#57163=CARTESIAN_POINT('Ctrl Pts',(-6.99999927542386,-22.8095751947521,
11.0455883208263));
#57164=CARTESIAN_POINT('Ctrl Pts',(-6.99999999465561,-22.8470536771216,
11.0443660224837));
#57165=CARTESIAN_POINT('Ctrl Pts',(-7.00000393348179,-23.0523021636611,
11.037672184605));
#57166=CARTESIAN_POINT('Ctrl Pts',(-7.00001006471103,-23.2550496791979,
11.0252996505177));
#57167=CARTESIAN_POINT('Ctrl Pts',(-7.00001375741216,-23.4549524564073,
11.0076812098584));
#57168=CARTESIAN_POINT('Ctrl Pts',(-7.00001750460198,-23.6578049557541,
10.9898027953));
#57169=CARTESIAN_POINT('Ctrl Pts',(-7.00001874206956,-23.8577282246578,
10.9665225331668));
#57170=CARTESIAN_POINT('Ctrl Pts',(-7.00001328593478,-24.0544142486451,
10.9382773269549));
#57171=CARTESIAN_POINT('Ctrl Pts',(-7.00001262322331,-24.0783040696869,
10.9348466158753));
#57172=CARTESIAN_POINT('Ctrl Pts',(-7.00001186252947,-24.1021461920723,
10.931342638763));
#57173=CARTESIAN_POINT('Ctrl Pts',(-7.00001099698697,-24.1259401133989,
10.9277661632342));
#57174=CARTESIAN_POINT('',(-6.271594443024,-24.2690120587724,11.8794941632625));
#57175=CARTESIAN_POINT('Origin',(-5.99998362344489,-24.1259473025315,10.9277594521136));
#57176=CARTESIAN_POINT('Ctrl Pts',(-6.26386059994277,-13.9442583574975,
8.42071137126985));
#57177=CARTESIAN_POINT('Ctrl Pts',(-6.26455151926992,-14.1129907025116,
8.59292006661441));
#57178=CARTESIAN_POINT('Ctrl Pts',(-6.26520985451036,-14.2852415147495,
8.75834742231281));
#57179=CARTESIAN_POINT('Ctrl Pts',(-6.26583560625273,-14.4604056907354,
8.91699490798369));
#57180=CARTESIAN_POINT('Ctrl Pts',(-6.2664706593002,-14.6381735437629,9.07800056314788));
#57181=CARTESIAN_POINT('Ctrl Pts',(-6.26707215299456,-14.8189420279879,
9.23202334515509));
#57182=CARTESIAN_POINT('Ctrl Pts',(-6.26764008795109,-15.002122358651,9.37909676806481));
#57183=CARTESIAN_POINT('Ctrl Pts',(-6.2681246797852,-15.1584214055542,9.50458751121598));
#57184=CARTESIAN_POINT('Ctrl Pts',(-6.26858483953038,-15.3164771401929,
9.62501942153129));
#57185=CARTESIAN_POINT('Ctrl Pts',(-6.26902056756885,-15.4759481442486,
9.74043079561972));
#57186=CARTESIAN_POINT('Ctrl Pts',(-6.26953467271229,-15.6641041869533,
9.87660192942662));
#57187=CARTESIAN_POINT('Ctrl Pts',(-6.27001476628493,-15.854228787839,10.0057843668122));
#57188=CARTESIAN_POINT('Ctrl Pts',(-6.27046084891459,-16.0457320728812,
10.1281573929876));
#57189=CARTESIAN_POINT('Ctrl Pts',(-6.27062083229436,-16.1144129421647,
10.1720453388927));
#57190=CARTESIAN_POINT('Ctrl Pts',(-6.27077644107981,-16.1832716087534,
10.2150575890123));
#57191=CARTESIAN_POINT('Ctrl Pts',(-6.27092767529992,-16.2522824065319,
10.2572029123285));
#57192=CARTESIAN_POINT('Ctrl Pts',(-6.27136815555626,-16.4532811875826,
10.3799541177375));
#57193=CARTESIAN_POINT('Ctrl Pts',(-6.27177152514005,-16.6555663828579,
10.4953498370541));
#57194=CARTESIAN_POINT('Ctrl Pts',(-6.27213778405132,-16.8585418317145,
10.6036186785427));
#57195=CARTESIAN_POINT('Ctrl Pts',(-6.27250404296258,-17.0615172805711,
10.7118875200312));
#57196=CARTESIAN_POINT('Ctrl Pts',(-6.27283319120131,-17.2651831715053,
10.8130295873899));
#57197=CARTESIAN_POINT('Ctrl Pts',(-6.2731252287675,-17.4689976408962,10.9072900318684));
#57198=CARTESIAN_POINT('Ctrl Pts',(-6.27334042212229,-17.6191821530989,
10.9767476072619));
#57199=CARTESIAN_POINT('Ctrl Pts',(-6.27353526468669,-17.7691757844474,
11.0423478542931));
#57200=CARTESIAN_POINT('Ctrl Pts',(-6.27370997818747,-17.9190755247098,
11.1043414442314));
#57201=CARTESIAN_POINT('Ctrl Pts',(-6.27388469168824,-18.0689752649722,
11.1663350341698));
#57202=CARTESIAN_POINT('Ctrl Pts',(-6.27403927612539,-18.2187815399094,
11.2247220111681));
#57203=CARTESIAN_POINT('Ctrl Pts',(-6.27417395322568,-18.3686262123569,
11.2797074203491));
#57204=CARTESIAN_POINT('Ctrl Pts',(-6.27427013793896,-18.4756434173988,
11.318977317053));
#57205=CARTESIAN_POINT('Ctrl Pts',(-6.27435616863818,-18.5826809229142,
11.3565113020647));
#57206=CARTESIAN_POINT('Ctrl Pts',(-6.27443212609425,-18.6897917166758,
11.3923810248371));
#57207=CARTESIAN_POINT('Ctrl Pts',(-6.27457884517869,-18.8966864496993,
11.4616668218703));
#57208=CARTESIAN_POINT('Ctrl Pts',(-6.27469165501223,-19.1080556828696,
11.5261455889694));
#57209=CARTESIAN_POINT('Ctrl Pts',(-6.2747705555949,-19.3236952442391,11.5853118140797));
#57210=CARTESIAN_POINT('Ctrl Pts',(-6.27484862874764,-19.5370733948855,
11.6438575633595));
#57211=CARTESIAN_POINT('Ctrl Pts',(-6.27489350013246,-19.7546328883749,
11.6972016144136));
#57212=CARTESIAN_POINT('Ctrl Pts',(-6.27490516974936,-19.9761300584837,
11.744833566385));
#57213=CARTESIAN_POINT('Ctrl Pts',(-6.2749166457757,-20.1939527499269,11.7916753385486));
#57214=CARTESIAN_POINT('Ctrl Pts',(-6.27489601248373,-20.4155836081791,
11.8329929400541));
#57215=CARTESIAN_POINT('Ctrl Pts',(-6.27484326987345,-20.640745185411,11.8682810499045));
#57216=CARTESIAN_POINT('Ctrl Pts',(-6.27479056731688,-20.865735770765,11.9035423613098));
#57217=CARTESIAN_POINT('Ctrl Pts',(-6.2747058041923,-21.0942518881818,11.9327833696204));
#57218=CARTESIAN_POINT('Ctrl Pts',(-6.2745889804997,-21.3259688314451,11.955479670973));
#57219=CARTESIAN_POINT('Ctrl Pts',(-6.27454781420096,-21.4076211803764,
11.9634773870286));
#57220=CARTESIAN_POINT('Ctrl Pts',(-6.27450266694103,-21.4896705313667,
11.9706622510988));
#57221=CARTESIAN_POINT('Ctrl Pts',(-6.27445353870782,-21.5721011963865,
11.9770107061869));
#57222=CARTESIAN_POINT('Ctrl Pts',(-6.2743162410566,-21.8024684609395,11.9947526015415));
#57223=CARTESIAN_POINT('Ctrl Pts',(-6.27414785108124,-22.0358175732131,
12.0059621189159));
#57224=CARTESIAN_POINT('Ctrl Pts',(-6.27394836851762,-22.2717646560156,
12.0102364739125));
#57225=CARTESIAN_POINT('Ctrl Pts',(-6.27375072701035,-22.5055341456103,
12.014471380206));
#57226=CARTESIAN_POINT('Ctrl Pts',(-6.27352256418332,-22.7418539653979,
12.0118985200148));
#57227=CARTESIAN_POINT('Ctrl Pts',(-6.27326387977963,-22.9803003340606,
12.0021219084666));
#57228=CARTESIAN_POINT('Ctrl Pts',(-6.27300884334362,-23.2153841318392,
11.9924831667023));
#57229=CARTESIAN_POINT('Ctrl Pts',(-6.27272414009183,-23.4525349673461,
11.9758423891121));
#57230=CARTESIAN_POINT('Ctrl Pts',(-6.27240976977808,-23.6912965484798,
11.9518163423101));
#57231=CARTESIAN_POINT('Ctrl Pts',(-6.27215746674537,-23.8829185572408,
11.9325338458174));
#57232=CARTESIAN_POINT('Ctrl Pts',(-6.27188605478029,-24.0755771485926,
11.908494328387));
#57233=CARTESIAN_POINT('Ctrl Pts',(-6.27159553375559,-24.2690121689631,
11.8794980525033));
#57234=CARTESIAN_POINT('Origin',(-5.999994993365,-24.1259380195517,10.9277770074801));
#57235=CARTESIAN_POINT('',(-5.98852246669737,-25.0410395151948,11.3308498388632));
#57236=CARTESIAN_POINT('Origin',(-5.999994993365,-24.1259380195517,10.9277770074801));
#57237=CARTESIAN_POINT('Origin',(-6.,-24.1259427050578,10.9277790633915));
#57238=CARTESIAN_POINT('Ctrl Pts',(-5.98841833134947,-25.040839011132,11.3313022852623));
#57239=CARTESIAN_POINT('Ctrl Pts',(-5.98810627250653,-25.0938945818823,
11.2108442590279));
#57240=CARTESIAN_POINT('Ctrl Pts',(-5.98726405053642,-25.2768814418996,
10.7897532298672));
#57241=CARTESIAN_POINT('Ctrl Pts',(-5.98726405053548,-25.5029619538456,
10.2439465916472));
#57242=CARTESIAN_POINT('Ctrl Pts',(-5.98810627252386,-25.6713270271153,
9.81679901787702));
#57243=CARTESIAN_POINT('Ctrl Pts',(-5.98841833138214,-25.71898776185,9.69410637308692));
#57244=CARTESIAN_POINT('Ctrl Pts',(-6.58019637691559,-25.0471116824598,
11.3340652823765));
#57245=CARTESIAN_POINT('Ctrl Pts',(-6.57988216951981,-25.1003453872547,
11.2136609948753));
#57246=CARTESIAN_POINT('Ctrl Pts',(-6.57903377822269,-25.2838224184272,
10.7926927033354));
#57247=CARTESIAN_POINT('Ctrl Pts',(-6.57903377822185,-25.5099484870406,
10.2467760815894));
#57248=CARTESIAN_POINT('Ctrl Pts',(-6.57988216953611,-25.6778801683539,
9.81936869307563));
#57249=CARTESIAN_POINT('Ctrl Pts',(-6.58019637694761,-25.725376944262,9.69658808751447));
#57250=CARTESIAN_POINT('Ctrl Pts',(-7.0007967752053,-24.6661026364245,11.1662377678248));
#57251=CARTESIAN_POINT('Ctrl Pts',(-7.00061249054646,-24.7189023956179,
11.0471442791618));
#57252=CARTESIAN_POINT('Ctrl Pts',(-7.00011449005887,-24.9007955979718,
10.6307100883018));
#57253=CARTESIAN_POINT('Ctrl Pts',(-7.00011449005883,-25.1245686193591,
10.0904742250701));
#57254=CARTESIAN_POINT('Ctrl Pts',(-7.00061249055608,-25.2904141434231,
9.66739286602032));
#57255=CARTESIAN_POINT('Ctrl Pts',(-7.00079677522358,-25.3372908904342,
9.54584598112046));
#57256=CARTESIAN_POINT('Ctrl Pts',(-6.99999917318215,-24.1245144769952,
10.9276780913239));
#57257=CARTESIAN_POINT('Ctrl Pts',(-6.99999957776327,-24.1765264223433,
10.8103725336039));
#57258=CARTESIAN_POINT('Ctrl Pts',(-7.00000004362099,-24.3557042137786,
10.4001860031049));
#57259=CARTESIAN_POINT('Ctrl Pts',(-7.00000004362179,-24.5761256613181,
9.86804155492472));
#57260=CARTESIAN_POINT('Ctrl Pts',(-6.99999957776352,-24.739473507827,9.45129804439077));
#57261=CARTESIAN_POINT('Ctrl Pts',(-6.99999917318139,-24.7856430652418,
9.33157248614975));
#57262=CARTESIAN_POINT('Origin',(-5.98852353414946,11.4730434400575,-4.75229019210214));
#57263=CARTESIAN_POINT('Origin',(-7.00021006969032,11.4504602414792,-4.74293587756365));
#57264=CARTESIAN_POINT('Ctrl Pts',(-6.05508738338625,-24.9010197753632,
11.6467810610876));
#57265=CARTESIAN_POINT('Ctrl Pts',(-4.03672492225717,-24.6398368704069,
12.1727625868536));
#57266=CARTESIAN_POINT('Ctrl Pts',(7.59697586626834E-7,-24.4085091422409,
12.7121411857612));
#57267=CARTESIAN_POINT('Ctrl Pts',(4.03672644165275,-24.6398369574816,12.1727623838323));
#57268=CARTESIAN_POINT('Ctrl Pts',(6.05508966247912,-24.9010200702845,11.646780467159));
#57269=CARTESIAN_POINT('Ctrl Pts',(-6.05508738338625,-25.2386170700518,
10.8984824909014));
#57270=CARTESIAN_POINT('Ctrl Pts',(-4.03672492225717,-25.1429604961832,
11.0706884016279));
#57271=CARTESIAN_POINT('Ctrl Pts',(7.59697586626834E-7,-25.1800058610512,
11.3017462712826));
#57272=CARTESIAN_POINT('Ctrl Pts',(4.03672644165275,-25.1429604822486,11.0706883146625));
#57273=CARTESIAN_POINT('Ctrl Pts',(6.05508966247912,-25.2386171780669,10.8984822964536));
#57274=CARTESIAN_POINT('Ctrl Pts',(-6.05508738338625,-25.5530349402587,
10.1393926838645));
#57275=CARTESIAN_POINT('Ctrl Pts',(-4.03672492225717,-25.6072797194157,
9.94969240521292));
#57276=CARTESIAN_POINT('Ctrl Pts',(7.59697586626834E-7,-25.7969468737938,
9.81219748812645));
#57277=CARTESIAN_POINT('Ctrl Pts',(4.03672644165275,-25.6072796480323,9.94969245696381));
#57278=CARTESIAN_POINT('Ctrl Pts',(6.05508966247912,-25.5530348790098,10.1393928980646));
#57279=CARTESIAN_POINT('Ctrl Pts',(-6.05508738338625,-25.8434316995194,
9.37154365087387));
#57280=CARTESIAN_POINT('Ctrl Pts',(-4.03672492225717,-26.0307798045846,
8.81463859944452));
#57281=CARTESIAN_POINT('Ctrl Pts',(7.59697586626834E-7,-26.2486273875397,
8.2693384925856));
#57282=CARTESIAN_POINT('Ctrl Pts',(4.03672644165275,-26.0307797225905,8.81463880469617));
#57283=CARTESIAN_POINT('Ctrl Pts',(6.05508966247912,-25.8434314879758,9.37154427972115));
#57284=CARTESIAN_POINT('Ctrl Pts',(-5.98852262888505,-25.0410393032183,
11.3308502499282));
#57285=CARTESIAN_POINT('Ctrl Pts',(-5.93906438611487,-25.0335296633685,
11.3464916934807));
#57286=CARTESIAN_POINT('Ctrl Pts',(-5.88263517116821,-25.025051050658,11.3641929089859));
#57287=CARTESIAN_POINT('Ctrl Pts',(-5.81916415490276,-25.0156980212809,
11.3837859022183));
#57288=CARTESIAN_POINT('Ctrl Pts',(-5.7580450642156,-25.0066915694493,11.4026528749038));
#57289=CARTESIAN_POINT('Ctrl Pts',(-5.69039610968652,-24.9968744776098,
11.4232739318758));
#57290=CARTESIAN_POINT('Ctrl Pts',(-5.61614355559872,-24.9863500316491,
11.4454588047106));
#57291=CARTESIAN_POINT('Ctrl Pts',(-5.5404621080218,-24.9756230564625,11.4680705964675));
#57292=CARTESIAN_POINT('Ctrl Pts',(-5.45792024476691,-24.9641612467195,
11.4923073176096));
#57293=CARTESIAN_POINT('Ctrl Pts',(-5.36843222079314,-24.9520928381922,
11.5179224145699));
#57294=CARTESIAN_POINT('Ctrl Pts',(-5.32368820880625,-24.9460586339285,
11.5307299630501));
#57295=CARTESIAN_POINT('Ctrl Pts',(-5.27720755800021,-24.9398730715649,
11.543881375116));
#57296=CARTESIAN_POINT('Ctrl Pts',(-5.22897913546587,-24.9335538910092,
11.5573412753069));
#57297=CARTESIAN_POINT('Ctrl Pts',(-5.2048649241987,-24.9303943007313,11.5640712254024));
#57298=CARTESIAN_POINT('Ctrl Pts',(-5.18031377002017,-24.9272013022212,
11.5708782958756));
#57299=CARTESIAN_POINT('Ctrl Pts',(-5.155324265948,-24.9239772467556,11.57775769834));
#57300=CARTESIAN_POINT('Ctrl Pts',(-5.13033476187583,-24.92075319129,11.5846371008043));
#57301=CARTESIAN_POINT('Ctrl Pts',(-5.10370559285897,-24.9173455615374,
11.5919148457444));
#57302=CARTESIAN_POINT('Ctrl Pts',(-5.07903930494025,-24.9142142529198,
11.5986080780921));
#57303=CARTESIAN_POINT('Ctrl Pts',(-5.0641312898593,-24.9123217267218,11.602653389211));
#57304=CARTESIAN_POINT('Ctrl Pts',(-5.04933271581953,-24.9104524028187,
11.6066511137227));
#57305=CARTESIAN_POINT('Ctrl Pts',(-5.03464390372513,-24.9086058757351,
11.610601946104));
#57306=CARTESIAN_POINT('Ctrl Pts',(-4.9171682275508,-24.8938380363538,11.6421992395044));
#57307=CARTESIAN_POINT('Ctrl Pts',(-4.80671569496028,-24.8805262788085,
11.670799962657));
#57308=CARTESIAN_POINT('Ctrl Pts',(-4.70342530185199,-24.8684850080852,
11.6967442810817));
#57309=CARTESIAN_POINT('Ctrl Pts',(-4.60047418857305,-24.8564832895424,
11.7226033797327));
#57310=CARTESIAN_POINT('Ctrl Pts',(-4.50463793164033,-24.8457437447952,
11.7458237648518));
#57311=CARTESIAN_POINT('Ctrl Pts',(-4.41602613739422,-24.8361073394874,
11.7667065466625));
#57312=CARTESIAN_POINT('Ctrl Pts',(-4.3839468301148,-24.8326187609119,11.774266546776));
#57313=CARTESIAN_POINT('Ctrl Pts',(-4.3528141094931,-24.8292749926518,11.7815198237035));
#57314=CARTESIAN_POINT('Ctrl Pts',(-4.32263238067729,-24.8260692849391,
11.7884794050893));
#57315=CARTESIAN_POINT('Ctrl Pts',(-4.28802312693375,-24.8223933142107,
11.7964599260065));
#57316=CARTESIAN_POINT('Ctrl Pts',(-4.25466435340653,-24.8188988662361,
11.8040542901814));
#57317=CARTESIAN_POINT('Ctrl Pts',(-4.22256207115286,-24.815576452521,11.811280988239));
#57318=CARTESIAN_POINT('Ctrl Pts',(-4.20651093002602,-24.8139152456634,
11.8148943372678));
#57319=CARTESIAN_POINT('Ctrl Pts',(-4.190773911718,-24.8122970494496,11.8184157707246));
#57320=CARTESIAN_POINT('Ctrl Pts',(-4.1753516959697,-24.8107207574243,11.8218474581548));
#57321=CARTESIAN_POINT('Ctrl Pts',(-4.16764058809556,-24.8099326114116,
11.8235633018699));
#57322=CARTESIAN_POINT('Ctrl Pts',(-4.16000818086133,-24.8091549415643,
11.8252567091328));
#57323=CARTESIAN_POINT('Ctrl Pts',(-4.15245455747703,-24.8083876122322,
11.8269279471741));
#57324=CARTESIAN_POINT('Ctrl Pts',(-4.14867774578487,-24.8080039475662,
11.8277635661948));
#57325=CARTESIAN_POINT('Ctrl Pts',(-4.1449206300552,-24.8076228680358,11.8285936429134));
#57326=CARTESIAN_POINT('Ctrl Pts',(-4.14118322045561,-24.807244356959,11.8294182102471));
#57327=CARTESIAN_POINT('Ctrl Pts',(-4.13931451565582,-24.8070551014206,
11.8298304939139));
#57328=CARTESIAN_POINT('Ctrl Pts',(-4.13745073738855,-24.806866487996,11.8302414002347));
#57329=CARTESIAN_POINT('Ctrl Pts',(-4.13559188690975,-24.8066785146178,
11.8306509332919));
#57330=CARTESIAN_POINT('Ctrl Pts',(-4.13373303643096,-24.8064905412396,
11.8310604663492));
#57331=CARTESIAN_POINT('Ctrl Pts',(-4.13363444561665,-24.8064804460971,
11.8310824417452));
#57332=CARTESIAN_POINT('Ctrl Pts',(-4.1300301200903,-24.8061165125615,11.8318754167459));
#57333=CARTESIAN_POINT('Ctrl Pts',(-4.08661760546933,-24.8017330933015,
11.8414264516245));
#57334=CARTESIAN_POINT('Ctrl Pts',(-4.04433457950343,-24.7975362580896,
11.85058237988));
#57335=CARTESIAN_POINT('Ctrl Pts',(-4.00318800196471,-24.7935150283471,
11.8593643927378));
#57336=CARTESIAN_POINT('Ctrl Pts',(-3.9000460902361,-24.783435032684,11.8813782186539));
#57337=CARTESIAN_POINT('Ctrl Pts',(-3.80404668802037,-24.7744568319423,
11.9010453906012));
#57338=CARTESIAN_POINT('Ctrl Pts',(-3.71528285757527,-24.7664251263882,
11.9186746484402));
#57339=CARTESIAN_POINT('Ctrl Pts',(-3.62703564900393,-24.7584401668426,
11.9362013007452));
#57340=CARTESIAN_POINT('Ctrl Pts',(-3.54593976635268,-24.7513907266947,
11.9517138490167));
#57341=CARTESIAN_POINT('Ctrl Pts',(-3.47206599162342,-24.7451472110363,
11.9654746815673));
#57342=CARTESIAN_POINT('Ctrl Pts',(-3.41362152570288,-24.7402077187812,
11.9763614206299));
#57343=CARTESIAN_POINT('Ctrl Pts',(-3.35969695735051,-24.7357731021218,
11.9861509848192));
#57344=CARTESIAN_POINT('Ctrl Pts',(-3.31031960817658,-24.7317894362562,
11.9949540482286));
#57345=CARTESIAN_POINT('Ctrl Pts',(-3.27705079452021,-24.7291053748482,
12.0008852592206));
#57346=CARTESIAN_POINT('Ctrl Pts',(-3.24584610621182,-24.7266262149396,
12.0063682825194));
#57347=CARTESIAN_POINT('Ctrl Pts',(-3.2167123660793,-24.7243378077796,12.0114324025904));
#57348=CARTESIAN_POINT('Ctrl Pts',(-3.20214549601304,-24.7231936041996,
12.0139644626259));
#57349=CARTESIAN_POINT('Ctrl Pts',(-3.18809636299643,-24.7220970904731,
12.0163917976402));
#57350=CARTESIAN_POINT('Ctrl Pts',(-3.174565693027,-24.7210467076192,12.018717647553));
#57351=CARTESIAN_POINT('Ctrl Pts',(-3.16780035804229,-24.7205215161922,
12.0198805725094));
#57352=CARTESIAN_POINT('Ctrl Pts',(-3.16116463881965,-24.7200078575691,
12.0210181262307));
#57353=CARTESIAN_POINT('Ctrl Pts',(-3.15465862315445,-24.7195055430928,
12.0221307017735));
#57354=CARTESIAN_POINT('Ctrl Pts',(-3.15140561532184,-24.7192543858547,
12.0226869895449));
#57355=CARTESIAN_POINT('Ctrl Pts',(-3.14818503337862,-24.7190060646578,
12.0232370327738));
#57356=CARTESIAN_POINT('Ctrl Pts',(-3.14499688787088,-24.7187605566668,
12.0237808790813));
#57357=CARTESIAN_POINT('Ctrl Pts',(-3.14180874236315,-24.7185150486758,
12.0243247253888));
#57358=CARTESIAN_POINT('Ctrl Pts',(-3.13695795616954,-24.7181421515035,
12.0251508337765));
#57359=CARTESIAN_POINT('Ctrl Pts',(-3.13552977107616,-24.718032449711,12.0253938744076));
#57360=CARTESIAN_POINT('Ctrl Pts',(-3.11970258360824,-24.7168167313537,
12.0280872575323));
#57361=CARTESIAN_POINT('Ctrl Pts',(-3.0967945756905,-24.7150575346586,12.0319848511427));
#57362=CARTESIAN_POINT('Ctrl Pts',(-3.06678983441689,-24.7127900582804,
12.037012281578));
#57363=CARTESIAN_POINT('Ctrl Pts',(-3.03690027360432,-24.7105312861591,
12.0420204130049));
#57364=CARTESIAN_POINT('Ctrl Pts',(-2.99996827922771,-24.707768137808,12.0481497555868));
#57365=CARTESIAN_POINT('Ctrl Pts',(-2.95596932035526,-24.7045569191481,
12.0552806302816));
#57366=CARTESIAN_POINT('Ctrl Pts',(-2.93821869684115,-24.703261408188,12.0581574590812));
#57367=CARTESIAN_POINT('Ctrl Pts',(-2.91931777485785,-24.7018932144384,
12.0611967667851));
#57368=CARTESIAN_POINT('Ctrl Pts',(-2.89926458877209,-24.7004570277544,
12.0643885313884));
#57369=CARTESIAN_POINT('Ctrl Pts',(-2.84971550087531,-24.6969083776826,
12.0722750100853));
#57370=CARTESIAN_POINT('Ctrl Pts',(-2.79313189875029,-24.6929431371324,
12.0810955571872));
#57371=CARTESIAN_POINT('Ctrl Pts',(-2.72948003773908,-24.6886468787094,
12.0906663764175));
#57372=CARTESIAN_POINT('Ctrl Pts',(-2.66624670467554,-24.6843788693304,
12.100174264961));
#57373=CARTESIAN_POINT('Ctrl Pts',(-2.59603758471431,-24.6797842017353,
12.110422630762));
#57374=CARTESIAN_POINT('Ctrl Pts',(-2.51881566037573,-24.67496750317,12.121184550676));
#57375=CARTESIAN_POINT('Ctrl Pts',(-2.46592222634894,-24.671668288213,12.1285559663179));
#57376=CARTESIAN_POINT('Ctrl Pts',(-2.40973856920156,-24.6682653336581,
12.136167357517));
#57377=CARTESIAN_POINT('Ctrl Pts',(-2.3502524094774,-24.6647978642146,12.143932829769));
#57378=CARTESIAN_POINT('Ctrl Pts',(-2.3184758099704,-24.6629455949083,12.1480810266417));
#57379=CARTESIAN_POINT('Ctrl Pts',(-2.28575682874977,-24.6610749935103,
12.1522730098206));
#57380=CARTESIAN_POINT('Ctrl Pts',(-2.25209361403474,-24.6591925761609,
12.1564944153469));
#57381=CARTESIAN_POINT('Ctrl Pts',(-2.23526200667722,-24.6582513674861,
12.1586051181101));
#57382=CARTESIAN_POINT('Ctrl Pts',(-2.21819434094244,-24.6573072040779,
12.1607231760983));
#57383=CARTESIAN_POINT('Ctrl Pts',(-2.2008903895958,-24.6563609431785,12.1628466938195));
#57384=CARTESIAN_POINT('Ctrl Pts',(-2.19223841392248,-24.6558878127288,
12.1639084526802));
#57385=CARTESIAN_POINT('Ctrl Pts',(-2.18352736684596,-24.6554141578566,
12.1649715764499));
#57386=CARTESIAN_POINT('Ctrl Pts',(-2.17475722021796,-24.6549400867563,
12.1660358252666));
#57387=CARTESIAN_POINT('Ctrl Pts',(-2.16817961024697,-24.6545845334311,
12.1668340118791));
#57388=CARTESIAN_POINT('Ctrl Pts',(-2.16156875677825,-24.6542287459733,
12.1676328313285));
#57389=CARTESIAN_POINT('Ctrl Pts',(-2.15492464800644,-24.6538727705109,
12.1684321812269));
#57390=CARTESIAN_POINT('Ctrl Pts',(-2.1527099450825,-24.6537541120234,12.168698631193));
#57391=CARTESIAN_POINT('Ctrl Pts',(-2.14918581021379,-24.653565683547,12.169121777238));
#57392=CARTESIAN_POINT('Ctrl Pts',(-2.14826945370353,-24.6535167341359,
12.1692317040438));
#57393=CARTESIAN_POINT('Ctrl Pts',(-2.01266622343075,-24.6462731578717,
12.1854987680001));
#57394=CARTESIAN_POINT('Ctrl Pts',(-1.87302045099594,-24.6395508390581,
12.2006547806672));
#57395=CARTESIAN_POINT('Ctrl Pts',(-1.7293456167262,-24.6334657709698,12.2144316569476));
#57396=CARTESIAN_POINT('Ctrl Pts',(-1.55031236472622,-24.6258831658879,
12.2315990264137));
#57397=CARTESIAN_POINT('Ctrl Pts',(-1.36502203923827,-24.6192903798497,
12.2466257338115));
#57398=CARTESIAN_POINT('Ctrl Pts',(-1.17351855249445,-24.6139000937111,
12.2589747504868));
#57399=CARTESIAN_POINT('Ctrl Pts',(-0.994986211747918,-24.6088749089587,
12.2704873286149));
#57400=CARTESIAN_POINT('Ctrl Pts',(-0.811053939099326,-24.6048949710037,
12.2796723335614));
#57401=CARTESIAN_POINT('Ctrl Pts',(-0.621782179049804,-24.6021357649185,
12.2860623894005));
#57402=CARTESIAN_POINT('Ctrl Pts',(-0.437696294019074,-24.5994521585842,
12.2922773634898));
#57403=CARTESIAN_POINT('Ctrl Pts',(-0.24855786948701,-24.5979230965636,
12.2958478190973));
#57404=CARTESIAN_POINT('Ctrl Pts',(-0.0545118224166704,-24.5977239499185,
12.2963372967855));
#57405=CARTESIAN_POINT('Ctrl Pts',(0.0790731766073289,-24.5975868535705,
12.2966742625598));
#57406=CARTESIAN_POINT('Ctrl Pts',(0.214983132282025,-24.5980801350522,
12.2955506236401));
#57407=CARTESIAN_POINT('Ctrl Pts',(0.35315773706709,-24.5992622024089,12.2928178531011));
#57408=CARTESIAN_POINT('Ctrl Pts',(0.484497401462059,-24.6003857976611,
12.2902202616984));
#57409=CARTESIAN_POINT('Ctrl Pts',(0.617882884816372,-24.6021314640099,
12.2861686774687));
#57410=CARTESIAN_POINT('Ctrl Pts',(0.753271902750463,-24.604568076601,12.2805367715706));
#57411=CARTESIAN_POINT('Ctrl Pts',(0.832469025839653,-24.6059933968392,
12.2772423334289));
#57412=CARTESIAN_POINT('Ctrl Pts',(0.912351596562833,-24.6076552162223,
12.2734070861427));
#57413=CARTESIAN_POINT('Ctrl Pts',(0.992910109818521,-24.6095679523229,
12.2690052580806));
#57414=CARTESIAN_POINT('Ctrl Pts',(1.03318936644636,-24.6105243203733,12.2668043440495));
#57415=CARTESIAN_POINT('Ctrl Pts',(1.0736376087202,-24.6115434212917,12.2644617866549));
#57416=CARTESIAN_POINT('Ctrl Pts',(1.1142535593614,-24.6126271063427,12.2619743229869));
#57417=CARTESIAN_POINT('Ctrl Pts',(1.13456153468199,-24.6131689488682,12.260730591153));
#57418=CARTESIAN_POINT('Ctrl Pts',(1.15491143709519,-24.6137269376663,12.2594506328696));
#57419=CARTESIAN_POINT('Ctrl Pts',(1.17530310430095,-24.6143013063295,12.2581340395361));
#57420=CARTESIAN_POINT('Ctrl Pts',(1.18549893790384,-24.6145884906612,12.2574757428694));
#57421=CARTESIAN_POINT('Ctrl Pts',(1.19570521270492,-24.6148797699744,12.2568082874476));
#57422=CARTESIAN_POINT('Ctrl Pts',(1.20592190810774,-24.6151751736556,12.2561316220514));
#57423=CARTESIAN_POINT('Ctrl Pts',(1.20990015198545,-24.6152901998789,12.2558681376404));
#57424=CARTESIAN_POINT('Ctrl Pts',(1.21387997585457,-24.6154058514412,12.2556032568084));
#57425=CARTESIAN_POINT('Ctrl Pts',(1.21786137849036,-24.6155221300862,12.2553369765201));
#57426=CARTESIAN_POINT('Ctrl Pts',(1.2189923796257,-24.6155551614803,12.2552613340051));
#57427=CARTESIAN_POINT('Ctrl Pts',(1.22012350816173,-24.6155882434778,12.2551855785591));
#57428=CARTESIAN_POINT('Ctrl Pts',(1.2212547640704,-24.6156213761122,12.2551097101167));
#57429=CARTESIAN_POINT('Ctrl Pts',(1.22381154177509,-24.6156962599473,12.254938238091));
#57430=CARTESIAN_POINT('Ctrl Pts',(1.2263689701191,-24.6157714024532,12.2547661888437));
#57431=CARTESIAN_POINT('Ctrl Pts',(1.22892704877899,-24.6158468040031,12.254593561651));
#57432=CARTESIAN_POINT('Ctrl Pts',(1.23148512743888,-24.6159222055531,12.2544209344582));
#57433=CARTESIAN_POINT('Ctrl Pts',(1.23542074363146,-24.6160387093936,12.254154237574));
#57434=CARTESIAN_POINT('Ctrl Pts',(1.23660323538095,-24.6160737861916,12.2540739454465));
#57435=CARTESIAN_POINT('Ctrl Pts',(1.30395072286034,-24.6180715457704,12.2495009976367));
#57436=CARTESIAN_POINT('Ctrl Pts',(1.37844758369426,-24.6204559223908,12.2440559080745));
#57437=CARTESIAN_POINT('Ctrl Pts',(1.46006213674872,-24.6233396542443,12.2374902403641));
#57438=CARTESIAN_POINT('Ctrl Pts',(1.54172913328555,-24.6262252391121,12.2309203537189));
#57439=CARTESIAN_POINT('Ctrl Pts',(1.63052319423837,-24.6296108041441,12.2232283669695));
#57440=CARTESIAN_POINT('Ctrl Pts',(1.72639935501991,-24.6336315012617,12.2141200251773));
#57441=CARTESIAN_POINT('Ctrl Pts',(1.81110721698522,-24.6371838405884,12.2060726841807));
#57442=CARTESIAN_POINT('Ctrl Pts',(1.90134326521786,-24.6412322703028,12.1969190487345));
#57443=CARTESIAN_POINT('Ctrl Pts',(1.99706565552425,-24.6458845705382,12.1864276028006));
#57444=CARTESIAN_POINT('Ctrl Pts',(2.1063522091672,-24.6511961163281,12.1744494860281));
#57445=CARTESIAN_POINT('Ctrl Pts',(2.22279079040698,-24.6572943924893,12.160728092125));
#57446=CARTESIAN_POINT('Ctrl Pts',(2.34629928875798,-24.6643605682681,12.1448817120011));
#57447=CARTESIAN_POINT('Ctrl Pts',(2.46252853931017,-24.6710102832757,12.1299692735021));
#57448=CARTESIAN_POINT('Ctrl Pts',(2.58501895958527,-24.6785173574658,12.1131744638724));
#57449=CARTESIAN_POINT('Ctrl Pts',(2.7136812410372,-24.687051272543,12.0941475403894));
#57450=CARTESIAN_POINT('Ctrl Pts',(2.74250184071604,-24.6889628860117,12.0898854727606));
#57451=CARTESIAN_POINT('Ctrl Pts',(2.77163203546633,-24.6909260947847,12.0855112874804));
#57452=CARTESIAN_POINT('Ctrl Pts',(2.80107067398166,-24.6929429031056,12.0810209004385));
#57453=CARTESIAN_POINT('Ctrl Pts',(2.82649119466277,-24.6946844346511,12.0771434121299));
#57454=CARTESIAN_POINT('Ctrl Pts',(2.85493634185601,-24.6966591221582,12.0727493060695));
#57455=CARTESIAN_POINT('Ctrl Pts',(2.88361400236558,-24.6986826338651,12.0682498311971));
#57456=CARTESIAN_POINT('Ctrl Pts',(2.89878517922108,-24.6997531205585,12.0658695000323));
#57457=CARTESIAN_POINT('Ctrl Pts',(2.91402157098735,-24.7008369188883,12.0634604317022));
#57458=CARTESIAN_POINT('Ctrl Pts',(2.9289108422853,-24.7019042081627,12.0610888880559));
#57459=CARTESIAN_POINT('Ctrl Pts',(3.02425374484228,-24.7087385558787,12.0459027953142));
#57460=CARTESIAN_POINT('Ctrl Pts',(3.11262116651476,-24.7154092679509,12.0311145311352));
#57461=CARTESIAN_POINT('Ctrl Pts',(3.19406216944735,-24.7217849183696,12.0170066694321));
#57462=CARTESIAN_POINT('Ctrl Pts',(3.25118406449557,-24.7262567350341,12.0071115580442));
#57463=CARTESIAN_POINT('Ctrl Pts',(3.30489854444122,-24.7305838293824,11.9975501317833));
#57464=CARTESIAN_POINT('Ctrl Pts',(3.35522197545394,-24.7347269021394,11.9884058881509));
#57465=CARTESIAN_POINT('Ctrl Pts',(3.42777339920782,-24.7406999811044,11.9752226078909));
#57466=CARTESIAN_POINT('Ctrl Pts',(3.49327682573633,-24.7462896487671,11.9629084824941));
#57467=CARTESIAN_POINT('Ctrl Pts',(3.55177749153045,-24.7513962548883,11.9516733020361));
#57468=CARTESIAN_POINT('Ctrl Pts',(3.61056547644036,-24.7565279415028,11.9403829413153));
#57469=CARTESIAN_POINT('Ctrl Pts',(3.662281897611,-24.7611718011313,11.9301820645786));
#57470=CARTESIAN_POINT('Ctrl Pts',(3.70696561522605,-24.765248372565,11.9212359999113));
#57471=CARTESIAN_POINT('Ctrl Pts',(3.75187520563725,-24.7693455507575,11.9122447135671));
#57472=CARTESIAN_POINT('Ctrl Pts',(3.78968093527517,-24.7728696794522,11.9045208998948));
#57473=CARTESIAN_POINT('Ctrl Pts',(3.82041308244611,-24.7757620715134,11.898185551049));
#57474=CARTESIAN_POINT('Ctrl Pts',(3.82688038828348,-24.7763707495846,11.896852333479));
#57475=CARTESIAN_POINT('Ctrl Pts',(3.83303440166048,-24.7769515284611,11.8955804417933));
#57476=CARTESIAN_POINT('Ctrl Pts',(3.83887534622704,-24.7775039851309,11.8943707442518));
#57477=CARTESIAN_POINT('Ctrl Pts',(3.851141932702,-24.7786642011604,11.8918302545531));
#57478=CARTESIAN_POINT('Ctrl Pts',(3.86202777749022,-24.7796994500888,11.889564179342));
#57479=CARTESIAN_POINT('Ctrl Pts',(3.87153463878721,-24.780606438657,11.8875792653162));
#57480=CARTESIAN_POINT('Ctrl Pts',(3.8762880694357,-24.7810599329411,11.8865868083033));
#57481=CARTESIAN_POINT('Ctrl Pts',(3.88069675421204,-24.7814813625433,11.8856646417763));
#57482=CARTESIAN_POINT('Ctrl Pts',(3.88476086456357,-24.7818704094171,11.884813414653));
#57483=CARTESIAN_POINT('Ctrl Pts',(3.88679291973933,-24.782064932854,11.8843878010913));
#57484=CARTESIAN_POINT('Ctrl Pts',(3.88873883130893,-24.7822513606371,11.8839799223937));
#57485=CARTESIAN_POINT('Ctrl Pts',(3.89059861927939,-24.7824296556881,11.8835898543782));
#57486=CARTESIAN_POINT('Ctrl Pts',(3.89152851326463,-24.7825188032136,11.8833948203705));
#57487=CARTESIAN_POINT('Ctrl Pts',(3.89243687635008,-24.7826059175579,11.8832042390341));
#57488=CARTESIAN_POINT('Ctrl Pts',(3.89332371087025,-24.7826909944048,11.8830181191914));
#57489=CARTESIAN_POINT('Ctrl Pts',(3.89376712813033,-24.7827335328282,11.88292505927));
#57490=CARTESIAN_POINT('Ctrl Pts',(3.89420516323368,-24.7827755619058,11.8828331146642));
#57491=CARTESIAN_POINT('Ctrl Pts',(3.89463512744225,-24.7828168226514,11.8827428518383));
#57492=CARTESIAN_POINT('Ctrl Pts',(3.89506509165082,-24.782858083397,11.8826525890124));
#57493=CARTESIAN_POINT('Ctrl Pts',(3.89549238168182,-24.7828990583497,11.8825629473677));
#57494=CARTESIAN_POINT('Ctrl Pts',(3.89721720804704,-24.7830646888322,11.8822006266423));
#57495=CARTESIAN_POINT('Ctrl Pts',(3.90600392129834,-24.7839084535057,11.8803548708123));
#57496=CARTESIAN_POINT('Ctrl Pts',(3.91477185417485,-24.7847533414518,11.8785070705958));
#57497=CARTESIAN_POINT('Ctrl Pts',(3.92352101537525,-24.7855993188514,11.8766573015967));
#57498=CARTESIAN_POINT('Ctrl Pts',(4.08352595353532,-24.8010705804277,11.8428286673394));
#57499=CARTESIAN_POINT('Ctrl Pts',(4.23725160174758,-24.8169049778325,11.8083456468854));
#57500=CARTESIAN_POINT('Ctrl Pts',(4.38475855196937,-24.8329052578264,11.77364883758));
#57501=CARTESIAN_POINT('Ctrl Pts',(4.40472994463671,-24.835071582017,11.7689511362046));
#57502=CARTESIAN_POINT('Ctrl Pts',(4.42458735895512,-24.8372409692867,11.7642494432575));
#57503=CARTESIAN_POINT('Ctrl Pts',(4.44433096146912,-24.8394129509478,11.7595447848344));
#57504=CARTESIAN_POINT('Ctrl Pts',(4.59308062634943,-24.8557768107853,11.7240995633596));
#57505=CARTESIAN_POINT('Ctrl Pts',(4.73536929916207,-24.872286764384,11.6884901115367));
#57506=CARTESIAN_POINT('Ctrl Pts',(4.87127286564285,-24.888754267773,11.6531293828841));
#57507=CARTESIAN_POINT('Ctrl Pts',(4.89543477694101,-24.8916819786969,11.6468426987943));
#57508=CARTESIAN_POINT('Ctrl Pts',(4.91939488858616,-24.8946083844813,11.6405637505741));
#57509=CARTESIAN_POINT('Ctrl Pts',(4.94315365408059,-24.8975324732694,11.6342946976842));
#57510=CARTESIAN_POINT('Ctrl Pts',(5.07994862119384,-24.9143683913517,11.5981996032611));
#57511=CARTESIAN_POINT('Ctrl Pts',(5.21006827964491,-24.9311264234348,11.562436664669));
#57512=CARTESIAN_POINT('Ctrl Pts',(5.33360073781613,-24.9476267914863,11.5273895893518));
#57513=CARTESIAN_POINT('Ctrl Pts',(5.36979448451348,-24.9524612305521,11.5171211547615));
#57514=CARTESIAN_POINT('Ctrl Pts',(5.40542280601805,-24.957273639452,11.5069138426419));
#57515=CARTESIAN_POINT('Ctrl Pts',(5.44048800083792,-24.9620597200354,11.4967765000317));
#57516=CARTESIAN_POINT('Ctrl Pts',(5.56340175383617,-24.9788363308507,11.4612421523103));
#57517=CARTESIAN_POINT('Ctrl Pts',(5.67939602405027,-24.9952885190694,11.4265714871969));
#57518=CARTESIAN_POINT('Ctrl Pts',(5.78856809304377,-25.0112461300498,11.3931131709817));
#57519=CARTESIAN_POINT('Ctrl Pts',(5.84238475164958,-25.0191124763617,11.3766198059857));
#57520=CARTESIAN_POINT('Ctrl Pts',(5.89454365912036,-25.0268588293931,11.3604202503116));
#57521=CARTESIAN_POINT('Ctrl Pts',(5.94505661807441,-25.034465991728,11.344551800168));
#57522=CARTESIAN_POINT('Ctrl Pts',(5.95968428646052,-25.036668892732,11.3399565748772));
#57523=CARTESIAN_POINT('Ctrl Pts',(5.97417392859596,-25.0388601269703,11.3353890972023));
#57524=CARTESIAN_POINT('Ctrl Pts',(5.98852581858791,-25.0410392599716,11.3308502293489));
#57525=CARTESIAN_POINT('Ctrl Pts',(-6.39567215687499,-24.2657748885789,
11.8440001031121));
#57526=CARTESIAN_POINT('Ctrl Pts',(-6.35564925762009,-24.2594187411299,
11.8565901649694));
#57527=CARTESIAN_POINT('Ctrl Pts',(-5.98525024769625,-24.2012639131291,
11.9719907509251));
#57528=CARTESIAN_POINT('Ctrl Pts',(-5.2561684893674,-24.0987569285165,12.1789670347241));
#57529=CARTESIAN_POINT('Ctrl Pts',(-4.17576488270491,-23.9769549473289,
12.4300237910532));
#57530=CARTESIAN_POINT('Ctrl Pts',(-3.01937236748527,-23.8792990190897,
12.6350405053752));
#57531=CARTESIAN_POINT('Ctrl Pts',(-1.83578745066896,-23.813668726209,12.7756187739789));
#57532=CARTESIAN_POINT('Ctrl Pts',(-0.697920992868922,-23.7825581791349,
12.8441383465189));
#57533=CARTESIAN_POINT('Ctrl Pts',(0.331415178970398,-23.7794558007235,
12.8512034394307));
#57534=CARTESIAN_POINT('Ctrl Pts',(1.24581749162491,-23.7959569070388,12.8144567277242));
#57535=CARTESIAN_POINT('Ctrl Pts',(2.07031043589906,-23.8272323667122,12.7465802066477));
#57536=CARTESIAN_POINT('Ctrl Pts',(2.81707948231361,-23.8693935680378,12.6564381575931));
#57537=CARTESIAN_POINT('Ctrl Pts',(3.49019584745524,-23.9189819909321,12.5517016211412));
#57538=CARTESIAN_POINT('Ctrl Pts',(4.09498188363305,-23.9729956946651,12.4387764844399));
#57539=CARTESIAN_POINT('Ctrl Pts',(4.65006137436846,-24.0305553196469,12.3195511568429));
#57540=CARTESIAN_POINT('Ctrl Pts',(5.18050883581102,-24.0928860470317,12.1916386147714));
#57541=CARTESIAN_POINT('Ctrl Pts',(5.70542717899815,-24.161879716131,12.0514948116598));
#57542=CARTESIAN_POINT('Ctrl Pts',(6.10978536005174,-24.2209477044549,11.9329722451569));
#57543=CARTESIAN_POINT('Ctrl Pts',(6.34031713732058,-24.2569838550135,11.8614125115549));
#57544=CARTESIAN_POINT('Ctrl Pts',(6.39541677308294,-24.2657356646736,11.8440802215452));
#57545=CARTESIAN_POINT('Ctrl Pts',(-6.33018760820761,-24.6384834345141,
11.8153028757991));
#57546=CARTESIAN_POINT('Ctrl Pts',(-6.29063887131025,-24.632207888034,11.8278584824185));
#57547=CARTESIAN_POINT('Ctrl Pts',(-5.92460081410956,-24.5747868495937,
11.9429531771344));
#57548=CARTESIAN_POINT('Ctrl Pts',(-5.20363827142956,-24.4735116632754,
12.1495424295994));
#57549=CARTESIAN_POINT('Ctrl Pts',(-4.13466637437114,-24.3531178682958,
12.400332283845));
#57550=CARTESIAN_POINT('Ctrl Pts',(-2.99013371612863,-24.2565650775772,
12.6052500696659));
#57551=CARTESIAN_POINT('Ctrl Pts',(-1.81835067631736,-24.1916608618674,
12.7458212153212));
#57552=CARTESIAN_POINT('Ctrl Pts',(-0.691523858728446,-24.1608836285925,
12.8143591049538));
#57553=CARTESIAN_POINT('Ctrl Pts',(0.328416326781379,-24.1578130063956,
12.8214277182404));
#57554=CARTESIAN_POINT('Ctrl Pts',(1.23411374818715,-24.1741398737994,12.7846682205713));
#57555=CARTESIAN_POINT('Ctrl Pts',(2.05053453853478,-24.2050743152816,12.716783758354));
#57556=CARTESIAN_POINT('Ctrl Pts',(2.78984559896008,-24.2467682391815,12.626650714225));
#57557=CARTESIAN_POINT('Ctrl Pts',(3.45612791133979,-24.2957999436839,12.5219504369033));
#57558=CARTESIAN_POINT('Ctrl Pts',(4.05467909050439,-24.3492003014555,12.4090946277549));
#57559=CARTESIAN_POINT('Ctrl Pts',(4.60394317864352,-24.4060984734748,12.2899771959904));
#57560=CARTESIAN_POINT('Ctrl Pts',(5.12872579761141,-24.467702523329,12.1622226552969));
#57561=CARTESIAN_POINT('Ctrl Pts',(5.64789551167839,-24.5358760477359,12.0223078678906));
#57562=CARTESIAN_POINT('Ctrl Pts',(6.04766431615617,-24.594221541182,11.9040400248831));
#57563=CARTESIAN_POINT('Ctrl Pts',(6.27548853220886,-24.6298039142637,11.8326675985416));
#57564=CARTESIAN_POINT('Ctrl Pts',(6.32993492750253,-24.6384446244456,11.815382831619));
#57565=CARTESIAN_POINT('Ctrl Pts',(-6.21932807476777,-24.9339439082172,
11.604605690097));
#57566=CARTESIAN_POINT('Ctrl Pts',(-6.18048319098318,-24.927839570483,11.6170311210407));
#57567=CARTESIAN_POINT('Ctrl Pts',(-5.82094596454687,-24.8719851686731,
11.7309382763999));
#57568=CARTESIAN_POINT('Ctrl Pts',(-5.11256521760226,-24.7734765152896,
11.935486217029));
#57569=CARTESIAN_POINT('Ctrl Pts',(-4.06220012775385,-24.656438577069,12.183872436982));
#57570=CARTESIAN_POINT('Ctrl Pts',(-2.93773661033481,-24.5626423516593,
12.3868519818438));
#57571=CARTESIAN_POINT('Ctrl Pts',(-1.78661031468882,-24.4996269921563,
12.5261022238268));
#57572=CARTESIAN_POINT('Ctrl Pts',(-0.679624998569868,-24.469749998326,
12.5940022893219));
#57573=CARTESIAN_POINT('Ctrl Pts',(0.322797658949184,-24.4667682564501,
12.6010062443498));
#57574=CARTESIAN_POINT('Ctrl Pts',(1.21266000790277,-24.4826189620022,12.5645869597438));
#57575=CARTESIAN_POINT('Ctrl Pts',(2.01470259299457,-24.5126494340044,12.4973377775454));
#57576=CARTESIAN_POINT('Ctrl Pts',(2.74098505384707,-24.5531332040697,12.4080520697349));
#57577=CARTESIAN_POINT('Ctrl Pts',(3.39555710185985,-24.6007563884208,12.3043401270959));
#57578=CARTESIAN_POINT('Ctrl Pts',(3.98362867469768,-24.6526406766682,12.1925548621677));
#57579=CARTESIAN_POINT('Ctrl Pts',(4.52330902376504,-24.7079423472852,12.0745750879856));
#57580=CARTESIAN_POINT('Ctrl Pts',(5.0389522756289,-24.7678368988428,11.9480529624072));
#57581=CARTESIAN_POINT('Ctrl Pts',(5.54907007392285,-24.8341368734838,11.8095087077752));
#57582=CARTESIAN_POINT('Ctrl Pts',(5.94182116608985,-24.8908896280395,11.6924277333148));
#57583=CARTESIAN_POINT('Ctrl Pts',(6.16560261557379,-24.9255012171011,11.6217903445456));
#57584=CARTESIAN_POINT('Ctrl Pts',(6.21907959854346,-24.9339060769377,11.6046848718899));
#57585=CARTESIAN_POINT('Ctrl Pts',(-6.09477939299971,-25.0678698905147,
11.2722082266352));
#57586=CARTESIAN_POINT('Ctrl Pts',(-6.05666692574621,-25.0619784177097,
11.2844450029348));
#57587=CARTESIAN_POINT('Ctrl Pts',(-5.70391276856255,-25.0080755673627,
11.3966227162906));
#57588=CARTESIAN_POINT('Ctrl Pts',(-5.00898083431377,-24.9130771230655,
11.5980591809797));
#57589=CARTESIAN_POINT('Ctrl Pts',(-3.97907981782851,-24.8003830729569,
11.8425929828331));
#57590=CARTESIAN_POINT('Ctrl Pts',(-2.87715857378435,-24.7102085307339,
12.0423498167333));
#57591=CARTESIAN_POINT('Ctrl Pts',(-1.74963945844598,-24.6497046156879,
12.1793435465576));
#57592=CARTESIAN_POINT('Ctrl Pts',(-0.665625857014882,-24.6210373185601,
12.2461322723438));
#57593=CARTESIAN_POINT('Ctrl Pts',(0.316165362967699,-24.6181761604121,
12.2530219051821));
#57594=CARTESIAN_POINT('Ctrl Pts',(1.18758896401542,-24.6333849650858,12.2171984183309));
#57595=CARTESIAN_POINT('Ctrl Pts',(1.97305721071989,-24.6622070463197,12.1510458485583));
#57596=CARTESIAN_POINT('Ctrl Pts',(2.68446448312266,-24.701083874296,12.0632032212655));
#57597=CARTESIAN_POINT('Ctrl Pts',(3.32579714717992,-24.7468495445224,11.9611487557751));
#57598=CARTESIAN_POINT('Ctrl Pts',(3.90213960567858,-24.796748592875,11.8511288088831));
#57599=CARTESIAN_POINT('Ctrl Pts',(4.43120697430717,-24.849975255363,11.7349908279827));
#57600=CARTESIAN_POINT('Ctrl Pts',(4.93684832779728,-24.9076663275402,11.6104228168409));
#57601=CARTESIAN_POINT('Ctrl Pts',(5.43719781099491,-24.9715750789933,11.473998412235));
#57602=CARTESIAN_POINT('Ctrl Pts',(5.82250829244893,-25.0263202652274,11.3586968561321));
#57603=CARTESIAN_POINT('Ctrl Pts',(6.04206701108784,-25.0597216307159,11.2891319452229));
#57604=CARTESIAN_POINT('Ctrl Pts',(6.09453542110593,-25.0678333230897,11.2722862444664));
#57605=CARTESIAN_POINT('',(6.27159454870745,-24.2690137147412,11.8794923467063));
#57606=CARTESIAN_POINT('Origin',(5.999999949026,-24.1259420052077,10.9277802669262));
#57607=CARTESIAN_POINT('Ctrl Pts',(-6.27159387328071,-24.2690123753742,
11.8794984953283));
#57608=CARTESIAN_POINT('Ctrl Pts',(-6.13239662717945,-24.2474082695837,
11.9224692255698));
#57609=CARTESIAN_POINT('Ctrl Pts',(-5.98564488051794,-24.22550253681,11.9663158871379));
#57610=CARTESIAN_POINT('Ctrl Pts',(-5.83132857677373,-24.2035349707518,
12.010553920225));
#57611=CARTESIAN_POINT('Ctrl Pts',(-5.67907400589207,-24.1818609009202,
12.0542009139703));
#57612=CARTESIAN_POINT('Ctrl Pts',(-5.51945536419364,-24.1601268679718,
12.0982289236256));
#57613=CARTESIAN_POINT('Ctrl Pts',(-5.35247229680066,-24.1385689747149,
12.1421228901419));
#57614=CARTESIAN_POINT('Ctrl Pts',(-5.32566767336653,-24.1351084369502,
12.1491688814623));
#57615=CARTESIAN_POINT('Ctrl Pts',(-5.29867331120474,-24.1316524459909,
12.1562113129512));
#57616=CARTESIAN_POINT('Ctrl Pts',(-5.27148923945306,-24.1282019864977,
12.1632479318689));
#57617=CARTESIAN_POINT('Ctrl Pts',(-5.14595591333737,-24.1122681094553,
12.1957423346728));
#57618=CARTESIAN_POINT('Ctrl Pts',(-5.01637663573241,-24.0964518554399,
12.2281140196681));
#57619=CARTESIAN_POINT('Ctrl Pts',(-4.88275737830249,-24.0808623948862,
12.2601325393302));
#57620=CARTESIAN_POINT('Ctrl Pts',(-4.71106404886683,-24.0608308033472,
12.3012745599501));
#57621=CARTESIAN_POINT('Ctrl Pts',(-4.53269546252188,-24.041172933994,12.3418362502158));
#57622=CARTESIAN_POINT('Ctrl Pts',(-4.34764543253218,-24.0221340484763,
12.3812950907415));
#57623=CARTESIAN_POINT('Ctrl Pts',(-4.29584179753053,-24.0168042277989,
12.3923413541347));
#57624=CARTESIAN_POINT('Ctrl Pts',(-4.24351464833661,-24.0115229877401,
12.4033009024142));
#57625=CARTESIAN_POINT('Ctrl Pts',(-4.19066409785601,-24.0062958742251,
12.4141615963694));
#57626=CARTESIAN_POINT('Ctrl Pts',(-4.14338773419268,-24.0016200682552,
12.4238768048658));
#57627=CARTESIAN_POINT('Ctrl Pts',(-4.09569255318101,-23.9969875734089,
12.4335129069651));
#57628=CARTESIAN_POINT('Ctrl Pts',(-4.04757898340068,-23.9924025346269,
12.4430611439712));
#57629=CARTESIAN_POINT('Ctrl Pts',(-3.90056246597125,-23.9783924240263,
12.472236874615));
#57630=CARTESIAN_POINT('Ctrl Pts',(-3.74963596560522,-23.9648249549461,
12.5005941124992));
#57631=CARTESIAN_POINT('Ctrl Pts',(-3.59479965791586,-23.9518214662445,
12.527874772864));
#57632=CARTESIAN_POINT('Ctrl Pts',(-3.51738150407117,-23.9453197218937,
12.5415151030463));
#57633=CARTESIAN_POINT('Ctrl Pts',(-3.43898588978398,-23.9389590682647,
12.5548860386607));
#57634=CARTESIAN_POINT('Ctrl Pts',(-3.35961278769273,-23.9327552481046,
12.5679537443453));
#57635=CARTESIAN_POINT('Ctrl Pts',(-3.3199262366471,-23.9296533380245,12.5744875971876));
#57636=CARTESIAN_POINT('Ctrl Pts',(-3.27999531125928,-23.9265906345002,
12.5809456267339));
#57637=CARTESIAN_POINT('Ctrl Pts',(-3.23982000755822,-23.923569150133,12.5873234975459));
#57638=CARTESIAN_POINT('Ctrl Pts',(-3.21973235570769,-23.9220584079494,
12.5905124329519));
#57639=CARTESIAN_POINT('Ctrl Pts',(-3.19958360912905,-23.9205579704376,
12.5936813276397));
#57640=CARTESIAN_POINT('Ctrl Pts',(-3.17937376683442,-23.9190680900284,
12.5968296331371));
#57641=CARTESIAN_POINT('Ctrl Pts',(-3.16169015482662,-23.9177644446704,
12.5995844004473));
#57642=CARTESIAN_POINT('Ctrl Pts',(-3.14395976640254,-23.9164688820872,
12.6023234040973));
#57643=CARTESIAN_POINT('Ctrl Pts',(-3.12618260080716,-23.9151815721529,
12.605046273797));
#57644=CARTESIAN_POINT('Ctrl Pts',(-3.1236430057221,-23.9149976707337,12.6054352551827));
#57645=CARTESIAN_POINT('Ctrl Pts',(-3.11986203063022,-23.9147243461149,
12.6060134344833));
#57646=CARTESIAN_POINT('Ctrl Pts',(-3.11856095164605,-23.9146303736825,
12.6062122290604));
#57647=CARTESIAN_POINT('Ctrl Pts',(-3.09161417126445,-23.9126841009898,
12.6103294839506));
#57648=CARTESIAN_POINT('Ctrl Pts',(-3.0634423340961,-23.9106768776393,12.6145803991693));
#57649=CARTESIAN_POINT('Ctrl Pts',(-3.0340454669724,-23.9086159226008,12.6189497247918));
#57650=CARTESIAN_POINT('Ctrl Pts',(-2.96197963940193,-23.9035635328408,
12.6296610385376));
#57651=CARTESIAN_POINT('Ctrl Pts',(-2.88255172211161,-23.8981867199339,
12.6410872436616));
#57652=CARTESIAN_POINT('Ctrl Pts',(-2.79576134945282,-23.8926070410898,
12.6529712009058));
#57653=CARTESIAN_POINT('Ctrl Pts',(-2.70930123057302,-23.8870485939787,
12.6648099374455));
#57654=CARTESIAN_POINT('Ctrl Pts',(-2.61553433409856,-23.8812888577212,
12.6771029777179));
#57655=CARTESIAN_POINT('Ctrl Pts',(-2.51446139230001,-23.875469340143,12.6895489825356));
#57656=CARTESIAN_POINT('Ctrl Pts',(-2.50259873636493,-23.8747863192127,
12.6910097362278));
#57657=CARTESIAN_POINT('Ctrl Pts',(-2.49063544288681,-23.8741024986736,
12.6924725431445));
#57658=CARTESIAN_POINT('Ctrl Pts',(-2.47857151659949,-23.8734181263219,
12.6939368729798));
#57659=CARTESIAN_POINT('Ctrl Pts',(-2.37688570196303,-23.8676496096352,
12.7062795853488));
#57660=CARTESIAN_POINT('Ctrl Pts',(-2.26804989959386,-23.8618405802166,
12.7187343033419));
#57661=CARTESIAN_POINT('Ctrl Pts',(-2.15206290281673,-23.8561525055082,
12.7309579405412));
#57662=CARTESIAN_POINT('Ctrl Pts',(-2.11969744814923,-23.8545652834123,
12.7343688709613));
#57663=CARTESIAN_POINT('Ctrl Pts',(-2.08677520819492,-23.8529876000154,
12.7377615251891));
#57664=CARTESIAN_POINT('Ctrl Pts',(-2.05329627690419,-23.8514232428241,
12.7411277870223));
#57665=CARTESIAN_POINT('Ctrl Pts',(-1.97656814841425,-23.8478379969708,
12.7488426978787));
#57666=CARTESIAN_POINT('Ctrl Pts',(-1.89691554236842,-23.8443225623912,
12.7564195700191));
#57667=CARTESIAN_POINT('Ctrl Pts',(-1.81433841354751,-23.840925217303,12.7637550184601));
#57668=CARTESIAN_POINT('Ctrl Pts',(-1.81240189321798,-23.8408455459954,
12.7639270424241));
#57669=CARTESIAN_POINT('Ctrl Pts',(-1.81046376456493,-23.8407659396075,
12.7640989332609));
#57670=CARTESIAN_POINT('Ctrl Pts',(-1.80852402756924,-23.8406863988239,
12.7642706895808));
#57671=CARTESIAN_POINT('Ctrl Pts',(-1.76910661759122,-23.8390700499663,
12.7677609510392));
#57672=CARTESIAN_POINT('Ctrl Pts',(-1.72902504057366,-23.8374807808731,
12.7711956978237));
#57673=CARTESIAN_POINT('Ctrl Pts',(-1.68827931980546,-23.8359241930247,
12.7745632605405));
#57674=CARTESIAN_POINT('Ctrl Pts',(-1.6669039077312,-23.8351075991331,12.7763299010466));
#57675=CARTESIAN_POINT('Ctrl Pts',(-1.64534571527873,-23.8342999985571,
12.7780780457792));
#57676=CARTESIAN_POINT('Ctrl Pts',(-1.6236047433072,-23.8335022087906,12.7798059678567));
#57677=CARTESIAN_POINT('Ctrl Pts',(-1.61273425732144,-23.8331033139073,
12.7806699288955));
#57678=CARTESIAN_POINT('Ctrl Pts',(-1.60181807642095,-23.8327068716801,
12.7815288338303));
#57679=CARTESIAN_POINT('Ctrl Pts',(-1.59085620070828,-23.8323129856556,
12.7823824639616));
#57680=CARTESIAN_POINT('Ctrl Pts',(-1.58537526285195,-23.8321160426433,
12.7828092790273));
#57681=CARTESIAN_POINT('Ctrl Pts',(-1.5798829012904,-23.8319197386788,12.7832347753643));
#57682=CARTESIAN_POINT('Ctrl Pts',(-1.57437911603661,-23.8317240867953,
12.7836589254565));
#57683=CARTESIAN_POINT('Ctrl Pts',(-1.56887533078281,-23.8315284349118,
12.7840830755486));
#57684=CARTESIAN_POINT('Ctrl Pts',(-1.56205960344969,-23.8312877045765,
12.7846050496261));
#57685=CARTESIAN_POINT('Ctrl Pts',(-1.55783348920669,-23.8311391004417,
12.7849273093667));
#57686=CARTESIAN_POINT('Ctrl Pts',(-1.33210031965717,-23.8232015766445,
12.8021404532776));
#57687=CARTESIAN_POINT('Ctrl Pts',(-1.11005377605612,-23.8171220368827,
12.8153351581337));
#57688=CARTESIAN_POINT('Ctrl Pts',(-0.891696916844576,-23.8127291071686,
12.8248709177998));
#57689=CARTESIAN_POINT('Ctrl Pts',(-0.848420688569367,-23.8118584707719,
12.8267608136042));
#57690=CARTESIAN_POINT('Ctrl Pts',(-0.805289283440663,-23.8110541627737,
12.8285068905267));
#57691=CARTESIAN_POINT('Ctrl Pts',(-0.762302573188932,-23.8103149647013,
12.8301118032893));
#57692=CARTESIAN_POINT('Ctrl Pts',(-0.724715167136212,-23.8096686128884,
12.8315151325353));
#57693=CARTESIAN_POINT('Ctrl Pts',(-0.687238375249081,-23.8090720098778,
12.8328105347313));
#57694=CARTESIAN_POINT('Ctrl Pts',(-0.649872395356749,-23.8085242237602,
12.8339997614218));
#57695=CARTESIAN_POINT('Ctrl Pts',(-0.558062474711744,-23.8071782882292,
12.8369217457616));
#57696=CARTESIAN_POINT('Ctrl Pts',(-0.466921580641413,-23.8061270274871,
12.8392028078876));
#57697=CARTESIAN_POINT('Ctrl Pts',(-0.376448947681508,-23.8053581703231,
12.8408704270691));
#57698=CARTESIAN_POINT('Ctrl Pts',(-0.312801774508532,-23.8048172820626,
12.8420435911891));
#57699=CARTESIAN_POINT('Ctrl Pts',(-0.249485488676972,-23.8044160906664,
12.8429131418859));
#57700=CARTESIAN_POINT('Ctrl Pts',(-0.186500090506563,-23.8041502798702,
12.8434883989328));
#57701=CARTESIAN_POINT('Ctrl Pts',(-0.155007391421359,-23.8040173744721,
12.8437760274562));
#57702=CARTESIAN_POINT('Ctrl Pts',(-0.123597414128386,-23.8039183139151,
12.8439900795266));
#57703=CARTESIAN_POINT('Ctrl Pts',(-0.0922701582487795,-23.8038525597042,
12.844131701988));
#57704=CARTESIAN_POINT('Ctrl Pts',(-0.0647192913967876,-23.8037947319289,
12.8442562523664));
#57705=CARTESIAN_POINT('Ctrl Pts',(-0.038338200399373,-23.8037631769384,
12.8443236937221));
#57706=CARTESIAN_POINT('Ctrl Pts',(-0.0102093966637263,-23.8037560884165,
12.8443378682552));
#57707=CARTESIAN_POINT('Ctrl Pts',(-0.0063537900014073,-23.8037551167949,
12.8443398111542));
#57708=CARTESIAN_POINT('Ctrl Pts',(-0.00246534702685521,-23.8037546375739,
12.8443406806357));
#57709=CARTESIAN_POINT('Ctrl Pts',(0.00146344560311196,-23.8037546780383,
12.8443404156627));
#57710=CARTESIAN_POINT('Ctrl Pts',(0.123999816234775,-23.8037559400956,
12.8443321513353));
#57711=CARTESIAN_POINT('Ctrl Pts',(0.246532789977683,-23.8042792177409,
12.843219982003));
#57712=CARTESIAN_POINT('Ctrl Pts',(0.369067470033404,-23.8053128677452,
12.841003900385));
#57713=CARTESIAN_POINT('Ctrl Pts',(0.644882197439504,-23.8076395224852,
12.8360156966607));
#57714=CARTESIAN_POINT('Ctrl Pts',(0.920705383073052,-23.8125504903585,
12.8254375262026));
#57715=CARTESIAN_POINT('Ctrl Pts',(1.19652643908533,-23.8200738774936,12.8092721265147));
#57716=CARTESIAN_POINT('Ctrl Pts',(1.22212487701974,-23.8207721090261,12.8077718459104));
#57717=CARTESIAN_POINT('Ctrl Pts',(1.24772329839335,-23.8214928587271,12.8062234073577));
#57718=CARTESIAN_POINT('Ctrl Pts',(1.27332169550815,-23.82223615935,12.8046267927066));
#57719=CARTESIAN_POINT('Ctrl Pts',(1.37083378686327,-23.825067617817,12.7985448012044));
#57720=CARTESIAN_POINT('Ctrl Pts',(1.46834552751173,-23.8282262803923,12.7917637905529));
#57721=CARTESIAN_POINT('Ctrl Pts',(1.56585687062987,-23.8317101409852,12.7842847834704));
#57722=CARTESIAN_POINT('Ctrl Pts',(1.74018381696187,-23.8379384500126,12.7709141085869));
#57723=CARTESIAN_POINT('Ctrl Pts',(1.91451114826108,-23.8452074329911,12.7553127104155));
#57724=CARTESIAN_POINT('Ctrl Pts',(2.08883802674333,-23.8535168166396,12.7374798377617));
#57725=CARTESIAN_POINT('Ctrl Pts',(2.17524324653907,-23.8576353675296,12.728640963948));
#57726=CARTESIAN_POINT('Ctrl Pts',(2.26164833787826,-23.8620095716639,12.7192537731417));
#57727=CARTESIAN_POINT('Ctrl Pts',(2.34805359177696,-23.8666392626977,12.7093187483884));
#57728=CARTESIAN_POINT('Ctrl Pts',(2.47841969236965,-23.8736244255182,12.6943290298475));
#57729=CARTESIAN_POINT('Ctrl Pts',(2.60878583208634,-23.8811913884664,12.6780923256736));
#57730=CARTESIAN_POINT('Ctrl Pts',(2.73915198362006,-23.8893399953416,12.660608688594));
#57731=CARTESIAN_POINT('Ctrl Pts',(2.7725502745386,-23.8914275735955,12.6561295842358));
#57732=CARTESIAN_POINT('Ctrl Pts',(2.80594857215928,-23.8935533167625,12.6515686306175));
#57733=CARTESIAN_POINT('Ctrl Pts',(2.83934685804531,-23.8957172371731,12.6469258080376));
#57734=CARTESIAN_POINT('Ctrl Pts',(2.87113163810424,-23.8977766163445,12.6425072850314));
#57735=CARTESIAN_POINT('Ctrl Pts',(2.90291640750853,-23.8998705731464,12.6380146122504));
#57736=CARTESIAN_POINT('Ctrl Pts',(2.93470118226597,-23.9019990913401,12.6334478151434));
#57737=CARTESIAN_POINT('Ctrl Pts',(2.98358847357062,-23.9052729068628,12.6264237496215));
#57738=CARTESIAN_POINT('Ctrl Pts',(3.03247576140564,-23.9086285029917,12.6192243322693));
#57739=CARTESIAN_POINT('Ctrl Pts',(3.08136305166664,-23.9120658769088,12.6118496265356));
#57740=CARTESIAN_POINT('Ctrl Pts',(3.09765881508698,-23.9132116682146,12.609391391291));
#57741=CARTESIAN_POINT('Ctrl Pts',(3.11203760514041,-23.9142296214825,12.6072074391805));
#57742=CARTESIAN_POINT('Ctrl Pts',(3.13025034275502,-23.9155305097556,12.6044164919562));
#57743=CARTESIAN_POINT('Ctrl Pts',(3.25877662891664,-23.9247108066441,12.5847209311238));
#57744=CARTESIAN_POINT('Ctrl Pts',(3.38588318064259,-23.9344233066419,12.5640238714892));
#57745=CARTESIAN_POINT('Ctrl Pts',(3.51155623328943,-23.9446289514687,12.5424066115913));
#57746=CARTESIAN_POINT('Ctrl Pts',(3.71381534700374,-23.9610539895661,12.5076156382218));
#57747=CARTESIAN_POINT('Ctrl Pts',(3.9123606482021,-23.9787560995128,12.4704422691085));
#57748=CARTESIAN_POINT('Ctrl Pts',(4.10715837540687,-23.9975763260287,12.4312175040207));
#57749=CARTESIAN_POINT('Ctrl Pts',(4.29250871339822,-24.0154838005966,12.3938950795192));
#57750=CARTESIAN_POINT('Ctrl Pts',(4.4744664469351,-24.0344036515817,12.3547152777956));
#57751=CARTESIAN_POINT('Ctrl Pts',(4.65302175618388,-24.0542061396187,12.313950313393));
#57752=CARTESIAN_POINT('Ctrl Pts',(4.83066123702135,-24.0739070586727,12.2733944366549));
#57753=CARTESIAN_POINT('Ctrl Pts',(5.0049332557109,-24.0944816891167,12.2312695841911));
#57754=CARTESIAN_POINT('Ctrl Pts',(5.17584377090454,-24.1158122573969,12.1878294987181));
#57755=CARTESIAN_POINT('Ctrl Pts',(5.35321544777451,-24.1379492140385,12.1427471888614));
#57756=CARTESIAN_POINT('Ctrl Pts',(5.52696673869725,-24.1609005245582,12.0962483800698));
#57757=CARTESIAN_POINT('Ctrl Pts',(5.69711918676627,-24.1845490788121,12.0485987285614));
#57758=CARTESIAN_POINT('Ctrl Pts',(5.87745056229334,-24.2096123462892,11.998098560639));
#57759=CARTESIAN_POINT('Ctrl Pts',(6.05373965431679,-24.235459144335,11.9463058423981));
#57760=CARTESIAN_POINT('Ctrl Pts',(6.22602530087827,-24.2619717767003,11.8935134849131));
#57761=CARTESIAN_POINT('Ctrl Pts',(6.24124677966984,-24.2643141742204,11.8888492672847));
#57762=CARTESIAN_POINT('Ctrl Pts',(6.25643701466579,-24.2666617667428,11.8841772329832));
#57763=CARTESIAN_POINT('Ctrl Pts',(6.27159604017702,-24.2690144967309,11.8794975712369));
#57764=CARTESIAN_POINT('Origin',(5.999999999061,-24.1259421376201,10.9277802195584));
#57765=CARTESIAN_POINT('Origin',(5.99996968604825,-24.1259230378211,10.9277552844787));
#57766=CARTESIAN_POINT('Ctrl Pts',(6.24176941899738,-13.957654817887,8.44269195219273));
#57767=CARTESIAN_POINT('Ctrl Pts',(6.29480662257667,-13.9539758868461,8.42029737038065));
#57768=CARTESIAN_POINT('Ctrl Pts',(6.43873776769985,-13.9497948794457,8.34843305972531));
#57769=CARTESIAN_POINT('Ctrl Pts',(6.65746053635757,-13.9704924485183,8.18719582107129));
#57770=CARTESIAN_POINT('Ctrl Pts',(6.86734070108195,-14.0338129508464,7.94766158322873));
#57771=CARTESIAN_POINT('Ctrl Pts',(7.01531431986487,-14.12893286126,7.67885700588408));
#57772=CARTESIAN_POINT('Ctrl Pts',(7.09527319749003,-14.2420002632323,7.41047463185613));
#57773=CARTESIAN_POINT('Ctrl Pts',(7.10994675708914,-14.3254890997433,7.23571490121343));
#57774=CARTESIAN_POINT('Ctrl Pts',(7.10820126656667,-14.3668778615597,7.15390513393751));
#57775=CARTESIAN_POINT('Ctrl Pts',(7.10813647714078,-14.3682028206859,7.15129096938794));
#57776=CARTESIAN_POINT('Ctrl Pts',(6.04288613265708,-13.4963640462423,8.03309250552645));
#57777=CARTESIAN_POINT('Ctrl Pts',(6.08960516161976,-13.4928601309614,8.01356864824412));
#57778=CARTESIAN_POINT('Ctrl Pts',(6.2166906694153,-13.4882574395743,7.95084472145826));
#57779=CARTESIAN_POINT('Ctrl Pts',(6.41097422058303,-13.5044523004311,7.80952772694627));
#57780=CARTESIAN_POINT('Ctrl Pts',(6.59849710701976,-13.5579129738396,7.59861108001617));
#57781=CARTESIAN_POINT('Ctrl Pts',(6.73122626769599,-13.6400563468318,7.36127071899955));
#57782=CARTESIAN_POINT('Ctrl Pts',(6.80304010187831,-13.7388311824901,7.12425047056187));
#57783=CARTESIAN_POINT('Ctrl Pts',(6.81617738657188,-13.8121459300844,6.9703554643886));
#57784=CARTESIAN_POINT('Ctrl Pts',(6.81461542349125,-13.8484941084794,6.89855976198674));
#57785=CARTESIAN_POINT('Ctrl Pts',(6.81455744755899,-13.8496577047512,6.89626585280356));
#57786=CARTESIAN_POINT('Ctrl Pts',(6.02645468922222,-12.8504950003107,8.09088772242199));
#57787=CARTESIAN_POINT('Ctrl Pts',(6.09090484391799,-12.8459131881969,8.06435034383859));
#57788=CARTESIAN_POINT('Ctrl Pts',(6.26494844742361,-12.8404855791265,7.97971703923798));
#57789=CARTESIAN_POINT('Ctrl Pts',(6.52611211563489,-12.8641139638988,7.79272678876749));
#57790=CARTESIAN_POINT('Ctrl Pts',(6.77358744402654,-12.9364281019538,7.51909413889916));
#57791=CARTESIAN_POINT('Ctrl Pts',(6.9465841611291,-13.0441857127227,7.21504636510149));
#57792=CARTESIAN_POINT('Ctrl Pts',(7.03980001104882,-13.1717068625044,6.91269989963593));
#57793=CARTESIAN_POINT('Ctrl Pts',(7.05702528395121,-13.266031894225,6.71530137399919));
#57794=CARTESIAN_POINT('Ctrl Pts',(7.05497402265406,-13.3130233822045,6.62240791160254));
#57795=CARTESIAN_POINT('Ctrl Pts',(7.05489787988465,-13.3145279375336,6.61943905343894));
#57796=CARTESIAN_POINT('Ctrl Pts',(6.20434282365839,-12.4603649383441,8.57827987685632));
#57797=CARTESIAN_POINT('Ctrl Pts',(6.2985528389579,-12.4541838053812,8.53959812679702));
#57798=CARTESIAN_POINT('Ctrl Pts',(6.55152409727625,-12.4480898317399,8.41685409211037));
#57799=CARTESIAN_POINT('Ctrl Pts',(6.9255489507725,-12.4860551148184,8.14954765545105));
#57800=CARTESIAN_POINT('Ctrl Pts',(7.2746460694698,-12.5931657472206,7.76436053208526));
#57801=CARTESIAN_POINT('Ctrl Pts',(7.51612672467238,-12.747777253834,7.34062969290588));
#57802=CARTESIAN_POINT('Ctrl Pts',(7.64578430161563,-12.9276098455488,6.92052689466441));
#57803=CARTESIAN_POINT('Ctrl Pts',(7.6699507152677,-13.0598954694388,6.64473012363261));
#57804=CARTESIAN_POINT('Ctrl Pts',(7.66706901025419,-13.1260031184009,6.51392112449348));
#57805=CARTESIAN_POINT('Ctrl Pts',(7.66696203505706,-13.1281199481508,6.50973940142776));
#57806=CARTESIAN_POINT('',(6.9999997358385,-13.9487123452115,6.97710990117158));
#57807=CARTESIAN_POINT('',(7.00000022915234,-12.52206486378,8.04447615962587));
#57808=CARTESIAN_POINT('Ctrl Pts',(7.,-13.9487123452086,6.97710990118712));
#57809=CARTESIAN_POINT('Ctrl Pts',(7.,-13.8452746480186,7.02168653880504));
#57810=CARTESIAN_POINT('Ctrl Pts',(7.,-13.7540053535313,7.06360287625015));
#57811=CARTESIAN_POINT('Ctrl Pts',(7.,-13.6763761579061,7.10177115731546));
#57812=CARTESIAN_POINT('Ctrl Pts',(7.,-13.6375615600935,7.12085529784811));
#57813=CARTESIAN_POINT('Ctrl Pts',(7.,-13.6021311738989,7.13895532994855));
#57814=CARTESIAN_POINT('Ctrl Pts',(7.,-13.5701291793535,7.15576042707438));
#57815=CARTESIAN_POINT('Ctrl Pts',(7.,-13.5541281820809,7.16416297563729));
#57816=CARTESIAN_POINT('Ctrl Pts',(7.,-13.5389831154623,7.17224067284011));
#57817=CARTESIAN_POINT('Ctrl Pts',(7.,-13.5246936731342,7.17995082951218));
#57818=CARTESIAN_POINT('Ctrl Pts',(7.,-13.5175489519701,7.18380590784822));
#57819=CARTESIAN_POINT('Ctrl Pts',(7.,-13.5106181368786,7.18756910105157));
#57820=CARTESIAN_POINT('Ctrl Pts',(7.,-13.5039008551055,7.19123504735637));
#57821=CARTESIAN_POINT('Ctrl Pts',(7.,-13.500542214219,7.19306802050878));
#57822=CARTESIAN_POINT('Ctrl Pts',(7.,-13.497236956662,7.19487668193654));
#57823=CARTESIAN_POINT('Ctrl Pts',(7.,-13.4939850306347,7.19666037209525));
#57824=CARTESIAN_POINT('Ctrl Pts',(7.,-13.4907331046074,7.19844406225396));
#57825=CARTESIAN_POINT('Ctrl Pts',(7.,-13.4891059090995,7.19933693116375));
#57826=CARTESIAN_POINT('Ctrl Pts',(7.,-13.4843891909902,7.20193587147612));
#57827=CARTESIAN_POINT('Ctrl Pts',(7.,-13.4089217012407,7.24351891647397));
#57828=CARTESIAN_POINT('Ctrl Pts',(7.,-13.3377088629193,7.28578459273304));
#57829=CARTESIAN_POINT('Ctrl Pts',(7.,-13.2712546130133,7.32835053042459));
#57830=CARTESIAN_POINT('Ctrl Pts',(7.,-13.2048003631073,7.37091646811614));
#57831=CARTESIAN_POINT('Ctrl Pts',(7.,-13.1443230524494,7.41286004032249));
#57832=CARTESIAN_POINT('Ctrl Pts',(7.,-13.0863568342088,7.45600927554525));
#57833=CARTESIAN_POINT('Ctrl Pts',(7.,-12.9704243977276,7.54230774599077));
#57834=CARTESIAN_POINT('Ctrl Pts',(7.,-12.8624865195397,7.63585224400371));
#57835=CARTESIAN_POINT('Ctrl Pts',(7.,-12.7672168886966,7.73520351279626));
#57836=CARTESIAN_POINT('Ctrl Pts',(7.,-12.6719472578536,7.83455478158881));
#57837=CARTESIAN_POINT('Ctrl Pts',(7.,-12.5894810216966,7.93953249757783));
#57838=CARTESIAN_POINT('Ctrl Pts',(7.,-12.5220651723765,8.04447541337249));
#57839=CARTESIAN_POINT('',(6.24994411212243,-12.4626497324863,8.55169576993692));
#57840=CARTESIAN_POINT('Ctrl Pts',(6.24994458392592,-12.4626510779178,8.55169669313912));
#57841=CARTESIAN_POINT('Ctrl Pts',(6.29980713482775,-12.4600704144922,8.52997497958608));
#57842=CARTESIAN_POINT('Ctrl Pts',(6.34865158794145,-12.4586352046275,8.50672736958435));
#57843=CARTESIAN_POINT('Ctrl Pts',(6.39650052995822,-12.4582919652257,8.48202083011274));
#57844=CARTESIAN_POINT('Ctrl Pts',(6.42315482381289,-12.458100763425,8.46825803128267));
#57845=CARTESIAN_POINT('Ctrl Pts',(6.44950004849653,-12.4582489082855,8.45404171252757));
#57846=CARTESIAN_POINT('Ctrl Pts',(6.47553829213457,-12.4587308389966,8.43937781738155));
#57847=CARTESIAN_POINT('Ctrl Pts',(6.52301980353868,-12.4596096539763,8.41263776861777));
#57848=CARTESIAN_POINT('Ctrl Pts',(6.56948206886044,-12.4615968089396,8.38441151778665));
#57849=CARTESIAN_POINT('Ctrl Pts',(6.61495853931863,-12.4646596198119,8.35471776067509));
#57850=CARTESIAN_POINT('Ctrl Pts',(6.62617140476325,-12.4654147990474,8.34739634589328));
#57851=CARTESIAN_POINT('Ctrl Pts',(6.63732421927012,-12.4662355009643,8.33998554122602));
#57852=CARTESIAN_POINT('Ctrl Pts',(6.64841723331421,-12.467121485517,8.33248529664793));
#57853=CARTESIAN_POINT('Ctrl Pts',(6.69398634271207,-12.4707610308061,8.301674962835));
#57854=CARTESIAN_POINT('Ctrl Pts',(6.73853003492269,-12.4755031700154,8.26936384606336));
#57855=CARTESIAN_POINT('Ctrl Pts',(6.78203915041949,-12.4813450910741,8.23553650332579));
#57856=CARTESIAN_POINT('Ctrl Pts',(6.82408117528156,-12.4869900274878,8.20284979002096));
#57857=CARTESIAN_POINT('Ctrl Pts',(6.86515751416727,-12.4936620603136,8.16874687499731));
#57858=CARTESIAN_POINT('Ctrl Pts',(6.90522598975078,-12.5013798136185,8.13319060703869));
#57859=CARTESIAN_POINT('Ctrl Pts',(6.93747899993367,-12.5075921981004,8.10456968608188));
#57860=CARTESIAN_POINT('Ctrl Pts',(6.96907832789861,-12.514482605464,8.07500655154155));
#57861=CARTESIAN_POINT('Ctrl Pts',(7.0000006857802,-12.5220636286664,8.04447631542505));
#57862=CARTESIAN_POINT('',(6.26385800258875,-13.9442712228614,8.42072567770104));
#57863=CARTESIAN_POINT('Origin',(6.52767709685874,-13.2547595885169,9.09522362637851));
#57864=CARTESIAN_POINT('Ctrl Pts',(6.26385556499199,-13.9442775931717,8.42071944622816));
#57865=CARTESIAN_POINT('Ctrl Pts',(6.30364986918725,-13.9340686569687,8.3947165152949));
#57866=CARTESIAN_POINT('Ctrl Pts',(6.34303408262301,-13.9248559416285,8.36600596164334));
#57867=CARTESIAN_POINT('Ctrl Pts',(6.38165189810817,-13.916706545455,8.33460109009556));
#57868=CARTESIAN_POINT('Ctrl Pts',(6.42679322248454,-13.9071805137124,8.29789115516716));
#57869=CARTESIAN_POINT('Ctrl Pts',(6.47088804817601,-13.8991074859413,8.25749861371456));
#57870=CARTESIAN_POINT('Ctrl Pts',(6.5134097964521,-13.8925137453288,8.21357735272315));
#57871=CARTESIAN_POINT('Ctrl Pts',(6.53319105122902,-13.8894463158774,8.19314504010624));
#57872=CARTESIAN_POINT('Ctrl Pts',(6.55263123592839,-13.8866991949207,8.17194929236314));
#57873=CARTESIAN_POINT('Ctrl Pts',(6.57167372767561,-13.8842762175336,8.15000655423389));
#57874=CARTESIAN_POINT('Ctrl Pts',(6.58329061004541,-13.8827980788707,8.13662037499314));
#57875=CARTESIAN_POINT('Ctrl Pts',(6.59475945253126,-13.881440596437,8.12295619689224));
#57876=CARTESIAN_POINT('Ctrl Pts',(6.60606692691309,-13.8802048332916,8.1090178202598));
#57877=CARTESIAN_POINT('Ctrl Pts',(6.64408883391461,-13.8760495224057,8.0621493824305));
#57878=CARTESIAN_POINT('Ctrl Pts',(6.68028935710774,-13.8732694357406,8.01217942416458));
#57879=CARTESIAN_POINT('Ctrl Pts',(6.71423356137519,-13.8718345738079,7.95935553048294));
#57880=CARTESIAN_POINT('Ctrl Pts',(6.73210548380837,-13.871079106366,7.93154328533327));
#57881=CARTESIAN_POINT('Ctrl Pts',(6.74935123905505,-13.8706967808737,7.90294015228878));
#57882=CARTESIAN_POINT('Ctrl Pts',(6.76590192403628,-13.8706852165941,7.87358370287777));
#57883=CARTESIAN_POINT('Ctrl Pts',(6.77350230243503,-13.8706799060647,7.86010268235081));
#57884=CARTESIAN_POINT('Ctrl Pts',(6.7809560457977,-13.8707528051892,7.84646281264733));
#57885=CARTESIAN_POINT('Ctrl Pts',(6.78825616054251,-13.870903806069,7.8326677959974));
#57886=CARTESIAN_POINT('Ctrl Pts',(6.79013419613901,-13.8709426527224,7.82911887475046));
#57887=CARTESIAN_POINT('Ctrl Pts',(6.79200206297191,-13.8709866688481,7.82555968552902));
#57888=CARTESIAN_POINT('Ctrl Pts',(6.79385967091336,-13.8710358344652,7.82199031382253));
#57889=CARTESIAN_POINT('Ctrl Pts',(6.7983988300735,-13.8711559731425,7.81326837313962));
#57890=CARTESIAN_POINT('Ctrl Pts',(6.80287674779809,-13.8713068589087,7.80448560945556));
#57891=CARTESIAN_POINT('Ctrl Pts',(6.80729207758989,-13.871488207311,7.79564330332061));
#57892=CARTESIAN_POINT('Ctrl Pts',(6.80949974248579,-13.8715788815121,7.79122215025313));
#57893=CARTESIAN_POINT('Ctrl Pts',(6.81169175993162,-13.8716771712627,7.78678611169662));
#57894=CARTESIAN_POINT('Ctrl Pts',(6.8138679617779,-13.8717830418694,7.7823353433877));
#57895=CARTESIAN_POINT('Ctrl Pts',(6.81548499128459,-13.8718617091563,7.77902819442299));
#57896=CARTESIAN_POINT('Ctrl Pts',(6.81751780310369,-13.8719669126278,7.77483363831133));
#57897=CARTESIAN_POINT('Ctrl Pts',(6.81901903974428,-13.8720493090388,7.7717112155293));
#57898=CARTESIAN_POINT('Ctrl Pts',(6.81953817065756,-13.8720778018979,7.77063147490302));
#57899=CARTESIAN_POINT('Ctrl Pts',(6.81999417830938,-13.8721033441437,7.76968019404295));
#57900=CARTESIAN_POINT('Ctrl Pts',(6.82034895003808,-13.8721233622159,7.76893900667714));
#57901=CARTESIAN_POINT('Ctrl Pts',(6.83460306900321,-13.8729276539882,7.73915937083463));
#57902=CARTESIAN_POINT('Ctrl Pts',(6.84880155763395,-13.874076872251,7.70735440476999));
#57903=CARTESIAN_POINT('Ctrl Pts',(6.86266124201387,-13.8756671067256,7.67346133410921));
#57904=CARTESIAN_POINT('Ctrl Pts',(6.87577619130936,-13.8771718916782,7.64138947078245));
#57905=CARTESIAN_POINT('Ctrl Pts',(6.88858789184152,-13.879071573022,7.60744770501848));
#57906=CARTESIAN_POINT('Ctrl Pts',(6.90081551644704,-13.8814491338862,7.57160537737455));
#57907=CARTESIAN_POINT('Ctrl Pts',(6.90556286907159,-13.8823722174918,7.5576896599969));
#57908=CARTESIAN_POINT('Ctrl Pts',(6.91022171578473,-13.8833673525982,7.54348772154589));
#57909=CARTESIAN_POINT('Ctrl Pts',(6.91477373911994,-13.8844394701365,7.52899884039857));
#57910=CARTESIAN_POINT('Ctrl Pts',(6.92451243856034,-13.8867331821194,7.49800100749425));
#57911=CARTESIAN_POINT('Ctrl Pts',(6.93376338705338,-13.8893794429974,7.46568845724205));
#57912=CARTESIAN_POINT('Ctrl Pts',(6.9423487824454,-13.8924173078754,7.43207739625192));
#57913=CARTESIAN_POINT('Ctrl Pts',(6.95179578557956,-13.8957600448972,7.39509321742059));
#57914=CARTESIAN_POINT('Ctrl Pts',(6.96043782096829,-13.8995769584793,7.35653610866358));
#57915=CARTESIAN_POINT('Ctrl Pts',(6.96800709073418,-13.9039173172265,7.3164568676453));
#57916=CARTESIAN_POINT('Ctrl Pts',(6.97344669462717,-13.9070364863232,7.28765419549672));
#57917=CARTESIAN_POINT('Ctrl Pts',(6.97833164672333,-13.9104259232775,7.25806603815568));
#57918=CARTESIAN_POINT('Ctrl Pts',(6.98254998067605,-13.9141031142514,7.22772233871471));
#57919=CARTESIAN_POINT('Ctrl Pts',(6.98802445798619,-13.9188753060166,7.18834283582162));
#57920=CARTESIAN_POINT('Ctrl Pts',(6.99237688811927,-13.9241325304546,7.14768911906493));
#57921=CARTESIAN_POINT('Ctrl Pts',(6.99536960209117,-13.9298949208174,7.10587570796624));
#57922=CARTESIAN_POINT('Ctrl Pts',(6.99836231606306,-13.9356573111802,7.06406229686755));
#57923=CARTESIAN_POINT('Ctrl Pts',(6.9999959467022,-13.9419248200711,7.02108887996642));
#57924=CARTESIAN_POINT('Ctrl Pts',(6.99999920776358,-13.9487123452195,6.97710990114864));
#57925=CARTESIAN_POINT('Ctrl Pts',(6.99990231887538,-13.8881494970745,6.87915686262218));
#57926=CARTESIAN_POINT('Ctrl Pts',(6.99990231887538,-14.0922215836893,7.13653119174548));
#57927=CARTESIAN_POINT('Ctrl Pts',(6.99990231887538,-14.6760168117915,7.80839106751792));
#57928=CARTESIAN_POINT('Ctrl Pts',(6.99990231887538,-15.7555521603482,8.78349827542946));
#57929=CARTESIAN_POINT('Ctrl Pts',(6.99990231887538,-17.1681240962604,9.71000741139101));
#57930=CARTESIAN_POINT('Ctrl Pts',(6.99990231887538,-18.7078310635836,10.4112072238231));
#57931=CARTESIAN_POINT('Ctrl Pts',(6.99990231887538,-20.3372561090755,10.8675680762032));
#57932=CARTESIAN_POINT('Ctrl Pts',(6.99990231887538,-22.0150940179141,11.0696961448058));
#57933=CARTESIAN_POINT('Ctrl Pts',(6.99990231887538,-23.3220434090589,11.025041445511));
#57934=CARTESIAN_POINT('Ctrl Pts',(6.99990231887538,-24.0577258216087,10.9251841086137));
#57935=CARTESIAN_POINT('Ctrl Pts',(6.99990231887538,-24.2367488249382,10.8963634460966));
#57936=CARTESIAN_POINT('Ctrl Pts',(7.00658753983221,-13.5133853982884,7.17628812110414));
#57937=CARTESIAN_POINT('Ctrl Pts',(7.00658753983221,-13.7263815573694,7.44491987418102));
#57938=CARTESIAN_POINT('Ctrl Pts',(7.00658753983221,-14.335562627462,8.14597361895549));
#57939=CARTESIAN_POINT('Ctrl Pts',(7.00658753983221,-15.461958137829,9.16342028926661));
#57940=CARTESIAN_POINT('Ctrl Pts',(7.00658753983221,-16.9363739076172,10.1305345660181));
#57941=CARTESIAN_POINT('Ctrl Pts',(7.00658753983221,-18.5431139524402,10.8622018415741));
#57942=CARTESIAN_POINT('Ctrl Pts',(7.00658753983221,-20.2433891695497,11.3384606731685));
#57943=CARTESIAN_POINT('Ctrl Pts',(7.00658753983221,-21.9947090334009,11.5494067320141));
#57944=CARTESIAN_POINT('Ctrl Pts',(7.00658753983221,-23.3583198226927,11.502805648718));
#57945=CARTESIAN_POINT('Ctrl Pts',(7.00658753983221,-24.1259502087164,11.3986200459028));
#57946=CARTESIAN_POINT('Ctrl Pts',(7.00658753983221,-24.3127635599996,11.3685459961419));
#57947=CARTESIAN_POINT('Ctrl Pts',(6.71725767918123,-13.214799698687,7.41302142873519));
#57948=CARTESIAN_POINT('Ctrl Pts',(6.71725767918123,-13.4349059316249,7.69062230617901));
#57949=CARTESIAN_POINT('Ctrl Pts',(6.71725767918123,-14.0643126567709,8.41493567435489));
#57950=CARTESIAN_POINT('Ctrl Pts',(6.71725767918123,-15.2280430512571,9.46611545314552));
#57951=CARTESIAN_POINT('Ctrl Pts',(6.71725767918123,-16.7517316421631,10.4655810527814));
#57952=CARTESIAN_POINT('Ctrl Pts',(6.71725767918123,-18.4118789327983,11.2215226620502));
#57953=CARTESIAN_POINT('Ctrl Pts',(6.71725767918123,-20.1686025880746,11.7136348052723));
#57954=CARTESIAN_POINT('Ctrl Pts',(6.71725767918123,-21.9784677101774,11.9316064191023));
#57955=CARTESIAN_POINT('Ctrl Pts',(6.71725767918123,-23.3872223199659,11.883454593803));
#57956=CARTESIAN_POINT('Ctrl Pts',(6.71725767918123,-24.1803066063053,11.7758205328527));
#57957=CARTESIAN_POINT('Ctrl Pts',(6.71725767918123,-24.3733267594099,11.7447478722026));
#57958=CARTESIAN_POINT('Ctrl Pts',(6.25443115695018,-13.1193849311526,7.48867091075995));
#57959=CARTESIAN_POINT('Ctrl Pts',(6.25443115695018,-13.3417632288447,7.76913792317712));
#57960=CARTESIAN_POINT('Ctrl Pts',(6.25443115695018,-13.9776331777085,8.50088403700404));
#57961=CARTESIAN_POINT('Ctrl Pts',(6.25443115695018,-15.1532941478884,9.56284342348165));
#57962=CARTESIAN_POINT('Ctrl Pts',(6.25443115695018,-16.6927281505116,10.5726470733296));
#57963=CARTESIAN_POINT('Ctrl Pts',(6.25443115695018,-18.3699420319087,11.3363456847244));
#57964=CARTESIAN_POINT('Ctrl Pts',(6.25443115695018,-20.1447041083536,11.8335238443235));
#57965=CARTESIAN_POINT('Ctrl Pts',(6.25443115695018,-21.9732777024755,12.0537405144227));
#57966=CARTESIAN_POINT('Ctrl Pts',(6.25443115695018,-23.3964582782285,12.0050931406458));
#57967=CARTESIAN_POINT('Ctrl Pts',(6.25443115695018,-24.1976765039544,11.8963571051786));
#57968=CARTESIAN_POINT('Ctrl Pts',(6.25443115695018,-24.3926800760654,11.864965332708));
#57969=CARTESIAN_POINT('Ctrl Pts',(6.99999999975193,-13.9487123452043,6.97710990119063));
#57970=CARTESIAN_POINT('Ctrl Pts',(6.99999999975356,-14.0537865445291,7.10682522671275));
#57971=CARTESIAN_POINT('Ctrl Pts',(6.99999999939392,-14.1614773187861,7.23374878526825));
#57972=CARTESIAN_POINT('Ctrl Pts',(6.9999999987102,-14.271796727239,7.35798005418243));
#57973=CARTESIAN_POINT('Ctrl Pts',(6.99999999819793,-14.3544522543465,7.45105888010567));
#57974=CARTESIAN_POINT('Ctrl Pts',(6.99999999754858,-14.4385843437506,7.54262579415969));
#57975=CARTESIAN_POINT('Ctrl Pts',(6.99999999746792,-14.5242127791809,7.63271038363396));
#57976=CARTESIAN_POINT('Ctrl Pts',(6.99999999735988,-14.6388965267303,7.7533623407257));
#57977=CARTESIAN_POINT('Ctrl Pts',(6.99999999919156,-14.7562632766479,7.87135693200949));
#57978=CARTESIAN_POINT('Ctrl Pts',(6.99999999987966,-14.8764168439348,7.98675539947756));
#57979=CARTESIAN_POINT('Ctrl Pts',(6.9999999999543,-14.889450370199,7.99927312151074));
#57980=CARTESIAN_POINT('Ctrl Pts',(7.0000000000004,-14.9025167201923,8.01176025725755));
#57981=CARTESIAN_POINT('Ctrl Pts',(7.0000000000004,-14.9156160496649,8.02421685618018));
#57982=CARTESIAN_POINT('Ctrl Pts',(7.0000000000004,-15.0670348546121,8.16820615933681));
#57983=CARTESIAN_POINT('Ctrl Pts',(6.99999999546748,-15.2227875870624,8.30815817490327));
#57984=CARTESIAN_POINT('Ctrl Pts',(6.99999999503653,-15.3825084355945,8.44364293588376));
#57985=CARTESIAN_POINT('Ctrl Pts',(6.99999999469253,-15.5100021830308,8.55179074536915));
#57986=CARTESIAN_POINT('Ctrl Pts',(6.9999999963596,-15.640023426811,8.65709269262027));
#57987=CARTESIAN_POINT('Ctrl Pts',(6.99999999805392,-15.7723691311277,8.75934684041249));
#57988=CARTESIAN_POINT('Ctrl Pts',(6.99999999906437,-15.8512969250208,8.82032875397988));
#57989=CARTESIAN_POINT('Ctrl Pts',(7.0000000000004,-15.9310511663872,8.88022697138982));
#57990=CARTESIAN_POINT('Ctrl Pts',(7.0000000000004,-16.0115798553702,8.93900894895164));
#57991=CARTESIAN_POINT('Ctrl Pts',(7.0000000000004,-16.2272079359332,9.09640682979922));
#57992=CARTESIAN_POINT('Ctrl Pts',(6.9999999976986,-16.4484492824618,9.24573591234888));
#57993=CARTESIAN_POINT('Ctrl Pts',(6.9999999985899,-16.6747881471727,9.38679488637287));
#57994=CARTESIAN_POINT('Ctrl Pts',(6.99999999924458,-16.8410388017354,9.4904056683452));
#57995=CARTESIAN_POINT('Ctrl Pts',(6.99999999995148,-17.0100406501369,9.58955400758841));
#57996=CARTESIAN_POINT('Ctrl Pts',(6.99999999999604,-17.1816029459403,9.68414853143226));
#57997=CARTESIAN_POINT('Ctrl Pts',(6.99999999999906,-17.1932035655252,9.69054477998316));
#57998=CARTESIAN_POINT('Ctrl Pts',(7.0000000000004,-17.204815895814,9.69692020378814));
#57999=CARTESIAN_POINT('Ctrl Pts',(7.0000000000004,-17.2164398762232,9.70327477688506));
#58000=CARTESIAN_POINT('Ctrl Pts',(7.0000000000004,-17.5356664538813,9.8777888891596));
#58001=CARTESIAN_POINT('Ctrl Pts',(6.9999999999951,-17.8636599576002,10.0365925445825));
#58002=CARTESIAN_POINT('Ctrl Pts',(6.9999999999726,-18.1987775349499,10.1787296000036));
#58003=CARTESIAN_POINT('Ctrl Pts',(6.99999999996567,-18.3020189970942,10.2225185219175));
#58004=CARTESIAN_POINT('Ctrl Pts',(7.0000000000004,-18.4059362502178,10.2647257190842));
#58005=CARTESIAN_POINT('Ctrl Pts',(7.0000000000004,-18.5104803250287,10.3053235815522));
#58006=CARTESIAN_POINT('Ctrl Pts',(7.0000000000004,-18.5793538172857,10.3320693973376));
#58007=CARTESIAN_POINT('Ctrl Pts',(6.99999999997084,-18.6484986914509,10.3581192795794));
#58008=CARTESIAN_POINT('Ctrl Pts',(6.99999999992955,-18.7179006488757,10.3834661744317));
#58009=CARTESIAN_POINT('Ctrl Pts',(6.99999999970469,-19.0957945309358,10.5214800986681));
#58010=CARTESIAN_POINT('Ctrl Pts',(7.0000000000004,-19.481310861725,10.6386470274233));
#58011=CARTESIAN_POINT('Ctrl Pts',(7.0000000000004,-19.8719302299936,10.7344092108449));
#58012=CARTESIAN_POINT('Ctrl Pts',(7.0000000000004,-20.028335196057,10.7727526271343));
#58013=CARTESIAN_POINT('Ctrl Pts',(6.99999999962046,-20.1855590343142,10.8076629791835));
#58014=CARTESIAN_POINT('Ctrl Pts',(6.9999999991226,-20.3434794936074,10.8391040063824));
#58015=CARTESIAN_POINT('Ctrl Pts',(6.9999999982468,-20.6212770476484,10.894411852443));
#58016=CARTESIAN_POINT('Ctrl Pts',(6.99999999886194,-20.9012308716709,10.9389870155385));
#58017=CARTESIAN_POINT('Ctrl Pts',(6.99999999981873,-21.1826749476473,10.9726474512991));
#58018=CARTESIAN_POINT('Ctrl Pts',(6.99999999992592,-21.2142039018405,10.9764182833323));
#58019=CARTESIAN_POINT('Ctrl Pts',(7.0000000000004,-21.2457515479638,10.9800520854491));
#58020=CARTESIAN_POINT('Ctrl Pts',(7.0000000000004,-21.2773169407793,10.9835485617856));
#58021=CARTESIAN_POINT('Ctrl Pts',(7.0000000000004,-21.4971771481314,11.007902322147));
#58022=CARTESIAN_POINT('Ctrl Pts',(6.99999999634339,-21.7179002558227,11.0256402092761));
#58023=CARTESIAN_POINT('Ctrl Pts',(6.99999999542,-21.9388779061459,11.0366879235032));
#58024=CARTESIAN_POINT('Ctrl Pts',(6.9999999953102,-21.9651560171461,11.0380016901232));
#58025=CARTESIAN_POINT('Ctrl Pts',(6.99999999523508,-21.991437727015,11.0392209091003));
#58026=CARTESIAN_POINT('Ctrl Pts',(6.99999999519962,-22.0177220131473,11.0403455046552));
#58027=CARTESIAN_POINT('Ctrl Pts',(6.99999999489106,-22.2464396793239,11.0501313846829));
#58028=CARTESIAN_POINT('Ctrl Pts',(7.0000000000004,-22.4753517979991,11.0527476023975));
#58029=CARTESIAN_POINT('Ctrl Pts',(7.0000000000004,-22.7037893032828,11.0482957738581));
#58030=CARTESIAN_POINT('Ctrl Pts',(7.0000000000004,-22.8739866007358,11.0449789402883));
#58031=CARTESIAN_POINT('Ctrl Pts',(6.99999999741537,-23.0439121332079,11.0376823617801));
#58032=CARTESIAN_POINT('Ctrl Pts',(6.99999999745857,-23.2136663743515,11.0264413935634));
#58033=CARTESIAN_POINT('Ctrl Pts',(6.99999999749981,-23.3756611564429,11.0157142495198));
#58034=CARTESIAN_POINT('Ctrl Pts',(6.99999999865199,-23.5375002857097,11.0013947135119));
#58035=CARTESIAN_POINT('Ctrl Pts',(6.99999999924109,-23.6992706986834,10.9834692572149));
#58036=CARTESIAN_POINT('Ctrl Pts',(6.99999999975915,-23.8415340467228,10.9677053398146));
#58037=CARTESIAN_POINT('Ctrl Pts',(6.99999999990903,-23.9837444368193,10.9491520850644));
#58038=CARTESIAN_POINT('Ctrl Pts',(6.99999999989437,-24.1259362010629,10.9277733094969));
#58039=CARTESIAN_POINT('Ctrl Pts',(6.26386081916884,-13.9442638623473,8.42073287747484));
#58040=CARTESIAN_POINT('Ctrl Pts',(6.26460715538793,-14.1256643553291,8.60589469623759));
#58041=CARTESIAN_POINT('Ctrl Pts',(6.26531568179332,-14.3114846099631,8.78358334204671));
#58042=CARTESIAN_POINT('Ctrl Pts',(6.26598638151121,-14.5010840416007,8.95374216520787));
#58043=CARTESIAN_POINT('Ctrl Pts',(6.26666473066603,-14.6928458849018,9.1258416768018));
#58044=CARTESIAN_POINT('Ctrl Pts',(6.2673043853985,-14.8884736297165,9.29023867958107));
#58045=CARTESIAN_POINT('Ctrl Pts',(6.26790533159812,-15.0873464622826,9.4469072536487));
#58046=CARTESIAN_POINT('Ctrl Pts',(6.26800176179048,-15.1192583797085,9.47204690965087));
#58047=CARTESIAN_POINT('Ctrl Pts',(6.2680971952959,-15.1512539400177,9.49698763549614));
#58048=CARTESIAN_POINT('Ctrl Pts',(6.26819163206334,-15.1833306763749,9.52172939986302));
#58049=CARTESIAN_POINT('Ctrl Pts',(6.26876871803122,-15.3793457979045,9.67292183712407));
#58050=CARTESIAN_POINT('Ctrl Pts',(6.26930858350217,-15.5783882018843,9.81668297483491));
#58051=CARTESIAN_POINT('Ctrl Pts',(6.26981121831375,-15.7798035976635,9.95308941123838));
#58052=CARTESIAN_POINT('Ctrl Pts',(6.27017912497558,-15.9272308434424,10.0529329467719));
#58053=CARTESIAN_POINT('Ctrl Pts',(6.27052708500013,-16.0759304839668,10.148836571751));
#58054=CARTESIAN_POINT('Ctrl Pts',(6.27085509519045,-16.2256622310779,10.2408371358993));
#58055=CARTESIAN_POINT('Ctrl Pts',(6.27121137948388,-16.3883006834675,10.3407680434105));
#58056=CARTESIAN_POINT('Ctrl Pts',(6.27154412512549,-16.5521566156048,10.436093917001));
#58057=CARTESIAN_POINT('Ctrl Pts',(6.27185332803515,-16.7169398449731,10.5268692971855));
#58058=CARTESIAN_POINT('Ctrl Pts',(6.27227096956888,-16.9395131730253,10.6494799448244));
#58059=CARTESIAN_POINT('Ctrl Pts',(6.27264565965075,-17.1637762166304,10.7637883382869));
#58060=CARTESIAN_POINT('Ctrl Pts',(6.27297739034783,-17.3890719580496,10.8699987576102));
#58061=CARTESIAN_POINT('Ctrl Pts',(6.27330912104492,-17.6143676994688,10.9762091769336));
#58062=CARTESIAN_POINT('Ctrl Pts',(6.27359789237642,-17.840696315615,11.0743217071008));
#58063=CARTESIAN_POINT('Ctrl Pts',(6.27384369855202,-18.0674568527804,11.164557360519));
#58064=CARTESIAN_POINT('Ctrl Pts',(6.27395596457378,-18.1710242401169,11.2057703113523));
#58065=CARTESIAN_POINT('Ctrl Pts',(6.27405926819507,-18.2746824802254,11.2453403802785));
#58066=CARTESIAN_POINT('Ctrl Pts',(6.27415361604219,-18.3783780729687,11.283289714812));
#58067=CARTESIAN_POINT('Ctrl Pts',(6.27415652049381,-18.3815702902948,11.2844579662295));
#58068=CARTESIAN_POINT('Ctrl Pts',(6.27415941639736,-18.3847625430648,11.2856246817208));
#58069=CARTESIAN_POINT('Ctrl Pts',(6.27416230375866,-18.3879548297647,11.2867898619452));
#58070=CARTESIAN_POINT('Ctrl Pts',(6.27420631274101,-18.4366114662014,11.3045494668581));
#58071=CARTESIAN_POINT('Ctrl Pts',(6.27424833721605,-18.4852759753122,11.3219524031927));
#58072=CARTESIAN_POINT('Ctrl Pts',(6.27428839779756,-18.5339427586306,11.3390018888015));
#58073=CARTESIAN_POINT('Ctrl Pts',(6.27431785032599,-18.5697225642477,11.351536665899));
#58074=CARTESIAN_POINT('Ctrl Pts',(6.27434670203493,-18.6061342790989,11.364096691144));
#58075=CARTESIAN_POINT('Ctrl Pts',(6.27437398879412,-18.6418708872981,11.3762338190514));
#58076=CARTESIAN_POINT('Ctrl Pts',(6.27438625183395,-18.6579314039148,11.3816884090155));
#58077=CARTESIAN_POINT('Ctrl Pts',(6.27439819879666,-18.6738553337517,11.3870582624603));
#58078=CARTESIAN_POINT('Ctrl Pts',(6.27440974216804,-18.6895229537664,11.3923059388776));
#58079=CARTESIAN_POINT('Ctrl Pts',(6.2745606464126,-18.8943426971077,11.4609077900793));
#58080=CARTESIAN_POINT('Ctrl Pts',(6.27467736446985,-19.1037514751474,11.5248694916449));
#58081=CARTESIAN_POINT('Ctrl Pts',(6.27475989460005,-19.3175737472424,11.5836612187159));
#58082=CARTESIAN_POINT('Ctrl Pts',(6.27484107125348,-19.5278893790404,11.6414887738264));
#58083=CARTESIAN_POINT('Ctrl Pts',(6.27488917214012,-19.7424750147591,11.6943145252498));
#58084=CARTESIAN_POINT('Ctrl Pts',(6.27490419657665,-19.9611187691495,11.7416109919988));
#58085=CARTESIAN_POINT('Ctrl Pts',(6.27490863040175,-20.0256421983445,11.7555685378339));
#58086=CARTESIAN_POINT('Ctrl Pts',(6.27491018365523,-20.0905187370529,11.7690443907007));
#58087=CARTESIAN_POINT('Ctrl Pts',(6.27490885633516,-20.1557421590437,11.7820245992169));
#58088=CARTESIAN_POINT('Ctrl Pts',(6.27490450759592,-20.3694356466198,11.8245520524328));
#58089=CARTESIAN_POINT('Ctrl Pts',(6.27486923773407,-20.5868563220246,11.8617604278984));
#58090=CARTESIAN_POINT('Ctrl Pts',(6.27480304721734,-20.8077282531982,11.8931697209086));
#58091=CARTESIAN_POINT('Ctrl Pts',(6.27475276868315,-20.9755032984753,11.9170283231715));
#58092=CARTESIAN_POINT('Ctrl Pts',(6.27468464903527,-21.1452687904443,11.9375405125988));
#58093=CARTESIAN_POINT('Ctrl Pts',(6.27459868879999,-21.3168849074982,11.9544888627757));
#58094=CARTESIAN_POINT('Ctrl Pts',(6.27448994477113,-21.5339879426928,11.9759293797162));
#58095=CARTESIAN_POINT('Ctrl Pts',(6.27435264840743,-21.7540541848264,11.9916670215249));
#58096=CARTESIAN_POINT('Ctrl Pts',(6.27418680218902,-21.9767610896238,12.0012473074002));
#58097=CARTESIAN_POINT('Ctrl Pts',(6.27401315229541,-22.2099471742547,12.0112783809986));
#58098=CARTESIAN_POINT('Ctrl Pts',(6.27380820257276,-22.4460283952983,12.0145579437078));
#58099=CARTESIAN_POINT('Ctrl Pts',(6.27357195679918,-22.6846248575645,12.0106606645995));
#58100=CARTESIAN_POINT('Ctrl Pts',(6.27333930405051,-22.9195925436593,12.0068226585978));
#58101=CARTESIAN_POINT('Ctrl Pts',(6.27307629996098,-23.156999600613,11.9960244224841));
#58102=CARTESIAN_POINT('Ctrl Pts',(6.27278294912994,-23.3964330132993,11.9778552766724));
#58103=CARTESIAN_POINT('Ctrl Pts',(6.27261681982308,-23.5320280165442,11.9675657963629));
#58104=CARTESIAN_POINT('Ctrl Pts',(6.27244095791103,-23.6682719810853,11.9549122836599));
#58105=CARTESIAN_POINT('Ctrl Pts',(6.27225536438287,-23.8050824682318,11.9398195552085));
#58106=CARTESIAN_POINT('Ctrl Pts',(6.27204648910949,-23.9590551211918,11.9228335222769));
#58107=CARTESIAN_POINT('Ctrl Pts',(6.27182528751364,-24.1137456239823,11.9027579534488));
#58108=CARTESIAN_POINT('Ctrl Pts',(6.27159176118849,-24.269011967666,11.87948072114));
#58109=CARTESIAN_POINT('Ctrl Pts',(-6.390310997256,-13.7249660551165,8.13937950337913));
#58110=CARTESIAN_POINT('Ctrl Pts',(-4.260207331504,-13.822173858898,9.11426650159885));
#58111=CARTESIAN_POINT('Ctrl Pts',(0.0001535201704872,-13.9182984617654,
10.0902631575042));
#58112=CARTESIAN_POINT('Ctrl Pts',(4.260514371845,-13.8221669310363,9.11419615987158));
#58113=CARTESIAN_POINT('Ctrl Pts',(6.390771557767,-13.7249450365591,8.1391687105328));
#58114=CARTESIAN_POINT('Ctrl Pts',(-6.390310997256,-14.2543287817417,8.7130969045735));
#58115=CARTESIAN_POINT('Ctrl Pts',(-4.260207331504,-14.3567676707194,9.62713419180754));
#58116=CARTESIAN_POINT('Ctrl Pts',(0.0001535201704872,-14.4578350530966,
10.5425537312277));
#58117=CARTESIAN_POINT('Ctrl Pts',(4.260514371845,-14.3567603866204,9.62706821596995));
#58118=CARTESIAN_POINT('Ctrl Pts',(6.390771557767,-14.2543066321015,8.71289926882854));
#58119=CARTESIAN_POINT('Ctrl Pts',(-6.390310997256,-15.6641218055026,9.9697330099508));
#58120=CARTESIAN_POINT('Ctrl Pts',(-4.260207331504,-15.7526919792921,10.7489906364295));
#58121=CARTESIAN_POINT('Ctrl Pts',(0.0001535201704857,-15.8421753984647,
11.5273040839031));
#58122=CARTESIAN_POINT('Ctrl Pts',(4.260514371845,-15.7526855300687,10.7489345420609));
#58123=CARTESIAN_POINT('Ctrl Pts',(6.390771557767,-15.6641026546149,9.96956451662773));
#58124=CARTESIAN_POINT('Ctrl Pts',(-6.390310997256,-18.3168609125049,11.387980958503));
#58125=CARTESIAN_POINT('Ctrl Pts',(-4.260207331504,-18.3050659003902,12.0191857141868));
#58126=CARTESIAN_POINT('Ctrl Pts',(0.0001535201704865,-18.2929947853426,
12.6510838649568));
#58127=CARTESIAN_POINT('Ctrl Pts',(4.260514371845,-18.3050667703783,12.019140172221));
#58128=CARTESIAN_POINT('Ctrl Pts',(6.390771557767,-18.3168634628512,11.3878444776082));
#58129=CARTESIAN_POINT('Ctrl Pts',(-6.390310997256,-21.4528914163396,12.0713618431172));
#58130=CARTESIAN_POINT('Ctrl Pts',(-4.260207331504,-21.2792389757099,12.6592425323955));
#58131=CARTESIAN_POINT('Ctrl Pts',(0.0001535201704863,-21.1056340488841,
13.2456889758127));
#58132=CARTESIAN_POINT('Ctrl Pts',(4.260514371845,-21.2792514877097,12.6592002662086));
#58133=CARTESIAN_POINT('Ctrl Pts',(6.390771557767,-21.4529289639657,12.0712347298623));
#58134=CARTESIAN_POINT('Ctrl Pts',(-6.390310997256,-23.5458951845813,11.9720502124476));
#58135=CARTESIAN_POINT('Ctrl Pts',(-4.260207331504,-23.2652553028773,12.6077625569466));
#58136=CARTESIAN_POINT('Ctrl Pts',(0.0001535201704863,-22.9846380445226,
13.2461450660854));
#58137=CARTESIAN_POINT('Ctrl Pts',(4.260514371845,-23.2652755274378,12.6077165476319));
#58138=CARTESIAN_POINT('Ctrl Pts',(6.390771557767,-23.5459558653483,11.9719127569248));
#58139=CARTESIAN_POINT('Ctrl Pts',(-6.390310997256,-24.5118462831682,11.8061936875796));
#58140=CARTESIAN_POINT('Ctrl Pts',(-4.260207331504,-24.187054612813,12.4817978962137));
#58141=CARTESIAN_POINT('Ctrl Pts',(0.0001535201704863,-23.8622603664262,
13.1582606881552));
#58142=CARTESIAN_POINT('Ctrl Pts',(4.260514371845,-24.187078021279,12.4817491423984));
#58143=CARTESIAN_POINT('Ctrl Pts',(6.390771557767,-24.5119165105465,11.8060476065166));
#58144=CARTESIAN_POINT('Ctrl Pts',(-6.26386059986259,-13.9442583573832,
8.42071137118441));
#58145=CARTESIAN_POINT('Ctrl Pts',(-5.97374970119676,-13.9556246846561,
8.54581702332281));
#58146=CARTESIAN_POINT('Ctrl Pts',(-5.68169246539988,-13.9653430040926,
8.66221523046253));
#58147=CARTESIAN_POINT('Ctrl Pts',(-5.38818163422549,-13.9736733100379,
8.76975971946819));
#58148=CARTESIAN_POINT('Ctrl Pts',(-5.1130280735255,-13.9814826073419,8.87057797195028));
#58149=CARTESIAN_POINT('Ctrl Pts',(-4.83659705802325,-13.9880722696807,
8.96361469734395));
#58150=CARTESIAN_POINT('Ctrl Pts',(-4.55929453756362,-13.993667873811,9.04879103044236));
#58151=CARTESIAN_POINT('Ctrl Pts',(-4.30183369063218,-13.9988630987808,
9.12787278859474));
#58152=CARTESIAN_POINT('Ctrl Pts',(-4.04362159347591,-14.0032015562529,
9.20017851794789));
#58153=CARTESIAN_POINT('Ctrl Pts',(-3.78498314220327,-14.0068718216736,
9.26568816177216));
#58154=CARTESIAN_POINT('Ctrl Pts',(-3.57030053449505,-14.0099183220977,
9.3200643811511));
#58155=CARTESIAN_POINT('Ctrl Pts',(-3.35532417670103,-14.0125045919245,
9.3697587733089));
#58156=CARTESIAN_POINT('Ctrl Pts',(-3.14023987314758,-14.0147423985495,
9.41478705629016));
#58157=CARTESIAN_POINT('Ctrl Pts',(-2.90175388934231,-14.017223683821,9.46471452281576));
#58158=CARTESIAN_POINT('Ctrl Pts',(-2.66312286525269,-14.0192917524254,
9.50892010592155));
#58159=CARTESIAN_POINT('Ctrl Pts',(-2.42459507108778,-14.0210013809793,
9.54737540544549));
#58160=CARTESIAN_POINT('Ctrl Pts',(-2.18947802829743,-14.0226865632502,
9.58528082579845));
#58161=CARTESIAN_POINT('Ctrl Pts',(-1.95446128433272,-14.0240235028694,
9.6175991989134));
#58162=CARTESIAN_POINT('Ctrl Pts',(-1.71978261078597,-14.0250694407982,
9.64435373630295));
#58163=CARTESIAN_POINT('Ctrl Pts',(-1.48662499776981,-14.0261085995218,
9.67093486521775));
#58164=CARTESIAN_POINT('Ctrl Pts',(-1.25380108699366,-14.0268605301828,
9.69202397759681));
#58165=CARTESIAN_POINT('Ctrl Pts',(-1.02154405662948,-14.0273858808287,
9.70769485074321));
#58166=CARTESIAN_POINT('Ctrl Pts',(-0.790903926706924,-14.0279075741485,
9.72325662819648));
#58167=CARTESIAN_POINT('Ctrl Pts',(-0.560822811783745,-14.0282058441238,
9.7334753107035));
#58168=CARTESIAN_POINT('Ctrl Pts',(-0.331529053916802,-14.0283443468537,
9.73847438258332));
#58169=CARTESIAN_POINT('Ctrl Pts',(-0.220829317145543,-14.0284112139846,
9.74088786276849));
#58170=CARTESIAN_POINT('Ctrl Pts',(-0.110313099121724,-14.028440904815,
9.74208551519516));
#58171=CARTESIAN_POINT('Ctrl Pts',(-6.09486637782099E-6,-14.0284409294581,
9.74208557977705));
#58172=CARTESIAN_POINT('Ctrl Pts',(-4.06324399737009E-6,-14.0284409294585,
9.74208557977824));
#58173=CARTESIAN_POINT('Ctrl Pts',(-2.03162154622285E-6,-14.028440929459,
9.74208557977902));
#58174=CARTESIAN_POINT('Ctrl Pts',(9.73437423716373E-13,-14.0284409294594,
9.7420855797794));
#58175=CARTESIAN_POINT('Ctrl Pts',(0.230469086304145,-14.0284409786639,
9.7420856225606));
#58176=CARTESIAN_POINT('Ctrl Pts',(0.461828188180037,-14.0283111792431,
9.736854391521));
#58177=CARTESIAN_POINT('Ctrl Pts',(0.693853393917424,-14.0279844554711,
9.72624208054898));
#58178=CARTESIAN_POINT('Ctrl Pts',(0.927890614266204,-14.0276548985026,
9.71553774455464));
#58179=CARTESIAN_POINT('Ctrl Pts',(1.16260554084993,-14.0271249736896,9.69935860948583));
#58180=CARTESIAN_POINT('Ctrl Pts',(1.39776838632542,-14.0263301126495,9.67760396297315));
#58181=CARTESIAN_POINT('Ctrl Pts',(1.63451272885995,-14.0255299060779,9.65570301397203));
#58182=CARTESIAN_POINT('Ctrl Pts',(1.87171103515599,-14.0244611738864,9.62815137182254));
#58183=CARTESIAN_POINT('Ctrl Pts',(2.10912885058401,-14.0230625490103,9.59489921480226));
#58184=CARTESIAN_POINT('Ctrl Pts',(2.34955154624848,-14.0216462224287,9.56122620162479));
#58185=CARTESIAN_POINT('Ctrl Pts',(2.59019934264518,-14.0198915802255,9.52170750950915));
#58186=CARTESIAN_POINT('Ctrl Pts',(2.83082876986943,-14.0177397699997,9.47634475584401));
#58187=CARTESIAN_POINT('Ctrl Pts',(2.93381742979539,-14.016818801795,9.45692963582143));
#58188=CARTESIAN_POINT('Ctrl Pts',(3.03680272483088,-14.0158251417994,9.43644464777512));
#58189=CARTESIAN_POINT('Ctrl Pts',(3.13976556667399,-14.0147544567981,9.41489280609712));
#58190=CARTESIAN_POINT('Ctrl Pts',(3.40252021405499,-14.0120221365268,9.35989387192684));
#58191=CARTESIAN_POINT('Ctrl Pts',(3.66512390726434,-14.0087696417089,9.29792768492639));
#58192=CARTESIAN_POINT('Ctrl Pts',(3.92723730947002,-14.0047935953969,9.22896929728601));
#58193=CARTESIAN_POINT('Ctrl Pts',(4.19824548982516,-14.0006826225623,9.15767081732511));
#58194=CARTESIAN_POINT('Ctrl Pts',(4.46872953867013,-13.9957980909824,9.07889806286959));
#58195=CARTESIAN_POINT('Ctrl Pts',(4.73831438756763,-13.989924171619,8.99268353198578));
#58196=CARTESIAN_POINT('Ctrl Pts',(5.03386704909763,-13.9834844458385,8.89816436976476));
#58197=CARTESIAN_POINT('Ctrl Pts',(5.32833893619776,-13.9758553153082,8.79470102870764));
#58198=CARTESIAN_POINT('Ctrl Pts',(5.62123581932587,-13.966765452181,8.68240143317886));
#58199=CARTESIAN_POINT('Ctrl Pts',(5.83635809277611,-13.9600892731776,8.59992140116319));
#58200=CARTESIAN_POINT('Ctrl Pts',(6.05063074977934,-13.9526253913755,8.51267626970352));
#58201=CARTESIAN_POINT('Ctrl Pts',(6.26385797775638,-13.9442712877421,8.42072561436248));
#58202=CARTESIAN_POINT('Ctrl Pts',(-6.38246443203547,-13.9383908459212,
8.36787486373552));
#58203=CARTESIAN_POINT('Ctrl Pts',(-5.84028083115186,-13.9679405559834,
8.61420389076076));
#58204=CARTESIAN_POINT('Ctrl Pts',(-4.52658547446533,-14.0220197310707,
9.12779052120603));
#58205=CARTESIAN_POINT('Ctrl Pts',(-2.38698044041613,-14.0625412099017,
9.65161902433709));
#58206=CARTESIAN_POINT('Ctrl Pts',(0.000170347585844104,-14.074148905673,
9.84433435176279));
#58207=CARTESIAN_POINT('Ctrl Pts',(2.38732116864064,-14.0625376336816,9.6515638422071));
#58208=CARTESIAN_POINT('Ctrl Pts',(4.52680602897707,-14.0220126621885,9.12771374035583));
#58209=CARTESIAN_POINT('Ctrl Pts',(5.8403891997243,-13.9679346096076,8.61415461209718));
#58210=CARTESIAN_POINT('Ctrl Pts',(6.3824653352414,-13.9383907598281,8.36787438517324));
#58211=CARTESIAN_POINT('Ctrl Pts',(-6.17792169704451,-13.4668082109749,
7.96586380831044));
#58212=CARTESIAN_POINT('Ctrl Pts',(-5.65283597290228,-13.4968949842233,
8.20286290735405));
#58213=CARTESIAN_POINT('Ctrl Pts',(-4.38071778940755,-13.5523312148905,
8.69705174761694));
#58214=CARTESIAN_POINT('Ctrl Pts',(-2.30965986038465,-13.594711467794,9.20104086192968));
#58215=CARTESIAN_POINT('Ctrl Pts',(0.000164816889377721,-13.6071139576131,
9.38641545191658));
#58216=CARTESIAN_POINT('Ctrl Pts',(2.30998959809195,-13.5947076725133,9.20098777798778));
#58217=CARTESIAN_POINT('Ctrl Pts',(4.38093134257534,-13.5523239111862,8.69697786471346));
#58218=CARTESIAN_POINT('Ctrl Pts',(5.6529409239163,-13.496888930705,8.20281549558108));
#58219=CARTESIAN_POINT('Ctrl Pts',(6.17792257224339,-13.4668081241968,7.9658633476716));
#58220=CARTESIAN_POINT('Ctrl Pts',(-6.17627932975538,-12.819634948171,8.03444485753682));
#58221=CARTESIAN_POINT('Ctrl Pts',(-5.6525453615486,-12.8494142008257,8.26859095498002));
#58222=CARTESIAN_POINT('Ctrl Pts',(-4.38305006790979,-12.9043210586211,
8.75729081380155));
#58223=CARTESIAN_POINT('Ctrl Pts',(-2.31263925115347,-12.9463212003266,
9.25691132133251));
#58224=CARTESIAN_POINT('Ctrl Pts',(0.000165084886385522,-12.9586088807456,
9.44103069662757));
#58225=CARTESIAN_POINT('Ctrl Pts',(2.31296921096063,-12.9463174397802,9.25685862519176));
#58226=CARTESIAN_POINT('Ctrl Pts',(4.38326327239891,-12.9043138199759,8.75721768025679));
#58227=CARTESIAN_POINT('Ctrl Pts',(5.65265004295757,-12.8494082113494,8.26854411454389));
#58228=CARTESIAN_POINT('Ctrl Pts',(6.17628020062437,-12.8196348638585,8.03444440429756));
#58229=CARTESIAN_POINT('Ctrl Pts',(-6.37611008149986,-12.4394857929392,
8.52104497605786));
#58230=CARTESIAN_POINT('Ctrl Pts',(-5.83725935363331,-12.4683328075045,
8.76067527638475));
#58231=CARTESIAN_POINT('Ctrl Pts',(-4.53013633532534,-12.5212077719813,
9.26135585406044));
#58232=CARTESIAN_POINT('Ctrl Pts',(-2.39288391276903,-12.5608756708728,
9.77485740321018));
#58233=CARTESIAN_POINT('Ctrl Pts',(0.000170896469408238,-12.5722284770212,
9.96458495286569));
#58234=CARTESIAN_POINT('Ctrl Pts',(2.39322501551571,-12.5608721720362,9.77480314203578));
#58235=CARTESIAN_POINT('Ctrl Pts',(4.53035599764022,-12.5212008502468,9.26128083830177));
#58236=CARTESIAN_POINT('Ctrl Pts',(5.83736705737718,-12.4683270075272,8.76062733918381));
#58237=CARTESIAN_POINT('Ctrl Pts',(6.37611097436569,-12.4394857125263,8.52104451479218));
#58238=CARTESIAN_POINT('Ctrl Pts',(-6.24994453580111,-12.4626498782336,
8.5516892069173));
#58239=CARTESIAN_POINT('Ctrl Pts',(-5.92266396136831,-12.4795853537977,
8.69426559471729));
#58240=CARTESIAN_POINT('Ctrl Pts',(-5.59137421024021,-12.4941004954635,
8.82614963762332));
#58241=CARTESIAN_POINT('Ctrl Pts',(-5.25652165743914,-12.5066279941841,
8.94692518664224));
#58242=CARTESIAN_POINT('Ctrl Pts',(-5.07745905565674,-12.5133270815764,
9.01150998331803));
#58243=CARTESIAN_POINT('Ctrl Pts',(-4.89737714265432,-12.5194574385904,
9.07291754746856));
#58244=CARTESIAN_POINT('Ctrl Pts',(-4.71634131068421,-12.5250830890805,
9.13107930125512));
#58245=CARTESIAN_POINT('Ctrl Pts',(-4.71594239822594,-12.5250954852015,
9.1312074606804));
#58246=CARTESIAN_POINT('Ctrl Pts',(-4.71554348114866,-12.5251078788533,
9.13133560436434));
#58247=CARTESIAN_POINT('Ctrl Pts',(-4.7151445594529,-12.5251202700365,9.13146373230635));
#58248=CARTESIAN_POINT('Ctrl Pts',(-4.45574827245172,-12.5331775578975,
9.21477810896677));
#58249=CARTESIAN_POINT('Ctrl Pts',(-4.19440038798913,-12.5401916346868,
9.29143869421521));
#58250=CARTESIAN_POINT('Ctrl Pts',(-3.93132276388625,-12.546313096607,9.3612957382668));
#58251=CARTESIAN_POINT('Ctrl Pts',(-3.79958166025011,-12.5493785346198,
9.39627797634766));
#58252=CARTESIAN_POINT('Ctrl Pts',(-3.66740695004575,-12.5522194472211,
9.42955435298118));
#58253=CARTESIAN_POINT('Ctrl Pts',(-3.5348275049362,-12.5548507179461,9.46110763365611));
#58254=CARTESIAN_POINT('Ctrl Pts',(-3.46853778238143,-12.5561663533086,
9.47688427399358));
#58255=CARTESIAN_POINT('Ctrl Pts',(-3.4021468725808,-12.5574295616256,9.49223012786894));
#58256=CARTESIAN_POINT('Ctrl Pts',(-3.33565847252883,-12.558641923233,9.50714318309749));
#58257=CARTESIAN_POINT('Ctrl Pts',(-3.29270944041516,-12.5594250637142,
9.51677646179608));
#58258=CARTESIAN_POINT('Ctrl Pts',(-3.24894270553966,-12.5602006274725,
9.52639899722143));
#58259=CARTESIAN_POINT('Ctrl Pts',(-3.20586447642415,-12.5609423146399,
9.5356786207993));
#58260=CARTESIAN_POINT('Ctrl Pts',(-3.18225429860695,-12.5613488161666,
9.5407645671636));
#58261=CARTESIAN_POINT('Ctrl Pts',(-3.15885115696836,-12.5617452452138,
9.54574841261899));
#58262=CARTESIAN_POINT('Ctrl Pts',(-3.13590449255282,-12.5621279759528,
9.55058190565942));
#58263=CARTESIAN_POINT('Ctrl Pts',(-2.87752273695214,-12.5664375626741,
9.60500752477578));
#58264=CARTESIAN_POINT('Ctrl Pts',(-2.61833357770723,-12.5700171693122,
9.65275239225978));
#58265=CARTESIAN_POINT('Ctrl Pts',(-2.35853328291647,-12.5730079702202,
9.69372098322824));
#58266=CARTESIAN_POINT('Ctrl Pts',(-2.05844140245972,-12.5764626047473,
9.74104326018444));
#58267=CARTESIAN_POINT('Ctrl Pts',(-1.75753439943394,-12.5791314749656,
9.77932590839172));
#58268=CARTESIAN_POINT('Ctrl Pts',(-1.45620395938076,-12.5811117327101,
9.80856738526045));
#58269=CARTESIAN_POINT('Ctrl Pts',(-1.15288133180468,-12.583105082543,9.83800218645898));
#58270=CARTESIAN_POINT('Ctrl Pts',(-0.849129087484969,-12.5844006107004,
9.85827601809503));
#58271=CARTESIAN_POINT('Ctrl Pts',(-0.545330181918182,-12.5850917275183,
9.86933760207849));
#58272=CARTESIAN_POINT('Ctrl Pts',(-0.3635454901294,-12.5855052723185,9.87595654177276));
#58273=CARTESIAN_POINT('Ctrl Pts',(-0.181743814745408,-12.5857023049162,
9.87927608634575));
#58274=CARTESIAN_POINT('Ctrl Pts',(-5.66486730211472E-6,-12.5857020422594,
9.87927649696493));
#58275=CARTESIAN_POINT('Ctrl Pts',(5.22870906782938E-5,-12.5857020421756,
9.87927649709586));
#58276=CARTESIAN_POINT('Ctrl Pts',(0.000110239054679118,-12.585702042071,
9.87927649689034));
#58277=CARTESIAN_POINT('Ctrl Pts',(0.000168191024690234,-12.5857020419454,
9.87927649634836));
#58278=CARTESIAN_POINT('Ctrl Pts',(0.297743100998625,-12.5857013970017,
9.87927371333765));
#58279=CARTESIAN_POINT('Ctrl Pts',(0.595477788875134,-12.585149424772,9.87040370035765));
#58280=CARTESIAN_POINT('Ctrl Pts',(0.89302731170243,-12.5839914134569,9.85270610253088));
#58281=CARTESIAN_POINT('Ctrl Pts',(1.11957567025123,-12.5831097264016,9.83923149937973));
#58282=CARTESIAN_POINT('Ctrl Pts',(1.34601651728224,-12.5818766562194,9.82063849533055));
#58283=CARTESIAN_POINT('Ctrl Pts',(1.57219035281345,-12.5802662194557,9.79692574624548));
#58284=CARTESIAN_POINT('Ctrl Pts',(1.83383500759072,-12.5784032180608,9.76949412917265));
#58285=CARTESIAN_POINT('Ctrl Pts',(2.09512554905751,-12.5760265328939,9.7352226106913));
#58286=CARTESIAN_POINT('Ctrl Pts',(2.35582217161252,-12.5730392452114,9.69414814227475));
#58287=CARTESIAN_POINT('Ctrl Pts',(2.3568381888416,-12.5730276028061,9.69398806207434));
#58288=CARTESIAN_POINT('Ctrl Pts',(2.35785419704612,-12.5730159510797,9.69382787855833));
#58289=CARTESIAN_POINT('Ctrl Pts',(2.35887019620811,-12.5730042900304,9.69366759172347));
#58290=CARTESIAN_POINT('Ctrl Pts',(2.48820019043544,-12.571519915339,9.67326413451434));
#58291=CARTESIAN_POINT('Ctrl Pts',(2.61738376537167,-12.5698845033371,9.65118661417029));
#58292=CARTESIAN_POINT('Ctrl Pts',(2.74639207799835,-12.5680849993724,9.62744286702406));
#58293=CARTESIAN_POINT('Ctrl Pts',(2.81140297034884,-12.5671781790586,9.61547772959771));
#58294=CARTESIAN_POINT('Ctrl Pts',(2.87636935570031,-12.5662296769901,9.60308945563726));
#58295=CARTESIAN_POINT('Ctrl Pts',(2.94128757520422,-12.5652375797244,9.59027920264321));
#58296=CARTESIAN_POINT('Ctrl Pts',(2.98336724997286,-12.5645945070923,9.58197565883359));
#58297=CARTESIAN_POINT('Ctrl Pts',(3.024643377431,-12.5639455463812,9.57365373262523));
#58298=CARTESIAN_POINT('Ctrl Pts',(3.06663870624113,-12.5632662467228,9.56500710690005));
#58299=CARTESIAN_POINT('Ctrl Pts',(3.08943147260578,-12.5628975600415,9.56031419162636));
#58300=CARTESIAN_POINT('Ctrl Pts',(3.11243591374572,-12.5625198480753,9.5555247743268));
#58301=CARTESIAN_POINT('Ctrl Pts',(3.13589407750061,-12.562128525598,9.55058363765296));
#58302=CARTESIAN_POINT('Ctrl Pts',(3.45792607029556,-12.5567564786418,9.48275206710139));
#58303=CARTESIAN_POINT('Ctrl Pts',(3.77778411279328,-12.5502797008164,9.40471925064032));
#58304=CARTESIAN_POINT('Ctrl Pts',(4.09504715332939,-12.5424384023626,9.31680416471889));
#58305=CARTESIAN_POINT('Ctrl Pts',(4.30300519283459,-12.5372986260721,9.2591780104708));
#58306=CARTESIAN_POINT('Ctrl Pts',(4.50984798325849,-12.531572438382,9.19730493485485));
#58307=CARTESIAN_POINT('Ctrl Pts',(4.71545186718156,-12.5251843761894,9.13126398304479));
#58308=CARTESIAN_POINT('Ctrl Pts',(5.031472821928,-12.5153656827164,9.02975653948312));
#58309=CARTESIAN_POINT('Ctrl Pts',(5.3445683477536,-12.5039841300981,8.9184043282054));
#58310=CARTESIAN_POINT('Ctrl Pts',(5.65441445792807,-12.4907289039645,8.79751201703659));
#58311=CARTESIAN_POINT('Ctrl Pts',(5.854308371056,-12.4821774362061,8.71951963193611));
#58312=CARTESIAN_POINT('Ctrl Pts',(6.05284931410823,-12.4728458597741,8.63755576109365));
#58313=CARTESIAN_POINT('Ctrl Pts',(6.24994316851036,-12.4626470416234,8.55169392353473));
#58314=CARTESIAN_POINT('Ctrl Pts',(6.99927526292643,9.44704415986502,24.8232802776653));
#58315=CARTESIAN_POINT('Ctrl Pts',(6.99927526292643,9.41629241490398,24.801050302151));
#58316=CARTESIAN_POINT('Ctrl Pts',(6.99927526292643,8.91758329726219,24.4365954978806));
#58317=CARTESIAN_POINT('Ctrl Pts',(6.99927526292643,8.00909875236458,23.647769984431));
#58318=CARTESIAN_POINT('Ctrl Pts',(6.99927526292643,6.88884119794498,22.3080781927806));
#58319=CARTESIAN_POINT('Ctrl Pts',(6.99927526292643,5.9930919361781,20.8057475120462));
#58320=CARTESIAN_POINT('Ctrl Pts',(6.99927526292643,5.34745705503301,19.1796203432765));
#58321=CARTESIAN_POINT('Ctrl Pts',(6.99927526292643,4.96742028329228,17.4733110856848));
#58322=CARTESIAN_POINT('Ctrl Pts',(6.99927526292643,4.87762649267095,15.9617880871282));
#58323=CARTESIAN_POINT('Ctrl Pts',(6.99927526292643,4.94001610509403,15.0339554789579));
#58324=CARTESIAN_POINT('Ctrl Pts',(6.99927526292643,4.98003572958382,14.6874887993379));
#58325=CARTESIAN_POINT('Ctrl Pts',(7.01783962573763,9.16157764065615,25.2182708006853));
#58326=CARTESIAN_POINT('Ctrl Pts',(7.01783962573763,9.12945983384568,25.1950528668925));
#58327=CARTESIAN_POINT('Ctrl Pts',(7.01783962573763,8.60860591634158,24.8144101938525));
#58328=CARTESIAN_POINT('Ctrl Pts',(7.01783962573763,7.66002850735824,23.9908049285709));
#58329=CARTESIAN_POINT('Ctrl Pts',(7.01783962573763,6.48952991797069,22.5910607154748));
#58330=CARTESIAN_POINT('Ctrl Pts',(7.01783962573763,5.55415345536922,21.0221777162444));
#58331=CARTESIAN_POINT('Ctrl Pts',(7.01783962573763,4.87968438631774,19.3235982272894));
#58332=CARTESIAN_POINT('Ctrl Pts',(7.01783962573763,4.48273427219063,17.5411348960416));
#58333=CARTESIAN_POINT('Ctrl Pts',(7.01783962573763,4.38895295266063,15.9624836593832));
#58334=CARTESIAN_POINT('Ctrl Pts',(7.01783962573763,4.45409550855552,14.9934905513188));
#58335=CARTESIAN_POINT('Ctrl Pts',(7.01783962573763,4.49590504859499,14.6315514586941));
#58336=CARTESIAN_POINT('Ctrl Pts',(6.72784681146792,8.9312011144958,25.5370351335853));
#58337=CARTESIAN_POINT('Ctrl Pts',(6.72784681146792,8.89798087162717,25.5130199000031));
#58338=CARTESIAN_POINT('Ctrl Pts',(6.72784681146792,8.35925570926948,25.119313330773));
#58339=CARTESIAN_POINT('Ctrl Pts',(6.72784681146792,7.37832265037781,24.267640191082));
#58340=CARTESIAN_POINT('Ctrl Pts',(6.72784681146792,6.16727865785568,22.8194326125491));
#58341=CARTESIAN_POINT('Ctrl Pts',(6.72784681146792,5.19992234383034,21.1968407160822));
#58342=CARTESIAN_POINT('Ctrl Pts',(6.72784681146792,4.50218357554392,19.4397909242666));
#58343=CARTESIAN_POINT('Ctrl Pts',(6.72784681146792,4.09158409519261,17.5958699096704));
#58344=CARTESIAN_POINT('Ctrl Pts',(6.72784681146792,3.99458476935429,15.9630449984808));
#58345=CARTESIAN_POINT('Ctrl Pts',(6.72784681146792,4.06194899928686,14.9608346395659));
#58346=CARTESIAN_POINT('Ctrl Pts',(6.72784681146792,4.10520303280751,14.5864090361991));
#58347=CARTESIAN_POINT('Ctrl Pts',(6.25435484201992,8.85825656412263,25.6379660805211));
#58348=CARTESIAN_POINT('Ctrl Pts',(6.25435484201992,8.82468725486408,25.6136983964164));
#58349=CARTESIAN_POINT('Ctrl Pts',(6.25435484201992,8.28030348682288,25.2158553812985));
#58350=CARTESIAN_POINT('Ctrl Pts',(6.25435484201992,7.28912559798158,24.3552950580346));
#58351=CARTESIAN_POINT('Ctrl Pts',(6.25435484201992,6.06524363863058,22.8917424334598));
#58352=CARTESIAN_POINT('Ctrl Pts',(6.25435484201992,5.08776148443815,21.2521445884091));
#58353=CARTESIAN_POINT('Ctrl Pts',(6.25435484201992,4.38265478775795,19.47658123523));
#58354=CARTESIAN_POINT('Ctrl Pts',(6.25435484201992,3.96773348304226,17.6132007594115));
#58355=CARTESIAN_POINT('Ctrl Pts',(6.25435484201992,3.86971523385333,15.963222736331));
#58356=CARTESIAN_POINT('Ctrl Pts',(6.25435484201992,3.93778291659275,14.9504947371498));
#58357=CARTESIAN_POINT('Ctrl Pts',(6.25435484201992,3.9814943227866,14.5721155065288));
#58358=CARTESIAN_POINT('',(7.00000000000001,9.33250976924427,24.7867247203051));
#58359=CARTESIAN_POINT('',(6.99999999999964,4.92969295105241,14.7967973165495));
#58360=CARTESIAN_POINT('Ctrl Pts',(7.00000000000005,9.33250976255615,24.7867247293583));
#58361=CARTESIAN_POINT('Ctrl Pts',(7.00000000000005,9.20047769609296,24.6891841303334));
#58362=CARTESIAN_POINT('Ctrl Pts',(7.00000000006095,9.07102168308161,24.5890317436279));
#58363=CARTESIAN_POINT('Ctrl Pts',(6.99999999867112,8.94403923540431,24.486233382507));
#58364=CARTESIAN_POINT('Ctrl Pts',(6.99999999727843,8.81679607174416,24.3832239593358));
#58365=CARTESIAN_POINT('Ctrl Pts',(6.99999999421914,8.69203630445828,24.2775573748931));
#58366=CARTESIAN_POINT('Ctrl Pts',(6.99999999313357,8.56968906002076,24.1691580041023));
#58367=CARTESIAN_POINT('Ctrl Pts',(6.99999999205182,8.44777245597257,24.0611401796836));
#58368=CARTESIAN_POINT('Ctrl Pts',(6.99999999470457,8.32825110191426,23.9504084532141));
#58369=CARTESIAN_POINT('Ctrl Pts',(6.99999999802626,8.21109171686694,23.8368518662112));
#58370=CARTESIAN_POINT('Ctrl Pts',(6.99999999906757,8.17436385458824,23.8012534317657));
#58371=CARTESIAN_POINT('Ctrl Pts',(7.00000000000005,8.13786840392794,23.7653771393012));
#58372=CARTESIAN_POINT('Ctrl Pts',(7.00000000000005,8.10160516772495,23.7292189109433));
#58373=CARTESIAN_POINT('Ctrl Pts',(7.00000000000005,8.07267838292857,23.7003758897502));
#58374=CARTESIAN_POINT('Ctrl Pts',(6.99999999938506,8.04389549916536,23.671356721074));
#58375=CARTESIAN_POINT('Ctrl Pts',(6.99999999847366,8.01526107836191,23.6421641904065));
#58376=CARTESIAN_POINT('Ctrl Pts',(6.99999999415778,7.87966422274191,23.5039244336721));
#58377=CARTESIAN_POINT('Ctrl Pts',(6.99999998570413,7.7473991572233,23.3617938511783));
#58378=CARTESIAN_POINT('Ctrl Pts',(6.99999998494294,7.61883545625649,23.2161013823617));
#58379=CARTESIAN_POINT('Ctrl Pts',(6.99999998418015,7.49000000656178,23.0701009592567));
#58380=CARTESIAN_POINT('Ctrl Pts',(6.99999998976665,7.36488188650251,22.9205238664381));
#58381=CARTESIAN_POINT('Ctrl Pts',(6.99999999468264,7.24381793950226,22.7677399422963));
#58382=CARTESIAN_POINT('Ctrl Pts',(6.99999999757253,7.17264988363522,22.6779251368291));
#58383=CARTESIAN_POINT('Ctrl Pts',(7.00000000000005,7.10288215896253,22.5870028455032));
#58384=CARTESIAN_POINT('Ctrl Pts',(7.00000000000005,7.03457692457189,22.4950538009022));
#58385=CARTESIAN_POINT('Ctrl Pts',(7.00000000000005,6.98764067308348,22.4318705980333));
#58386=CARTESIAN_POINT('Ctrl Pts',(6.99999999889749,6.94140041000313,22.3681993760895));
#58387=CARTESIAN_POINT('Ctrl Pts',(6.99999999756676,6.89586168253803,22.3040493688111));
#58388=CARTESIAN_POINT('Ctrl Pts',(6.99999999341046,6.75362945488333,22.1036880731148));
#58389=CARTESIAN_POINT('Ctrl Pts',(6.99999998911106,6.61823772701506,21.8986585551687));
#58390=CARTESIAN_POINT('Ctrl Pts',(6.99999999137286,6.48987017006242,21.6892961098581));
#58391=CARTESIAN_POINT('Ctrl Pts',(6.99999999340019,6.37480992104594,21.5016373613082));
#58392=CARTESIAN_POINT('Ctrl Pts',(7.00000000000005,6.26539334235283,21.3104967513935));
#58393=CARTESIAN_POINT('Ctrl Pts',(7.00000000000005,6.16178267245402,21.1160965407411));
#58394=CARTESIAN_POINT('Ctrl Pts',(7.00000000000005,6.10658746605843,21.0125361664979));
#58395=CARTESIAN_POINT('Ctrl Pts',(6.99999999798935,6.0530248573596,20.9080563407882));
#58396=CARTESIAN_POINT('Ctrl Pts',(6.99999999626516,6.00114000791266,20.8027233076497));
#58397=CARTESIAN_POINT('Ctrl Pts',(6.99999999250274,5.88792037752004,20.5728726439744));
#58398=CARTESIAN_POINT('Ctrl Pts',(6.99999999167263,5.78269282412516,20.3389576788273));
#58399=CARTESIAN_POINT('Ctrl Pts',(6.99999999476594,5.68575403995867,20.1017228715802));
#58400=CARTESIAN_POINT('Ctrl Pts',(6.99999999683534,5.6209025782142,19.943014216846));
#58401=CARTESIAN_POINT('Ctrl Pts',(7.00000000000005,5.55975985482664,19.7828203356804));
#58402=CARTESIAN_POINT('Ctrl Pts',(7.00000000000005,5.50240279152306,19.6213693832778));
#58403=CARTESIAN_POINT('Ctrl Pts',(7.00000000000005,5.45009099025049,19.4741200359279));
#58404=CARTESIAN_POINT('Ctrl Pts',(6.99999999705134,5.40094158554649,19.3258230175821));
#58405=CARTESIAN_POINT('Ctrl Pts',(6.99999999409828,5.35498665730465,19.1765629015957));
#58406=CARTESIAN_POINT('Ctrl Pts',(6.99999998947404,5.2830251860527,18.9428343776582));
#58407=CARTESIAN_POINT('Ctrl Pts',(6.99999998692731,5.21889427230412,18.7067443810182));
#58408=CARTESIAN_POINT('Ctrl Pts',(6.99999999182212,5.1627249648281,18.4686326355673));
#58409=CARTESIAN_POINT('Ctrl Pts',(6.99999999469964,5.12970466676817,18.3286536833662));
#58410=CARTESIAN_POINT('Ctrl Pts',(7.00000000000005,5.09943680476764,18.1879758874761));
#58411=CARTESIAN_POINT('Ctrl Pts',(7.00000000000005,5.07195641421797,18.0466678965669));
#58412=CARTESIAN_POINT('Ctrl Pts',(7.00000000000005,5.03480694334795,17.8556401496179));
#58413=CARTESIAN_POINT('Ctrl Pts',(6.99999998960188,5.00268470340247,17.6634616339159));
#58414=CARTESIAN_POINT('Ctrl Pts',(6.99999998461861,4.97570501838642,17.4706050373956));
#58415=CARTESIAN_POINT('Ctrl Pts',(6.99999997943762,4.94765482772354,17.2700962360598));
#58416=CARTESIAN_POINT('Ctrl Pts',(6.99999998080576,4.92516373828694,17.0688548847934));
#58417=CARTESIAN_POINT('Ctrl Pts',(6.99999998755707,4.90822419654875,16.8674168812407));
#58418=CARTESIAN_POINT('Ctrl Pts',(6.99999999250474,4.89581014344996,16.7197941113412));
#58419=CARTESIAN_POINT('Ctrl Pts',(7.00000000000005,4.88637652011908,16.5720658725087));
#58420=CARTESIAN_POINT('Ctrl Pts',(7.00000000000005,4.87990258513925,16.4244427931237));
#58421=CARTESIAN_POINT('Ctrl Pts',(7.00000000000005,4.87262550786042,16.2585059154486));
#58422=CARTESIAN_POINT('Ctrl Pts',(6.99999999328029,4.86916233836076,16.0927162210766));
#58423=CARTESIAN_POINT('Ctrl Pts',(6.99999999271624,4.86945768018416,15.9269562920536));
#58424=CARTESIAN_POINT('Ctrl Pts',(6.99999999249361,4.86957425256143,15.8615303095054));
#58425=CARTESIAN_POINT('Ctrl Pts',(6.99999999280638,4.87027693192223,15.7961088794921));
#58426=CARTESIAN_POINT('Ctrl Pts',(6.99999999341992,4.87156453058809,15.7306845305713));
#58427=CARTESIAN_POINT('Ctrl Pts',(6.99999999496892,4.87481533850375,15.5655072925178));
#58428=CARTESIAN_POINT('Ctrl Pts',(6.99999999795329,4.88179088200453,15.4003113655275));
#58429=CARTESIAN_POINT('Ctrl Pts',(6.99999999909603,4.89250690007613,15.2350111867318));
#58430=CARTESIAN_POINT('Ctrl Pts',(7.00000000010515,4.9019698574621,15.0890401238441));
#58431=CARTESIAN_POINT('Ctrl Pts',(6.99999999999946,4.91435036442321,14.9429875256047));
#58432=CARTESIAN_POINT('Ctrl Pts',(6.99999999999946,4.92969295105302,14.7967973165496));
#58433=CARTESIAN_POINT('',(6.2715946948284,8.76071067545968,25.5608579362149));
#58434=CARTESIAN_POINT('Origin',(5.999999877386,9.33250977407517,24.7867246592848));
#58435=CARTESIAN_POINT('',(6.263859499331,3.90573865723227,15.8144314043406));
#58436=CARTESIAN_POINT('Ctrl Pts',(6.27159470456883,8.76071047658687,25.5608577604478));
#58437=CARTESIAN_POINT('Ctrl Pts',(6.27193966898912,8.57412216343359,25.4228903957121));
#58438=CARTESIAN_POINT('Ctrl Pts',(6.27225782564642,8.39339832660335,25.280910240924));
#58439=CARTESIAN_POINT('Ctrl Pts',(6.27254917025225,8.21861683396742,25.1354918255172));
#58440=CARTESIAN_POINT('Ctrl Pts',(6.27284515814358,8.04104977277711,24.9877558136701));
#58441=CARTESIAN_POINT('Ctrl Pts',(6.273113472547,7.86961592067851,24.8364710622416));
#58442=CARTESIAN_POINT('Ctrl Pts',(6.27335410990005,7.70435956582304,24.6822006939131));
#58443=CARTESIAN_POINT('Ctrl Pts',(6.27354178806678,7.57547263564886,24.5618819672409));
#58444=CARTESIAN_POINT('Ctrl Pts',(6.27371263093874,7.4503425644811,24.4397463543931));
#58445=CARTESIAN_POINT('Ctrl Pts',(6.27386663718526,7.32897538003059,24.3160449569086));
#58446=CARTESIAN_POINT('Ctrl Pts',(6.27406868749697,7.16974627079252,24.1537534493471));
#58447=CARTESIAN_POINT('Ctrl Pts',(6.27424175784606,7.01699420978249,23.9887688320545));
#58448=CARTESIAN_POINT('Ctrl Pts',(6.27438584597958,6.87062082868007,23.8216790784536));
#58449=CARTESIAN_POINT('Ctrl Pts',(6.27447251908614,6.78257308076604,23.7211698438286));
#58450=CARTESIAN_POINT('Ctrl Pts',(6.27454870538725,6.69683289921858,23.6198979734037));
#58451=CARTESIAN_POINT('Ctrl Pts',(6.27461440453154,6.61337480174416,23.5179833665145));
#58452=CARTESIAN_POINT('Ctrl Pts',(6.27472591356408,6.47172407237543,23.3450070006969));
#58453=CARTESIAN_POINT('Ctrl Pts',(6.27480721202419,6.33664860500451,23.170181629431));
#58454=CARTESIAN_POINT('Ctrl Pts',(6.27485829885037,6.20800497223007,22.9940551814749));
#58455=CARTESIAN_POINT('Ctrl Pts',(6.27487121255017,6.17548650555785,22.9495340349212));
#58456=CARTESIAN_POINT('Ctrl Pts',(6.2748821958076,6.14337890295727,22.9049295182343));
#58457=CARTESIAN_POINT('Ctrl Pts',(6.27489124861356,6.11167962107519,22.8602500105962));
#58458=CARTESIAN_POINT('Ctrl Pts',(6.27492812667764,5.9825474874977,22.6782408354367));
#58459=CARTESIAN_POINT('Ctrl Pts',(6.27493296938054,5.86019259786137,22.4949912131483));
#58460=CARTESIAN_POINT('Ctrl Pts',(6.27490577665586,5.74438889409281,22.311044212034));
#58461=CARTESIAN_POINT('Ctrl Pts',(6.27488257757821,5.64559264810312,22.154112502773));
#58462=CARTESIAN_POINT('Ctrl Pts',(6.27483606184547,5.55156428911671,21.9966722845104));
#58463=CARTESIAN_POINT('Ctrl Pts',(6.2747662299236,5.46215434352605,21.8390322558468));
#58464=CARTESIAN_POINT('Ctrl Pts',(6.27472435194041,5.40853548128942,21.7444960280921));
#58465=CARTESIAN_POINT('Ctrl Pts',(6.27467408868735,5.35657741163384,21.6498874448625));
#58466=CARTESIAN_POINT('Ctrl Pts',(6.27461544167778,5.30624656452333,21.5552687339916));
#58467=CARTESIAN_POINT('Ctrl Pts',(6.27458611817299,5.28108114096807,21.5079593785561));
#58468=CARTESIAN_POINT('Ctrl Pts',(6.2745546960971,5.25632253120737,21.4606474869213));
#58469=CARTESIAN_POINT('Ctrl Pts',(6.27452117889509,5.23196642427779,21.4133404892521));
#58470=CARTESIAN_POINT('Ctrl Pts',(6.27450442029408,5.21978837081299,21.3896869904175));
#58471=CARTESIAN_POINT('Ctrl Pts',(6.27448713773378,5.20771094360307,21.3660347147777));
#58472=CARTESIAN_POINT('Ctrl Pts',(6.27446933121476,5.19573360226955,21.3423845802045));
#58473=CARTESIAN_POINT('Ctrl Pts',(6.27445391938858,5.18536702234589,21.3219150115889));
#58474=CARTESIAN_POINT('Ctrl Pts',(6.2744387297381,5.17546073754221,21.302217342206));
#58475=CARTESIAN_POINT('Ctrl Pts',(6.27442216601483,5.16501365433626,21.281292176439));
#58476=CARTESIAN_POINT('Ctrl Pts',(6.27441959233996,5.16339038430915,21.2780408196983));
#58477=CARTESIAN_POINT('Ctrl Pts',(6.27441698549086,5.16175414864423,21.2747597818786));
#58478=CARTESIAN_POINT('Ctrl Pts',(6.27441433947949,5.16010129477184,21.2714415111871));
#58479=CARTESIAN_POINT('Ctrl Pts',(6.27440279750611,5.15289150132369,21.2569671243763));
#58480=CARTESIAN_POINT('Ctrl Pts',(6.27439106570806,5.14570665026556,21.2424690495645));
#58481=CARTESIAN_POINT('Ctrl Pts',(6.27437914408635,5.13854692001712,21.2279473420534));
#58482=CARTESIAN_POINT('Ctrl Pts',(6.2742001112939,5.03102576804095,21.0098677963058));
#58483=CARTESIAN_POINT('Ctrl Pts',(6.27397826838863,4.92916789617758,20.7864547547487));
#58484=CARTESIAN_POINT('Ctrl Pts',(6.27371361964825,4.83351597227066,20.5579710708369));
#58485=CARTESIAN_POINT('Ctrl Pts',(6.27345239286638,4.73910084591757,20.3324417243792));
#58486=CARTESIAN_POINT('Ctrl Pts',(6.27314946005732,4.65073221455464,20.1019719667757));
#58487=CARTESIAN_POINT('Ctrl Pts',(6.27280482717338,4.56895654665535,19.8668588618551));
#58488=CARTESIAN_POINT('Ctrl Pts',(6.27260798328253,4.52224875585436,19.7325693598394));
#58489=CARTESIAN_POINT('Ctrl Pts',(6.27239753540531,4.47769227178865,19.5967658531892));
#58490=CARTESIAN_POINT('Ctrl Pts',(6.27217348494914,4.4353926019923,19.4595104126762));
#58491=CARTESIAN_POINT('Ctrl Pts',(6.27177013693201,4.35924239801633,19.2124155809151));
#58492=CARTESIAN_POINT('Ctrl Pts',(6.27132270389783,4.29040507220786,18.9606117357067));
#58493=CARTESIAN_POINT('Ctrl Pts',(6.27083119604893,4.22947047055946,18.7045320508306));
#58494=CARTESIAN_POINT('Ctrl Pts',(6.27036732538413,4.17196218409212,18.4628515691678));
#58495=CARTESIAN_POINT('Ctrl Pts',(6.26986419841394,4.12149304373649,18.217362945302));
#58496=CARTESIAN_POINT('Ctrl Pts',(6.26932182509284,4.07857892143672,17.9684782794355));
#58497=CARTESIAN_POINT('Ctrl Pts',(6.26905884935212,4.05777153165553,17.847803779394));
#58498=CARTESIAN_POINT('Ctrl Pts',(6.2687866472112,4.03874054889739,17.7263316145486));
#58499=CARTESIAN_POINT('Ctrl Pts',(6.26850522002609,4.02154646450729,17.6041128541433));
#58500=CARTESIAN_POINT('Ctrl Pts',(6.26791729738518,3.98562672385184,17.348788634639));
#58501=CARTESIAN_POINT('Ctrl Pts',(6.26728911425905,3.95772350439215,17.0902028081567));
#58502=CARTESIAN_POINT('Ctrl Pts',(6.26662068529587,3.93824701803358,16.8288403534343));
#58503=CARTESIAN_POINT('Ctrl Pts',(6.26595956850197,3.91898359151107,16.5703370305252));
#58504=CARTESIAN_POINT('Ctrl Pts',(6.26525908155454,3.90796355341187,16.3091174478807));
#58505=CARTESIAN_POINT('Ctrl Pts',(6.26451924198579,3.90559007207061,16.0457015126995));
#58506=CARTESIAN_POINT('Ctrl Pts',(6.2643032360479,3.90489710283129,15.9687937498052));
#58507=CARTESIAN_POINT('Ctrl Pts',(6.26408387561693,3.90494122833423,15.8916990992977));
#58508=CARTESIAN_POINT('Ctrl Pts',(6.26386116118917,3.90573258256842,15.8144313373355));
#58509=CARTESIAN_POINT('Ctrl Pts',(6.99999999999946,4.92969295105265,14.7967973165499));
#58510=CARTESIAN_POINT('Ctrl Pts',(7.00000003182991,4.89790687011507,14.8200962579317));
#58511=CARTESIAN_POINT('Ctrl Pts',(6.99872202620472,4.86684766352378,14.843151536839));
#58512=CARTESIAN_POINT('Ctrl Pts',(6.9963283798615,4.83663262564484,14.8659154105751));
#58513=CARTESIAN_POINT('Ctrl Pts',(6.99385186988673,4.80537159875714,14.8894673277293));
#58514=CARTESIAN_POINT('Ctrl Pts',(6.99018212459228,4.77501418352712,14.9127071669234));
#58515=CARTESIAN_POINT('Ctrl Pts',(6.98550026819671,4.74563468961346,14.9355742924579));
#58516=CARTESIAN_POINT('Ctrl Pts',(6.98072065912985,4.71564178004406,14.9589188616422));
#58517=CARTESIAN_POINT('Ctrl Pts',(6.97488710906418,4.68666762354792,14.98187480912));
#58518=CARTESIAN_POINT('Ctrl Pts',(6.96817910818256,4.65873797521076,15.0043722661871));
#58519=CARTESIAN_POINT('Ctrl Pts',(6.9612398354513,4.62984539595801,15.0276453684277));
#58520=CARTESIAN_POINT('Ctrl Pts',(6.95336553314029,4.6020700174534,15.0504276449154));
#58521=CARTESIAN_POINT('Ctrl Pts',(6.94472806264123,4.57539155224688,15.0726388605227));
#58522=CARTESIAN_POINT('Ctrl Pts',(6.94166914281976,4.56594349844046,15.0805048587553));
#58523=CARTESIAN_POINT('Ctrl Pts',(6.93851421614368,4.55663262766185,15.0882992220146));
#58524=CARTESIAN_POINT('Ctrl Pts',(6.93526991044448,4.54745686940672,15.096018363856));
#58525=CARTESIAN_POINT('Ctrl Pts',(6.92517489872626,4.51890549487626,15.1200373172373));
#58526=CARTESIAN_POINT('Ctrl Pts',(6.9142321383047,4.49170592042528,15.1433602032958));
#58527=CARTESIAN_POINT('Ctrl Pts',(6.90266739083218,4.46584896584675,15.1659445078881));
#58528=CARTESIAN_POINT('Ctrl Pts',(6.89228282415092,4.44263070970818,15.1862240874939));
#58529=CARTESIAN_POINT('Ctrl Pts',(6.88139666907031,4.42049387796962,15.2059080622683));
#58530=CARTESIAN_POINT('Ctrl Pts',(6.87015182633685,4.39940255498227,15.2249667510503));
#58531=CARTESIAN_POINT('Ctrl Pts',(6.85826800906539,4.37711274316933,15.2451084266866));
#58532=CARTESIAN_POINT('Ctrl Pts',(6.84598542356712,4.35599382686861,15.2645550463613));
#58533=CARTESIAN_POINT('Ctrl Pts',(6.83346225158623,4.33599910281022,15.2832873166577));
#58534=CARTESIAN_POINT('Ctrl Pts',(6.82720066559579,4.32600174078102,15.2926534518059));
#58535=CARTESIAN_POINT('Ctrl Pts',(6.82087870508477,4.31628525721843,15.3018411349062));
#58536=CARTESIAN_POINT('Ctrl Pts',(6.81451474301598,4.30684284344094,15.3108487116038));
#58537=CARTESIAN_POINT('Ctrl Pts',(6.81133276198159,4.30212163655219,15.3153524999526));
#58538=CARTESIAN_POINT('Ctrl Pts',(6.80814027492826,4.29746895059205,15.3198112619028));
#58539=CARTESIAN_POINT('Ctrl Pts',(6.80493947884344,4.29288386412139,15.3242248417572));
#58540=CARTESIAN_POINT('Ctrl Pts',(6.80333908080103,4.29059132088605,15.3264316316844));
#58541=CARTESIAN_POINT('Ctrl Pts',(6.80173660508477,4.28831567774204,15.3286271261022));
#58542=CARTESIAN_POINT('Ctrl Pts',(6.80013232216023,4.28605681842174,15.3308113069044));
#58543=CARTESIAN_POINT('Ctrl Pts',(6.79874993359117,4.28411039035989,15.3326933855126));
#58544=CARTESIAN_POINT('Ctrl Pts',(6.79775798456452,4.28272134681384,15.3340389472113));
#58545=CARTESIAN_POINT('Ctrl Pts',(6.79614408876686,4.28048077370916,15.3362131510563));
#58546=CARTESIAN_POINT('Ctrl Pts',(6.79588503398598,4.28012112770504,15.3365621437865));
#58547=CARTESIAN_POINT('Ctrl Pts',(6.79560987565501,4.27973960727994,15.3369325016948));
#58548=CARTESIAN_POINT('Ctrl Pts',(6.79531431958812,4.27933047508902,15.337329891204));
#58549=CARTESIAN_POINT('Ctrl Pts',(6.76951420699996,4.24361590932029,15.3720193976253));
#58550=CARTESIAN_POINT('Ctrl Pts',(6.74173255827647,4.21000266490947,15.4059751937068));
#58551=CARTESIAN_POINT('Ctrl Pts',(6.71227734444122,4.17864917320428,15.439110835369));
#58552=CARTESIAN_POINT('Ctrl Pts',(6.68190104901643,4.14631523966156,15.4732826477296));
#58553=CARTESIAN_POINT('Ctrl Pts',(6.64974534687681,4.11638416653758,15.5065819374885));
#58554=CARTESIAN_POINT('Ctrl Pts',(6.6161493421093,4.08897088661842,15.5389140150329));
#58555=CARTESIAN_POINT('Ctrl Pts',(6.58093661722554,4.06023841409273,15.572801989492));
#58556=CARTESIAN_POINT('Ctrl Pts',(6.54414181559471,4.03427162417726,15.6056271410108));
#58557=CARTESIAN_POINT('Ctrl Pts',(6.50615167047959,4.01114470028624,15.6372849612645));
#58558=CARTESIAN_POINT('Ctrl Pts',(6.4749471911299,3.99214862599401,15.6632881732915));
#58559=CARTESIAN_POINT('Ctrl Pts',(6.44293613655435,3.975067367133,15.6885038655809));
#58560=CARTESIAN_POINT('Ctrl Pts',(6.41033062344876,3.95991630293878,15.7128780676492));
#58561=CARTESIAN_POINT('Ctrl Pts',(6.36985327840053,3.94110737172364,15.7431368457949));
#58562=CARTESIAN_POINT('Ctrl Pts',(6.32845982679951,3.92527454314398,15.7720983393468));
#58563=CARTESIAN_POINT('Ctrl Pts',(6.28655299478072,3.91240124871222,15.7996692510339));
#58564=CARTESIAN_POINT('Ctrl Pts',(6.27900493180689,3.91008257100812,15.8046351949537));
#58565=CARTESIAN_POINT('Ctrl Pts',(6.27144020631059,3.90785977293139,15.8095560578491));
#58566=CARTESIAN_POINT('Ctrl Pts',(6.26386116118917,3.90573258256842,15.8144313373355));
#58567=CARTESIAN_POINT('Ctrl Pts',(7.10569404143661,5.09054165125083,15.2151876877299));
#58568=CARTESIAN_POINT('Ctrl Pts',(7.10698751687283,5.00269310760996,15.2441266563576));
#58569=CARTESIAN_POINT('Ctrl Pts',(7.0902945199642,4.80945364231557,15.312718885045));
#58570=CARTESIAN_POINT('Ctrl Pts',(6.99969996992157,4.52705209321443,15.4294190158596));
#58571=CARTESIAN_POINT('Ctrl Pts',(6.83798590956392,4.26863790102804,15.5561021331105));
#58572=CARTESIAN_POINT('Ctrl Pts',(6.62407657918662,4.06622759758902,15.6779599862762));
#58573=CARTESIAN_POINT('Ctrl Pts',(6.41886258694164,3.95388203420082,15.7685510741009));
#58574=CARTESIAN_POINT('Ctrl Pts',(6.29029260882867,3.91233292862259,15.8162139975417));
#58575=CARTESIAN_POINT('Ctrl Pts',(6.24978854300632,3.9018220331908,15.8304216839861));
#58576=CARTESIAN_POINT('Ctrl Pts',(6.81662658173112,4.90577014638609,14.6682465297021));
#58577=CARTESIAN_POINT('Ctrl Pts',(6.81778595104908,4.82838688483558,14.6937210486444));
#58578=CARTESIAN_POINT('Ctrl Pts',(6.80279186069882,4.65778890045996,14.754496390137));
#58579=CARTESIAN_POINT('Ctrl Pts',(6.72115173917901,4.4083902191048,14.8587571478518));
#58580=CARTESIAN_POINT('Ctrl Pts',(6.57567845311055,4.18091900980098,14.9723280494875));
#58581=CARTESIAN_POINT('Ctrl Pts',(6.384034670463,4.00376978964618,15.081523231443));
#58582=CARTESIAN_POINT('Ctrl Pts',(6.20121810832221,3.9062350109221,15.1623974452969));
#58583=CARTESIAN_POINT('Ctrl Pts',(6.08727994870383,3.87041481062267,15.204739989342));
#58584=CARTESIAN_POINT('Ctrl Pts',(6.05144712941405,3.86137576219619,15.2173393578419));
#58585=CARTESIAN_POINT('Ctrl Pts',(7.05823304509093,4.72145803038867,14.0984567957104));
#58586=CARTESIAN_POINT('Ctrl Pts',(7.05976380412154,4.62141948135273,14.1314134593268));
#58587=CARTESIAN_POINT('Ctrl Pts',(7.04010452168148,4.40252217185232,14.2090883142289));
#58588=CARTESIAN_POINT('Ctrl Pts',(6.93421353969746,4.08329669950976,14.3408115984512));
#58589=CARTESIAN_POINT('Ctrl Pts',(6.7444197293285,3.78963037230628,14.4845606457827));
#58590=CARTESIAN_POINT('Ctrl Pts',(6.4910049093302,3.55726100403775,14.6244807199787));
#58591=CARTESIAN_POINT('Ctrl Pts',(6.24476176461835,3.4265307786445,14.7303629781109));
#58592=CARTESIAN_POINT('Ctrl Pts',(6.08867719634714,3.37773039761847,14.7870387478717));
#58593=CARTESIAN_POINT('Ctrl Pts',(6.0393188304862,3.36535861577285,14.8040347283816));
#58594=CARTESIAN_POINT('Ctrl Pts',(7.66731039910081,4.66246517745525,13.8917937410857));
#58595=CARTESIAN_POINT('Ctrl Pts',(7.66946689865306,4.52196894416207,13.9381201648513));
#58596=CARTESIAN_POINT('Ctrl Pts',(7.64193305760113,4.21648837384924,14.0459844860487));
#58597=CARTESIAN_POINT('Ctrl Pts',(7.49498492088685,3.77181855920877,14.2265034331141));
#58598=CARTESIAN_POINT('Ctrl Pts',(7.23027996478551,3.35957593531508,14.423315567559));
#58599=CARTESIAN_POINT('Ctrl Pts',(6.87282901199206,3.02884202226372,14.6165723783504));
#58600=CARTESIAN_POINT('Ctrl Pts',(6.52022670404055,2.83935539051515,14.7652770063116));
#58601=CARTESIAN_POINT('Ctrl Pts',(6.29371870310657,2.76764241383735,14.8462471717371));
#58602=CARTESIAN_POINT('Ctrl Pts',(6.22178457189615,2.74938677633292,14.8706715897612));
#58603=CARTESIAN_POINT('',(6.24994594247521,2.765465712864,14.8593875553346));
#58604=CARTESIAN_POINT('Ctrl Pts',(6.26385699586341,3.90574781113883,15.8144315048343));
#58605=CARTESIAN_POINT('Ctrl Pts',(6.25434798380003,3.90347005541746,15.7850252855376));
#58606=CARTESIAN_POINT('Ctrl Pts',(6.24501496153337,3.89975208452744,15.7549930856709));
#58607=CARTESIAN_POINT('Ctrl Pts',(6.23596108667827,3.89444439028301,15.7245073673137));
#58608=CARTESIAN_POINT('Ctrl Pts',(6.22713383888874,3.88926955265422,15.6947847353702));
#58609=CARTESIAN_POINT('Ctrl Pts',(6.21857222852935,3.88258290074168,15.6646313129789));
#58610=CARTESIAN_POINT('Ctrl Pts',(6.21037775698272,3.87427382466893,15.6342471001828));
#58611=CARTESIAN_POINT('Ctrl Pts',(6.20230962221974,3.8660928522744,15.6043313304947));
#58612=CARTESIAN_POINT('Ctrl Pts',(6.19459771432488,3.85633847793405,15.5741922828855));
#58613=CARTESIAN_POINT('Ctrl Pts',(6.18734021170931,3.84494221012623,15.5440547858302));
#58614=CARTESIAN_POINT('Ctrl Pts',(6.18021026865726,3.83374624578704,15.5144469924724));
#58615=CARTESIAN_POINT('Ctrl Pts',(6.17351923089785,3.82096516393263,15.4848413319623));
#58616=CARTESIAN_POINT('Ctrl Pts',(6.16735661573876,3.80657784168717,15.455475932425));
#58617=CARTESIAN_POINT('Ctrl Pts',(6.1665592055774,3.80471619745706,15.4516762033523));
#58618=CARTESIAN_POINT('Ctrl Pts',(6.16577063373331,3.80282772589229,15.4478805235924));
#58619=CARTESIAN_POINT('Ctrl Pts',(6.16499108510522,3.80091244122259,15.4440894309064));
#58620=CARTESIAN_POINT('Ctrl Pts',(6.15905868185249,3.78633703104931,15.415239029827));
#58621=CARTESIAN_POINT('Ctrl Pts',(6.15364986165422,3.77020476525735,15.3866536317792));
#58622=CARTESIAN_POINT('Ctrl Pts',(6.14883921111318,3.75254960135707,15.3585762389554));
#58623=CARTESIAN_POINT('Ctrl Pts',(6.14409019033999,3.7351206196838,15.3308585486681));
#58624=CARTESIAN_POINT('Ctrl Pts',(6.1399243836778,3.716207531236,15.3036367366627));
#58625=CARTESIAN_POINT('Ctrl Pts',(6.13640028093367,3.69589197713741,15.2771455138267));
#58626=CARTESIAN_POINT('Ctrl Pts',(6.13289687262579,3.67569572118926,15.2508098542537));
#58627=CARTESIAN_POINT('Ctrl Pts',(6.1300278736233,3.65411363410035,15.2251970341261));
#58628=CARTESIAN_POINT('Ctrl Pts',(6.12783385014554,3.63127298396052,15.2005265382343));
#58629=CARTESIAN_POINT('Ctrl Pts',(6.1256472714576,3.60850983702044,15.1759397545994));
#58630=CARTESIAN_POINT('Ctrl Pts',(6.12413123414268,3.58449708246778,15.1522896565134));
#58631=CARTESIAN_POINT('Ctrl Pts',(6.1233063543654,3.55940279460655,15.1297707718731));
#58632=CARTESIAN_POINT('Ctrl Pts',(6.12248221725878,3.53433110008748,15.1072721618415));
#58633=CARTESIAN_POINT('Ctrl Pts',(6.12234803831525,3.50818043438343,15.0859033522775));
#58634=CARTESIAN_POINT('Ctrl Pts',(6.12290344669521,3.48115267077958,15.0658252908192));
#58635=CARTESIAN_POINT('Ctrl Pts',(6.12346156137084,3.45399321107174,15.0456493965359));
#58636=CARTESIAN_POINT('Ctrl Pts',(6.12471595661025,3.42594883438446,15.0267773356849));
#58637=CARTESIAN_POINT('Ctrl Pts',(6.12664506630351,3.39724869516408,15.0093306421183));
#58638=CARTESIAN_POINT('Ctrl Pts',(6.12858163947937,3.36843751871722,14.99181644949));
#58639=CARTESIAN_POINT('Ctrl Pts',(6.13119800640248,3.33896633964887,14.9757389134287));
#58640=CARTESIAN_POINT('Ctrl Pts',(6.1344525305991,3.3090793273335,14.9611735632068));
#58641=CARTESIAN_POINT('Ctrl Pts',(6.13774444965242,3.27884890981502,14.9464408554384));
#58642=CARTESIAN_POINT('Ctrl Pts',(6.14168905204685,3.24819391461928,14.9332553333186));
#58643=CARTESIAN_POINT('Ctrl Pts',(6.14622583015071,3.21736659817575,14.9216444301484));
#58644=CARTESIAN_POINT('Ctrl Pts',(6.14953012183543,3.19491400229062,14.9131878096306));
#58645=CARTESIAN_POINT('Ctrl Pts',(6.1531481575373,3.17237001510414,14.9055653725594));
#58646=CARTESIAN_POINT('Ctrl Pts',(6.15705202271518,3.14982812311891,14.8987714044217));
#58647=CARTESIAN_POINT('Ctrl Pts',(6.1625076467821,3.11832598797211,14.8892768818413));
#58648=CARTESIAN_POINT('Ctrl Pts',(6.1685214499985,3.08682925243436,14.8814020376996));
#58649=CARTESIAN_POINT('Ctrl Pts',(6.17500783915478,3.05557312923402,14.8750910675516));
#58650=CARTESIAN_POINT('Ctrl Pts',(6.18164262016742,3.02360194654021,14.8686357186816));
#58651=CARTESIAN_POINT('Ctrl Pts',(6.18877150533514,2.99188314996284,14.863816109299));
#58652=CARTESIAN_POINT('Ctrl Pts',(6.19629722070769,2.96063494824442,14.8605298222474));
#58653=CARTESIAN_POINT('Ctrl Pts',(6.20393441429794,2.92892386776148,14.8571948555148));
#58654=CARTESIAN_POINT('Ctrl Pts',(6.21197992740394,2.89769780882519,14.85543825752));
#58655=CARTESIAN_POINT('Ctrl Pts',(6.22033178841968,2.86714287327628,14.8551190429553));
#58656=CARTESIAN_POINT('Ctrl Pts',(6.22888396322111,2.83585509808839,14.8547921722434));
#58657=CARTESIAN_POINT('Ctrl Pts',(6.23775702918233,2.80527124043204,14.8559716889506));
#58658=CARTESIAN_POINT('Ctrl Pts',(6.24684646258028,2.7755427257783,14.8584823292218));
#58659=CARTESIAN_POINT('Ctrl Pts',(6.24787684252207,2.77217269556219,14.8587669358923));
#58660=CARTESIAN_POINT('Ctrl Pts',(6.2489100109869,2.76881360546945,14.859068630846));
#58661=CARTESIAN_POINT('Ctrl Pts',(6.24994582233798,2.76546563683757,14.8593871468619));
#58662=CARTESIAN_POINT('',(6.99999997823011,3.16613311195312,14.5427407175274));
#58663=CARTESIAN_POINT('Ctrl Pts',(6.99999993220815,3.16613252794448,14.5427396600064));
#58664=CARTESIAN_POINT('Ctrl Pts',(6.96231762727278,3.13329554641419,14.5625135410054));
#58665=CARTESIAN_POINT('Ctrl Pts',(6.92360816603438,3.10217170226233,14.5820110124235));
#58666=CARTESIAN_POINT('Ctrl Pts',(6.88387823383206,3.07270488837879,14.6012599053988));
#58667=CARTESIAN_POINT('Ctrl Pts',(6.87356165203147,3.065053307342,14.6062582219814));
#58668=CARTESIAN_POINT('Ctrl Pts',(6.86317604426154,3.05751362050396,14.6112397769873));
#58669=CARTESIAN_POINT('Ctrl Pts',(6.8527210844064,3.05008520711899,14.6162050497553));
#58670=CARTESIAN_POINT('Ctrl Pts',(6.82600907014904,3.0311059009334,14.6288911278282));
#58671=CARTESIAN_POINT('Ctrl Pts',(6.79884483386461,3.0128524446524,14.641470956376));
#58672=CARTESIAN_POINT('Ctrl Pts',(6.77122670154749,2.99531605711247,14.6539509876441));
#58673=CARTESIAN_POINT('Ctrl Pts',(6.70346621716213,2.95229091332536,14.6845704717628));
#58674=CARTESIAN_POINT('Ctrl Pts',(6.63297634616849,2.91356612828382,14.7145915227367));
#58675=CARTESIAN_POINT('Ctrl Pts',(6.56020276160944,2.87939117496359,14.7438671099234));
#58676=CARTESIAN_POINT('Ctrl Pts',(6.54699691805475,2.87318962408809,14.7491795983311));
#58677=CARTESIAN_POINT('Ctrl Pts',(6.53371574536084,2.8671379488153,14.7544675514922));
#58678=CARTESIAN_POINT('Ctrl Pts',(6.52036174280708,2.86123771480371,14.7597301048116));
#58679=CARTESIAN_POINT('Ctrl Pts',(6.4904965666444,2.84804230560353,14.7714993913094));
#58680=CARTESIAN_POINT('Ctrl Pts',(6.46026959312842,2.83560758267573,14.7831403452059));
#58681=CARTESIAN_POINT('Ctrl Pts',(6.42966397675873,2.82393755775448,14.7946591670874));
#58682=CARTESIAN_POINT('Ctrl Pts',(6.38476129492752,2.80681601347085,14.8115588755516));
#58683=CARTESIAN_POINT('Ctrl Pts',(6.33904417176279,2.79133823120731,14.8281961702507));
#58684=CARTESIAN_POINT('Ctrl Pts',(6.2924722492654,2.77753576511219,14.8445798018293));
#58685=CARTESIAN_POINT('Ctrl Pts',(6.27837566303401,2.77335797636992,14.8495388686436));
#58686=CARTESIAN_POINT('Ctrl Pts',(6.26420064751584,2.76933401082123,14.8544746304912));
#58687=CARTESIAN_POINT('Ctrl Pts',(6.24994582233798,2.76546563683757,14.8593871468619));
#58688=CARTESIAN_POINT('Ctrl Pts',(7.,4.9296929510512,14.7967973165494));
#58689=CARTESIAN_POINT('Ctrl Pts',(7.,4.79879097364903,14.7447999429358));
#58690=CARTESIAN_POINT('Ctrl Pts',(7.,4.67469316982841,14.7000467303213));
#58691=CARTESIAN_POINT('Ctrl Pts',(7.,4.55739953958936,14.6625376787058));
#58692=CARTESIAN_POINT('Ctrl Pts',(7.,4.51830166284301,14.6500346615006));
#58693=CARTESIAN_POINT('Ctrl Pts',(7.,4.4820605631409,14.6389453969358));
#58694=CARTESIAN_POINT('Ctrl Pts',(7.,4.44237396721083,14.6274433474232));
#58695=CARTESIAN_POINT('Ctrl Pts',(7.,4.28362758349054,14.5814351493728));
#58696=CARTESIAN_POINT('Ctrl Pts',(7.,4.12819843211269,14.5472955039941));
#58697=CARTESIAN_POINT('Ctrl Pts',(7.,3.9812641135579,14.5257824769341));
#58698=CARTESIAN_POINT('Ctrl Pts',(7.,3.68739547644833,14.4827564228141));
#58699=CARTESIAN_POINT('Ctrl Pts',(7.,3.41568526058562,14.488409179345));
#58700=CARTESIAN_POINT('Ctrl Pts',(7.,3.16613346596978,14.5427407465266));
#58701=CARTESIAN_POINT('Ctrl Pts',(6.38289431678474,3.93904937645538,15.7741367696646));
#58702=CARTESIAN_POINT('Ctrl Pts',(6.33037402857394,3.92420127911889,15.7930335494319));
#58703=CARTESIAN_POINT('Ctrl Pts',(5.6967036132714,3.74727551077352,16.0176262814828));
#58704=CARTESIAN_POINT('Ctrl Pts',(4.3653537707354,3.43062433292629,16.4060367717622));
#58705=CARTESIAN_POINT('Ctrl Pts',(2.27852928213159,3.11272070634599,16.7768273765144));
#58706=CARTESIAN_POINT('Ctrl Pts',(0.00160600171922482,2.99217538455127,
16.9128348891133));
#58707=CARTESIAN_POINT('Ctrl Pts',(-2.27556282787673,3.11240056823132,16.777192259624));
#58708=CARTESIAN_POINT('Ctrl Pts',(-4.36295887685328,3.43014050386403,16.4066150670817));
#58709=CARTESIAN_POINT('Ctrl Pts',(-5.6953528158905,3.74692061286735,16.0180709627932));
#58710=CARTESIAN_POINT('Ctrl Pts',(-6.32980048790067,3.9240391095482,15.7932399281334));
#58711=CARTESIAN_POINT('Ctrl Pts',(-6.3828984100613,3.93905052008556,15.7741353000131));
#58712=CARTESIAN_POINT('Ctrl Pts',(6.18023342351759,3.89116773501399,15.1627904562897));
#58713=CARTESIAN_POINT('Ctrl Pts',(6.12935373465988,3.87698876809142,15.1810909844233));
#58714=CARTESIAN_POINT('Ctrl Pts',(5.5154849218392,3.70803107728603,15.3985987917746));
#58715=CARTESIAN_POINT('Ctrl Pts',(4.22593147396741,3.40552953667279,15.7747860843702));
#58716=CARTESIAN_POINT('Ctrl Pts',(2.2054008109767,3.10176244037637,16.1338745651197));
#58717=CARTESIAN_POINT('Ctrl Pts',(0.00155433447093668,2.98658018383598,
16.2655671789925));
#58718=CARTESIAN_POINT('Ctrl Pts',(-2.20252913753767,3.10145653633292,16.1342278953521));
#58719=CARTESIAN_POINT('Ctrl Pts',(-4.22361213522192,3.40506724930268,15.7753461730261));
#58720=CARTESIAN_POINT('Ctrl Pts',(-5.51417640650268,3.70769210772978,15.3990294647388));
#58721=CARTESIAN_POINT('Ctrl Pts',(-6.12879810980744,3.87683390721015,15.1812908509248));
#58722=CARTESIAN_POINT('Ctrl Pts',(-6.18023738901782,3.89116882781119,15.1627890325264));
#58723=CARTESIAN_POINT('Ctrl Pts',(6.17613448039233,3.39302982546975,14.7530757616085));
#58724=CARTESIAN_POINT('Ctrl Pts',(6.12540401856028,3.379030795255,14.77115610782));
#58725=CARTESIAN_POINT('Ctrl Pts',(5.51330412368829,3.2122020990137,14.9860629206928));
#58726=CARTESIAN_POINT('Ctrl Pts',(4.22664027251003,2.91314014013688,15.3581450830883));
#58727=CARTESIAN_POINT('Ctrl Pts',(2.20729613110763,2.61210322269024,15.7140461237668));
#58728=CARTESIAN_POINT('Ctrl Pts',(0.00155619864217923,2.49773465424207,
15.8447871362558));
#58729=CARTESIAN_POINT('Ctrl Pts',(-2.20442381705102,2.61179967411732,15.7143967100113));
#58730=CARTESIAN_POINT('Ctrl Pts',(-4.22432454682835,2.91268259313759,15.3586995966211));
#58731=CARTESIAN_POINT('Ctrl Pts',(-5.51199907533185,3.21186725438272,14.9864886029628));
#58732=CARTESIAN_POINT('Ctrl Pts',(-6.12485002384382,3.37887789813221,14.7713535689273));
#58733=CARTESIAN_POINT('Ctrl Pts',(-6.17613843389023,3.39303090233569,14.753074354535));
#58734=CARTESIAN_POINT('Ctrl Pts',(6.37215938761968,2.78307364974066,14.8198971917583));
#58735=CARTESIAN_POINT('Ctrl Pts',(6.3199952273895,2.76864705353836,14.8382795416226));
#58736=CARTESIAN_POINT('Ctrl Pts',(5.69054844857231,2.59670875603571,15.056795096808));
#58737=CARTESIAN_POINT('Ctrl Pts',(4.36615521637009,2.28812300275669,15.435607729357));
#58738=CARTESIAN_POINT('Ctrl Pts',(2.2824842989152,1.97663889786705,15.7989326795465));
#58739=CARTESIAN_POINT('Ctrl Pts',(0.00161001422916566,1.85801376889573,
15.9327063761786));
#58740=CARTESIAN_POINT('Ctrl Pts',(-2.27951693148397,1.97632431053655,15.7992911267141));
#58741=CARTESIAN_POINT('Ctrl Pts',(-4.36376916166503,2.28765030166368,15.43617298023));
#58742=CARTESIAN_POINT('Ctrl Pts',(-5.68920595027655,2.59636352431106,15.0572281149511));
#58743=CARTESIAN_POINT('Ctrl Pts',(-6.31942557697566,2.76848948409855,14.8384803004125));
#58744=CARTESIAN_POINT('Ctrl Pts',(-6.37216345227932,2.78307475611255,14.8198957610868));
#58745=CARTESIAN_POINT('',(-6.26386065629335,3.90573732468848,15.8144217481535));
#58746=CARTESIAN_POINT('',(-6.249946130096,2.76546781932625,14.8593870899707));
#58747=CARTESIAN_POINT('Ctrl Pts',(-6.26386066455461,3.90573729438309,15.8144217478187));
#58748=CARTESIAN_POINT('Ctrl Pts',(-6.25434831141213,3.90345828807139,15.7850176820746));
#58749=CARTESIAN_POINT('Ctrl Pts',(-6.24501346021768,3.89973955504434,15.754986953564));
#58750=CARTESIAN_POINT('Ctrl Pts',(-6.23595867491624,3.89443139082405,15.724502287951));
#58751=CARTESIAN_POINT('Ctrl Pts',(-6.22713146317302,3.88925663648362,15.6947837922242));
#58752=CARTESIAN_POINT('Ctrl Pts',(-6.21857071083251,3.8825706633106,15.6646341979587));
#58753=CARTESIAN_POINT('Ctrl Pts',(-6.21037751462733,3.87426278352997,15.634253634215));
#58754=CARTESIAN_POINT('Ctrl Pts',(-6.20231060850718,3.86608296156923,15.6043413570694));
#58755=CARTESIAN_POINT('Ctrl Pts',(-6.19460034139449,3.85633023035241,15.5742056254424));
#58756=CARTESIAN_POINT('Ctrl Pts',(-6.18734460751122,3.844936061604,15.5440713466953));
#58757=CARTESIAN_POINT('Ctrl Pts',(-6.18021636223641,3.83374209682414,15.5144665495039));
#58758=CARTESIAN_POINT('Ctrl Pts',(-6.17352715644783,3.82096343865695,15.4848637891835));
#58759=CARTESIAN_POINT('Ctrl Pts',(-6.16736625649837,3.80657894180169,15.4555012511846));
#58760=CARTESIAN_POINT('Ctrl Pts',(-6.16656710070447,3.80471306926708,15.4516925150328));
#58761=CARTESIAN_POINT('Ctrl Pts',(-6.16577682489813,3.80282024355606,15.4478878475468));
#58762=CARTESIAN_POINT('Ctrl Pts',(-6.16499561473955,3.8009004789636,15.4440877906076));
#58763=CARTESIAN_POINT('Ctrl Pts',(-6.15906452005692,3.78632526454647,15.4152370424981));
#58764=CARTESIAN_POINT('Ctrl Pts',(-6.15365690109852,3.77019315686551,15.3866513455472));
#58765=CARTESIAN_POINT('Ctrl Pts',(-6.14884735387733,3.75253811793426,15.3585736969602));
#58766=CARTESIAN_POINT('Ctrl Pts',(-6.1440994216987,3.73510925746118,15.3308557507387));
#58767=CARTESIAN_POINT('Ctrl Pts',(-6.13993460837156,3.71619625756151,15.3036337249475));
#58768=CARTESIAN_POINT('Ctrl Pts',(-6.1364114164295,3.69588076477368,15.2771423239223));
#58769=CARTESIAN_POINT('Ctrl Pts',(-6.1329089125532,3.67568456388303,15.2508064795219));
#58770=CARTESIAN_POINT('Ctrl Pts',(-6.13004073682332,3.65410250414156,15.2251935101448));
#58771=CARTESIAN_POINT('Ctrl Pts',(-6.12784747118893,3.63126185987898,15.2005228928044));
#58772=CARTESIAN_POINT('Ctrl Pts',(-6.12566164681365,3.60849870880713,15.1759359773436));
#58773=CARTESIAN_POINT('Ctrl Pts',(-6.12414629946667,3.58448592772055,15.1522857758375));
#58774=CARTESIAN_POINT('Ctrl Pts',(-6.12332206340787,3.55939159786993,15.1297668076039));
#58775=CARTESIAN_POINT('Ctrl Pts',(-6.12249856901549,3.53431984847043,15.1072681024522));
#58776=CARTESIAN_POINT('Ctrl Pts',(-6.12236498739556,3.50816911136713,15.0858992186932));
#58777=CARTESIAN_POINT('Ctrl Pts',(-6.12292096736125,3.48114126735242,15.0658210949586));
#58778=CARTESIAN_POINT('Ctrl Pts',(-6.12347965668713,3.45398171325965,15.0456451280056));
#58779=CARTESIAN_POINT('Ctrl Pts',(-6.12473460135381,3.42593723222674,15.0267730077924));
#58780=CARTESIAN_POINT('Ctrl Pts',(-6.1266642557543,3.39723698661223,15.0093262589561));
#58781=CARTESIAN_POINT('Ctrl Pts',(-6.12860137628395,3.36842569534072,14.9918120059699));
#58782=CARTESIAN_POINT('Ctrl Pts',(-6.13121828625185,3.33895439904086,14.9757344144424));
#58783=CARTESIAN_POINT('Ctrl Pts',(-6.13447336941178,3.30906727489292,14.9611690045746));
#58784=CARTESIAN_POINT('Ctrl Pts',(-6.13776585195478,3.27883676166707,14.9464362449598));
#58785=CARTESIAN_POINT('Ctrl Pts',(-6.1417110334367,3.24818167679902,14.9332506648979));
#58786=CARTESIAN_POINT('Ctrl Pts',(-6.14624842574256,3.2173542835874,14.9216396889257));
#58787=CARTESIAN_POINT('Ctrl Pts',(-6.14955235103642,3.19490716036996,14.9131850976946));
#58788=CARTESIAN_POINT('Ctrl Pts',(-6.15316988431773,3.17236869747348,14.9055642707548));
#58789=CARTESIAN_POINT('Ctrl Pts',(-6.15707313882021,3.14983231529049,14.8987714964257));
#58790=CARTESIAN_POINT('Ctrl Pts',(-6.16252922916163,3.11833026051006,14.8892763455498));
#58791=CARTESIAN_POINT('Ctrl Pts',(-6.1685437480149,3.08683362732814,14.881400776874));
#58792=CARTESIAN_POINT('Ctrl Pts',(-6.1750305166369,3.05557747107911,14.8750891980218));
#58793=CARTESIAN_POINT('Ctrl Pts',(-6.18166567463506,3.02360630836121,14.8686332373822));
#58794=CARTESIAN_POINT('Ctrl Pts',(-6.18879458347136,2.99188738929926,14.8638131319262));
#58795=CARTESIAN_POINT('Ctrl Pts',(-6.19631949447585,2.96063879745935,14.8605266373239));
#58796=CARTESIAN_POINT('Ctrl Pts',(-6.20395586199788,2.9289273617104,14.8571914642398));
#58797=CARTESIAN_POINT('Ctrl Pts',(-6.21199969621026,2.89770067096357,14.8554349526722));
#58798=CARTESIAN_POINT('Ctrl Pts',(-6.22034867567113,2.86714473778872,14.8551162453579));
#58799=CARTESIAN_POINT('Ctrl Pts',(-6.22889787688057,2.83585602494922,14.8547898949376));
#58800=CARTESIAN_POINT('Ctrl Pts',(-6.23776670786458,2.80527084272535,14.8559703646471));
#58801=CARTESIAN_POINT('Ctrl Pts',(-6.24685040422301,2.77554055782156,14.8584824801066));
#58802=CARTESIAN_POINT('Ctrl Pts',(-6.24787961953862,2.77217201011222,14.8587671117811));
#58803=CARTESIAN_POINT('Ctrl Pts',(-6.24891160143422,2.76881438591469,14.8590688213317));
#58804=CARTESIAN_POINT('Ctrl Pts',(-6.24994620423252,2.76546786623744,14.8593873420339));
#58805=CARTESIAN_POINT('Ctrl Pts',(6.24994601128656,2.76546575640966,14.8593877892967));
#58806=CARTESIAN_POINT('Ctrl Pts',(6.23688268274706,2.76192003125581,14.8638898479677));
#58807=CARTESIAN_POINT('Ctrl Pts',(6.22381281177066,2.758383592908,14.8683771686433));
#58808=CARTESIAN_POINT('Ctrl Pts',(6.21073642273195,2.75485647619773,14.8728497532653));
#58809=CARTESIAN_POINT('Ctrl Pts',(5.89583157450962,2.66991665458339,14.9805582787141));
#58810=CARTESIAN_POINT('Ctrl Pts',(5.57714884580729,2.59038142383472,15.0797242785993));
#58811=CARTESIAN_POINT('Ctrl Pts',(5.25507847391284,2.51679039840292,15.1703536776165));
#58812=CARTESIAN_POINT('Ctrl Pts',(5.12540270308979,2.48716031199542,15.2068439549048));
#58813=CARTESIAN_POINT('Ctrl Pts',(4.99517746302832,2.4584940523232,15.2419498660761));
#58814=CARTESIAN_POINT('Ctrl Pts',(4.86442719004076,2.430827743042,15.2756698507746));
#58815=CARTESIAN_POINT('Ctrl Pts',(4.72158141783862,2.40060206761544,15.3125092174759));
#58816=CARTESIAN_POINT('Ctrl Pts',(4.57811215030979,2.37156574348657,15.3476943597705));
#58817=CARTESIAN_POINT('Ctrl Pts',(4.43405184968593,2.3437574901839,15.3812229418945));
#58818=CARTESIAN_POINT('Ctrl Pts',(4.34163140552557,2.32591738357279,15.4027328682138));
#58819=CARTESIAN_POINT('Ctrl Pts',(4.2489676810377,2.30858273346186,15.4235609671336));
#58820=CARTESIAN_POINT('Ctrl Pts',(4.1560722555045,2.29176233052638,15.4437067653028));
#58821=CARTESIAN_POINT('Ctrl Pts',(4.03722420398995,2.27024273359146,15.4694807885648));
#58822=CARTESIAN_POINT('Ctrl Pts',(3.91799531497457,2.24956537429438,15.4941382888263));
#58823=CARTESIAN_POINT('Ctrl Pts',(3.7984066156939,2.2297482034648,15.5176780933186));
#58824=CARTESIAN_POINT('Ctrl Pts',(3.73861226605356,2.21983961805001,15.5294479955647));
#58825=CARTESIAN_POINT('Ctrl Pts',(3.67872796073169,2.21014607752472,15.540938459558));
#58826=CARTESIAN_POINT('Ctrl Pts',(3.61875638520038,2.20066963256445,15.5521492675595));
#58827=CARTESIAN_POINT('Ctrl Pts',(3.58877059743473,2.19593141008432,15.5577546715602));
#58828=CARTESIAN_POINT('Ctrl Pts',(3.55876299195175,2.19124746136859,15.5632901606998));
#58829=CARTESIAN_POINT('Ctrl Pts',(3.52873390545623,2.18661803702737,15.568755703007));
#58830=CARTESIAN_POINT('Ctrl Pts',(3.51371936220847,2.18430332485676,15.5714884741606));
#58831=CARTESIAN_POINT('Ctrl Pts',(3.49869944869878,2.18200224377232,15.5742037585528));
#58832=CARTESIAN_POINT('Ctrl Pts',(3.48367420720818,2.1797148244456,15.5769015519158));
#58833=CARTESIAN_POINT('Ctrl Pts',(3.47616158646288,2.17857111478224,15.5782504485973));
#58834=CARTESIAN_POINT('Ctrl Pts',(3.46864763372183,2.17743082055785,15.5795949725182));
#58835=CARTESIAN_POINT('Ctrl Pts',(3.46113235428294,2.17629394556369,15.5809351231284));
#58836=CARTESIAN_POINT('Ctrl Pts',(3.45361707484405,2.17515707056953,15.5822752737386));
#58837=CARTESIAN_POINT('Ctrl Pts',(3.44743233343186,2.17422380971264,15.5833751816107));
#58838=CARTESIAN_POINT('Ctrl Pts',(3.43858254117336,2.17289358204932,15.5849424544647));
#58839=CARTESIAN_POINT('Ctrl Pts',(3.14008338800505,2.12802565527505,15.6378057992805));
#58840=CARTESIAN_POINT('Ctrl Pts',(2.84023806810342,2.08874745949898,15.6836350337927));
#58841=CARTESIAN_POINT('Ctrl Pts',(2.53936105399959,2.05530037816818,15.7224748688494));
#58842=CARTESIAN_POINT('Ctrl Pts',(2.46824426694122,2.04739465972102,15.7316552453808));
#58843=CARTESIAN_POINT('Ctrl Pts',(2.397069716932,2.03981481366109,15.740444968727));
#58844=CARTESIAN_POINT('Ctrl Pts',(2.32584133863707,2.03256421704252,15.7488443180986));
#58845=CARTESIAN_POINT('Ctrl Pts',(2.02872663239869,2.00231982659104,15.7838804972295));
#58846=CARTESIAN_POINT('Ctrl Pts',(1.73067698408626,1.97780192424327,15.8121272568313));
#58847=CARTESIAN_POINT('Ctrl Pts',(1.43206897838644,1.95907405420351,15.8336317426784));
#58848=CARTESIAN_POINT('Ctrl Pts',(1.13260365157316,1.94029241534949,15.8551979691667));
#58849=CARTESIAN_POINT('Ctrl Pts',(0.832576211040715,1.92733393854369,15.8699832033154));
#58850=CARTESIAN_POINT('Ctrl Pts',(0.532350103633079,1.92029402808205,15.8779965148456));
#58851=CARTESIAN_POINT('Ctrl Pts',(0.355508731868288,1.91614732866977,15.8827165740556));
#58852=CARTESIAN_POINT('Ctrl Pts',(0.178598162966609,1.91405469724503,15.8850863636833));
#58853=CARTESIAN_POINT('Ctrl Pts',(0.00169119634424886,1.91404105211554,
15.8851013992713));
#58854=CARTESIAN_POINT('Ctrl Pts',(0.00127018941862394,1.91404101964257,
15.8851014350533));
#58855=CARTESIAN_POINT('Ctrl Pts',(0.000849182513112402,1.91404099894601,
15.8851014574968));
#58856=CARTESIAN_POINT('Ctrl Pts',(0.000428175628690854,1.91404099002539,
15.885101466602));
#58857=CARTESIAN_POINT('Ctrl Pts',(-0.295821261727005,1.91403471286351,
15.8851078735931));
#58858=CARTESIAN_POINT('Ctrl Pts',(-0.592082537846746,1.91982817586115,
15.8785163704752));
#58859=CARTESIAN_POINT('Ctrl Pts',(-0.888018597841453,1.93134935298145,
15.8653354740815));
#58860=CARTESIAN_POINT('Ctrl Pts',(-1.16781466674178,1.94224217917986,15.8528734476707));
#58861=CARTESIAN_POINT('Ctrl Pts',(-1.44732031479291,1.95825540061563,15.8345208284142));
#58862=CARTESIAN_POINT('Ctrl Pts',(-1.72623621321286,1.97935406242927,15.8102539049019));
#58863=CARTESIAN_POINT('Ctrl Pts',(-1.92541348354479,1.99442087608708,15.7929245966339));
#58864=CARTESIAN_POINT('Ctrl Pts',(-2.12429486350001,2.01206591538091,15.772580171839));
#58865=CARTESIAN_POINT('Ctrl Pts',(-2.32276918863322,2.03225621732713,15.749205779174));
#58866=CARTESIAN_POINT('Ctrl Pts',(-2.41024261755301,2.04115467278718,15.7389040019846));
#58867=CARTESIAN_POINT('Ctrl Pts',(-2.49763694585371,2.05054760835353,15.7280135760389));
#58868=CARTESIAN_POINT('Ctrl Pts',(-2.5849451592377,2.06042746753833,15.7165340406164));
#58869=CARTESIAN_POINT('Ctrl Pts',(-2.72764899419556,2.07657593444503,15.6977709292798));
#58870=CARTESIAN_POINT('Ctrl Pts',(-2.8701197132973,2.09403058809539,15.6774337170849));
#58871=CARTESIAN_POINT('Ctrl Pts',(-3.0123190135386,2.11276975943822,15.6555185530409));
#58872=CARTESIAN_POINT('Ctrl Pts',(-3.08341866365925,2.12213934510964,15.6445609710189));
#58873=CARTESIAN_POINT('Ctrl Pts',(-3.15445045723932,2.13183005722226,15.6332088769221));
#58874=CARTESIAN_POINT('Ctrl Pts',(-3.22540966173381,2.14183879526575,15.621461681064));
#58875=CARTESIAN_POINT('Ctrl Pts',(-3.26088926398105,2.1468431642875,15.615588083135));
#58876=CARTESIAN_POINT('Ctrl Pts',(-3.29635071879944,2.15192703959139,15.6096157081738));
#58877=CARTESIAN_POINT('Ctrl Pts',(-3.33179343581059,2.15709002170296,15.603544473918));
#58878=CARTESIAN_POINT('Ctrl Pts',(-3.34951479431616,2.15967151275875,15.6005088567902));
#58879=CARTESIAN_POINT('Ctrl Pts',(-3.3672314683567,2.16227278050301,15.5974485247369));
#58880=CARTESIAN_POINT('Ctrl Pts',(-3.38494338430507,2.16489377364487,15.5943634669989));
#58881=CARTESIAN_POINT('Ctrl Pts',(-3.39379934227925,2.16620427021581,15.5928209381299));
#58882=CARTESIAN_POINT('Ctrl Pts',(-3.4026541107295,2.16751969813528,15.5912722278333));
#58883=CARTESIAN_POINT('Ctrl Pts',(-3.41150768046408,2.16884005090279,15.5897173347344));
#58884=CARTESIAN_POINT('Ctrl Pts',(-3.42036125019866,2.17016040367029,15.5881624416356));
#58885=CARTESIAN_POINT('Ctrl Pts',(-3.43054576231002,2.17168588194971,15.5863654858208));
#58886=CARTESIAN_POINT('Ctrl Pts',(-3.43806478433061,2.17281587722003,15.5850341056336));
#58887=CARTESIAN_POINT('Ctrl Pts',(-3.77201242870819,2.22300315658308,15.5259025754879));
#58888=CARTESIAN_POINT('Ctrl Pts',(-4.10337711699034,2.27999983117208,15.4581331881754));
#58889=CARTESIAN_POINT('Ctrl Pts',(-4.43166424742788,2.34336085642193,15.3817687090566));
#58890=CARTESIAN_POINT('Ctrl Pts',(-4.75049586433221,2.40489692121435,15.3076037233045));
#58891=CARTESIAN_POINT('Ctrl Pts',(-5.0664249048189,2.47243665009828,15.2253313086487));
#58892=CARTESIAN_POINT('Ctrl Pts',(-5.37910815822552,2.54552983393255,15.1349700559336));
#58893=CARTESIAN_POINT('Ctrl Pts',(-5.65842118622162,2.61082235689373,15.0542523493268));
#58894=CARTESIAN_POINT('Ctrl Pts',(-5.93514414538488,2.68054677629062,14.9670796084188));
#58895=CARTESIAN_POINT('Ctrl Pts',(-6.20901142408678,2.754393574655,14.8734392389871));
#58896=CARTESIAN_POINT('Ctrl Pts',(-6.22266346129535,2.75807477104978,14.8687713508999));
#58897=CARTESIAN_POINT('Ctrl Pts',(-6.23630839772604,2.76176621297451,14.8640873862658));
#58898=CARTESIAN_POINT('Ctrl Pts',(-6.24994620423252,2.76546786623744,14.8593873420339));
#58899=CARTESIAN_POINT('Ctrl Pts',(6.26385989004508,3.90573722903797,15.8144313886596));
#58900=CARTESIAN_POINT('Ctrl Pts',(5.97575428768946,3.82586736882485,15.9102651438246));
#58901=CARTESIAN_POINT('Ctrl Pts',(5.68582534910169,3.75094724810674,15.9988446813235));
#58902=CARTESIAN_POINT('Ctrl Pts',(5.3945598678898,3.6812480626751,16.0802607757235));
#58903=CARTESIAN_POINT('Ctrl Pts',(5.12091588958906,3.61576566391478,16.1567512128211));
#58904=CARTESIAN_POINT('Ctrl Pts',(4.84609219773543,3.55489216164144,16.2269184315589));
#58905=CARTESIAN_POINT('Ctrl Pts',(4.57049247071768,3.49883082501622,16.2908752458165));
#58906=CARTESIAN_POINT('Ctrl Pts',(4.3141786584873,3.44669254801345,16.3503564908012));
#58907=CARTESIAN_POINT('Ctrl Pts',(4.05719362167251,3.39871677068944,16.4044660162595));
#58908=CARTESIAN_POINT('Ctrl Pts',(3.79986208486601,3.35504215638728,16.4533307302619));
#58909=CARTESIAN_POINT('Ctrl Pts',(3.5788250075668,3.31752748089386,16.4953034853318));
#58910=CARTESIAN_POINT('Ctrl Pts',(3.35753227928865,3.28318603588267,16.5334069594315));
#58911=CARTESIAN_POINT('Ctrl Pts',(3.13618969347213,3.25208718836777,16.5677462998486));
#58912=CARTESIAN_POINT('Ctrl Pts',(2.89302858237386,3.21792281693557,16.6054705910844));
#58913=CARTESIAN_POINT('Ctrl Pts',(2.64982777084286,3.18767649632752,16.6386688269005));
#58914=CARTESIAN_POINT('Ctrl Pts',(2.40682922976721,3.16139780783334,16.6673754459146));
#58915=CARTESIAN_POINT('Ctrl Pts',(2.16739919224934,3.13550502944781,16.6956604999612));
#58916=CARTESIAN_POINT('Ctrl Pts',(1.9281655280082,3.11346424917113,16.7195848778018));
#58917=CARTESIAN_POINT('Ctrl Pts',(1.68935970347767,3.09529058551682,16.7392205017433));
#58918=CARTESIAN_POINT('Ctrl Pts',(1.45216061585603,3.07723919817726,16.758724012987));
#58919=CARTESIAN_POINT('Ctrl Pts',(1.21538363011777,3.06300312649857,16.7739962464026));
#58920=CARTESIAN_POINT('Ctrl Pts',(0.97925557199319,3.05256423844098,16.7851468963415));
#58921=CARTESIAN_POINT('Ctrl Pts',(0.744819945335308,3.04220017038896,16.796217624771));
#58922=CARTESIAN_POINT('Ctrl Pts',(0.511023977340595,3.03557908285324,16.8032256251656));
#58923=CARTESIAN_POINT('Ctrl Pts',(0.278089651340314,3.0326499369104,16.8063174478311));
#58924=CARTESIAN_POINT('Ctrl Pts',(0.185394849023527,3.03148430104732,16.8075478199093));
#58925=CARTESIAN_POINT('Ctrl Pts',(0.0928364957948917,3.03090294439015,
16.8081584672785));
#58926=CARTESIAN_POINT('Ctrl Pts',(0.000428580633955471,3.03090115441879,
16.8081603748149));
#58927=CARTESIAN_POINT('Ctrl Pts',(0.000285720792900251,3.03090115165155,
16.8081603777639));
#58928=CARTESIAN_POINT('Ctrl Pts',(0.000142860581873481,3.0309011502693,
16.8081603792583));
#58929=CARTESIAN_POINT('Ctrl Pts',(9.25926002537381E-13,3.03090115027208,
16.8081603792981));
#58930=CARTESIAN_POINT('Ctrl Pts',(-0.229766623293178,3.03090115473717,
16.8081604432517));
#58931=CARTESIAN_POINT('Ctrl Pts',(-0.460490123967034,3.0344866432905,16.8043944620728));
#58932=CARTESIAN_POINT('Ctrl Pts',(-0.69194503962102,3.04172214172834,16.7967026659101));
#58933=CARTESIAN_POINT('Ctrl Pts',(-0.925222791853488,3.04901462375271,
16.7889502925616));
#58934=CARTESIAN_POINT('Ctrl Pts',(-1.15924352503365,3.06001481866249,16.7772100212543));
#58935=CARTESIAN_POINT('Ctrl Pts',(-1.39377640777272,3.07475437006698,16.7613587211585));
#58936=CARTESIAN_POINT('Ctrl Pts',(-1.62977802676596,3.08958622628291,16.745408154048));
#58937=CARTESIAN_POINT('Ctrl Pts',(-1.86629822996335,3.10820436967548,16.7252949381079));
#58938=CARTESIAN_POINT('Ctrl Pts',(-2.10310182209333,3.13060683891653,16.7009341835963));
#58939=CARTESIAN_POINT('Ctrl Pts',(-2.34274022974235,3.15327749187429,16.6762818024065));
#58940=CARTESIAN_POINT('Ctrl Pts',(-2.58266885192898,3.17982357446078,16.6472795948639));
#58941=CARTESIAN_POINT('Ctrl Pts',(-2.82264394517536,3.21020880819815,16.6138806971338));
#58942=CARTESIAN_POINT('Ctrl Pts',(-2.92710054047309,3.2234349227111,16.5993427919855));
#58943=CARTESIAN_POINT('Ctrl Pts',(-3.031565940621,3.23738800871796,16.5839723683053));
#58944=CARTESIAN_POINT('Ctrl Pts',(-3.13602004348828,3.25206312380919,16.5677679300934));
#58945=CARTESIAN_POINT('Ctrl Pts',(-3.39881199848447,3.28898366669603,16.5269998235238));
#58946=CARTESIAN_POINT('Ctrl Pts',(-3.66152807655967,3.330475068804,16.4809254841673));
#58947=CARTESIAN_POINT('Ctrl Pts',(-3.92382420254392,3.37641784233135,16.4293734954318));
#58948=CARTESIAN_POINT('Ctrl Pts',(-4.19336752573358,3.42363000685205,16.3763971340439));
#58949=CARTESIAN_POINT('Ctrl Pts',(-4.46246736982849,3.47554247180431,16.3176366166871));
#58950=CARTESIAN_POINT('Ctrl Pts',(-4.73075034417782,3.53198937119391,16.2529547001071));
#58951=CARTESIAN_POINT('Ctrl Pts',(-5.02422899918551,3.59373745696935,16.182198209028));
#58952=CARTESIAN_POINT('Ctrl Pts',(-5.31673014775518,3.66091130547962,16.1043559293831));
#58953=CARTESIAN_POINT('Ctrl Pts',(-5.60776500962217,3.73325701383207,16.0193031511413));
#58954=CARTESIAN_POINT('Ctrl Pts',(-5.82736838303714,3.78784621838432,15.9551256952159));
#58955=CARTESIAN_POINT('Ctrl Pts',(-6.04613690946994,3.84537918370047,15.8868441243541));
#58956=CARTESIAN_POINT('Ctrl Pts',(-6.26386060035812,3.90573752918775,15.8144217504419));
#58957=CARTESIAN_POINT('Ctrl Pts',(-6.390311350216,8.98426037265861,25.6807373550228));
#58958=CARTESIAN_POINT('Ctrl Pts',(-4.260207566811,8.27687305387726,25.9287992801895));
#58959=CARTESIAN_POINT('Ctrl Pts',(0.0001663376447509,7.56887468463083,
26.1774672305152));
#58960=CARTESIAN_POINT('Ctrl Pts',(4.2605402421,8.27692834075613,25.9287798619571));
#58961=CARTESIAN_POINT('Ctrl Pts',(6.39081036315,8.98442609659955,25.6806792400505));
#58962=CARTESIAN_POINT('Ctrl Pts',(-6.390311350216,8.18394872075491,25.1149839598735));
#58963=CARTESIAN_POINT('Ctrl Pts',(-4.260207566811,7.53598946889127,25.3660580162986));
#58964=CARTESIAN_POINT('Ctrl Pts',(0.0001663376447509,6.88615615907008,
25.6190369308858));
#58965=CARTESIAN_POINT('Ctrl Pts',(4.2605402421,7.53604021371134,25.3660382614307));
#58966=CARTESIAN_POINT('Ctrl Pts',(6.39081036315,8.18410052210986,25.1149251392324));
#58967=CARTESIAN_POINT('Ctrl Pts',(-6.390311350216,6.63374485883001,23.7052292454154));
#58968=CARTESIAN_POINT('Ctrl Pts',(-4.260207566811,6.0952594820613,23.9981327481698));
#58969=CARTESIAN_POINT('Ctrl Pts',(0.0001663376447509,5.55782025246395,
24.2900565601985));
#58970=CARTESIAN_POINT('Ctrl Pts',(4.2605402421,6.09530145014608,23.9981099521357));
#58971=CARTESIAN_POINT('Ctrl Pts',(6.39081036315,6.63387101309451,23.7051606251128));
#58972=CARTESIAN_POINT('Ctrl Pts',(-6.390311350216,4.89945807530355,21.0044950488482));
#58973=CARTESIAN_POINT('Ctrl Pts',(-4.260207566811,4.44478852897079,21.4424839271908));
#58974=CARTESIAN_POINT('Ctrl Pts',(0.0001663376447509,3.9894320739417,21.8807691942861));
#58975=CARTESIAN_POINT('Ctrl Pts',(4.2605402421,4.44482408729352,21.4424497019397));
#58976=CARTESIAN_POINT('Ctrl Pts',(6.39081036315,4.89956459350057,21.0043924385214));
#58977=CARTESIAN_POINT('Ctrl Pts',(-6.390311350216,4.02649740779966,18.1257286739828));
#58978=CARTESIAN_POINT('Ctrl Pts',(-4.260207566811,3.53810588786846,18.7393844386643));
#58979=CARTESIAN_POINT('Ctrl Pts',(0.0001663376447509,3.05102639999064,
19.3530201602777));
#58980=CARTESIAN_POINT('Ctrl Pts',(4.2605402421,3.53814392341047,18.7393365204708));
#58981=CARTESIAN_POINT('Ctrl Pts',(6.39081036315,4.02661182627713,18.1255849090983));
#58982=CARTESIAN_POINT('Ctrl Pts',(-6.390311350216,3.91822558910252,16.240123855731));
#58983=CARTESIAN_POINT('Ctrl Pts',(-4.260207566811,3.34432525984736,16.9588977715367));
#58984=CARTESIAN_POINT('Ctrl Pts',(0.0001663376447509,2.76847548009877,
17.6776814527756));
#58985=CARTESIAN_POINT('Ctrl Pts',(4.2605402421,3.34437022737152,16.9588416424509));
#58986=CARTESIAN_POINT('Ctrl Pts',(6.39081036315,3.91836004022115,16.2399554641724));
#58987=CARTESIAN_POINT('Ctrl Pts',(-6.390311350216,3.94962416452014,15.4599810530666));
#58988=CARTESIAN_POINT('Ctrl Pts',(-4.260207566811,3.32898447675662,16.2180891202845));
#58989=CARTESIAN_POINT('Ctrl Pts',(0.0001663376447509,2.70679255855811,
16.9762181824682));
#58990=CARTESIAN_POINT('Ctrl Pts',(4.2605402421,3.32903306309379,16.2180299187524));
#58991=CARTESIAN_POINT('Ctrl Pts',(6.39081036315,3.94976956555253,15.4598034464652));
#58992=CARTESIAN_POINT('',(-6.27159361731543,8.76070973784035,25.560856303641));
#58993=CARTESIAN_POINT('Ctrl Pts',(-6.27159386307865,8.7607092746329,25.560857167973));
#58994=CARTESIAN_POINT('Ctrl Pts',(-6.19789584443463,8.73653383838215,25.5688564326203));
#58995=CARTESIAN_POINT('Ctrl Pts',(-6.11723339296007,8.71055314298554,25.5775121686293));
#58996=CARTESIAN_POINT('Ctrl Pts',(-6.02951379280947,8.6830033204438,25.5867458367231));
#58997=CARTESIAN_POINT('Ctrl Pts',(-5.94295765287483,8.65581890224077,25.595857034976));
#58998=CARTESIAN_POINT('Ctrl Pts',(-5.84953032636904,8.62710668875392,25.6055309450653));
#58999=CARTESIAN_POINT('Ctrl Pts',(-5.74914273791409,8.5971414490545,25.6156747169211));
#59000=CARTESIAN_POINT('Ctrl Pts',(-5.64673108221044,8.56657203446444,25.6260230128292));
#59001=CARTESIAN_POINT('Ctrl Pts',(-5.53707566211109,8.53469824792391,25.6368604233356));
#59002=CARTESIAN_POINT('Ctrl Pts',(-5.42008190491958,8.50186484299704,25.6480690713867));
#59003=CARTESIAN_POINT('Ctrl Pts',(-5.30308814772807,8.46903143807017,25.6592777194379));
#59004=CARTESIAN_POINT('Ctrl Pts',(-5.1787560534444,8.43523827313954,25.6708576585075));
#59005=CARTESIAN_POINT('Ctrl Pts',(-5.04699104937212,8.40088573760002,25.6826707313487));
#59006=CARTESIAN_POINT('Ctrl Pts',(-4.91609386884737,8.36675945287322,25.694406001568));
#59007=CARTESIAN_POINT('Ctrl Pts',(-4.77785368976756,8.33207908056211,25.7063721043635));
#59008=CARTESIAN_POINT('Ctrl Pts',(-4.63217381914409,8.29729989669217,25.7184182727122));
#59009=CARTESIAN_POINT('Ctrl Pts',(-4.48649394852062,8.26252071282223,25.7304644410609));
#59010=CARTESIAN_POINT('Ctrl Pts',(-4.33337438635348,8.22764256319013,25.7425907306237));
#59011=CARTESIAN_POINT('Ctrl Pts',(-4.17271843965407,8.19317938183559,25.754624827507));
#59012=CARTESIAN_POINT('Ctrl Pts',(-4.01206249295466,8.15871620048106,25.7666589243902));
#59013=CARTESIAN_POINT('Ctrl Pts',(-3.84387131200249,8.12466886539935,25.7786011414393));
#59014=CARTESIAN_POINT('Ctrl Pts',(-3.66807400178512,8.0916212708232,25.7902592314014));
#59015=CARTESIAN_POINT('Ctrl Pts',(-3.58017534667644,8.07509747353512,25.7960882763825));
#59016=CARTESIAN_POINT('Ctrl Pts',(-3.49037543354537,8.05882467347477,25.8018459904061));
#59017=CARTESIAN_POINT('Ctrl Pts',(-3.39866732483497,8.04288236229473,25.8075066450451));
#59018=CARTESIAN_POINT('Ctrl Pts',(-3.35281327047977,8.0349112067047,25.8103369723646));
#59019=CARTESIAN_POINT('Ctrl Pts',(-3.30648215931862,8.02702270521989,25.8131429946146));
#59020=CARTESIAN_POINT('Ctrl Pts',(-3.25967330048623,8.01922725194684,25.8159214242958));
#59021=CARTESIAN_POINT('Ctrl Pts',(-3.23626887107004,8.01532952531032,25.8173106391365));
#59022=CARTESIAN_POINT('Ctrl Pts',(-3.21274500420225,8.01145506267285,25.8186929533658));
#59023=CARTESIAN_POINT('Ctrl Pts',(-3.18910161784883,8.00760518302979,25.8200679461676));
#59024=CARTESIAN_POINT('Ctrl Pts',(-3.17727992467212,8.00568024320826,25.8207554425686));
#59025=CARTESIAN_POINT('Ctrl Pts',(-3.16542835159289,8.00376144925788,25.8214411084579));
#59026=CARTESIAN_POINT('Ctrl Pts',(-3.1535468890103,8.00184896775755,25.8221248909217));
#59027=CARTESIAN_POINT('Ctrl Pts',(-3.14166542642771,7.99993648625723,25.8228086733855));
#59028=CARTESIAN_POINT('Ctrl Pts',(-3.12814002921763,7.99777354469439,25.8235824798023));
#59029=CARTESIAN_POINT('Ctrl Pts',(-3.11781282328897,7.99613062797019,25.8241705346935));
#59030=CARTESIAN_POINT('Ctrl Pts',(-2.86369606000897,7.95570413863917,25.8386405284771));
#59031=CARTESIAN_POINT('Ctrl Pts',(-2.61950244535401,7.92184254420193,25.8508203757612));
#59032=CARTESIAN_POINT('Ctrl Pts',(-2.38554390379139,7.89344260645399,25.8610830655099));
#59033=CARTESIAN_POINT('Ctrl Pts',(-2.16264725215207,7.86638545783056,25.8708605208082));
#59034=CARTESIAN_POINT('Ctrl Pts',(-1.94904069704484,7.84428557582742,25.878897909814));
#59035=CARTESIAN_POINT('Ctrl Pts',(-1.74499397723141,7.82623317289244,25.8855028517309));
#59036=CARTESIAN_POINT('Ctrl Pts',(-1.60616344485852,7.81395057059251,25.8899967617701));
#59037=CARTESIAN_POINT('Ctrl Pts',(-1.4717584003362,7.80354254385131,25.8938272527317));
#59038=CARTESIAN_POINT('Ctrl Pts',(-1.34186380268046,7.7947356937536,25.8970866460556));
#59039=CARTESIAN_POINT('Ctrl Pts',(-1.16964671100351,7.78305937974182,25.9014080208395));
#59040=CARTESIAN_POINT('Ctrl Pts',(-1.00532510305835,7.77419108036862,25.9047256080539));
#59041=CARTESIAN_POINT('Ctrl Pts',(-0.848989845323112,7.76752305953098,
25.9072401816312));
#59042=CARTESIAN_POINT('Ctrl Pts',(-0.768759682953442,7.76410107780889,
25.9085306432284));
#59043=CARTESIAN_POINT('Ctrl Pts',(-0.690632862249034,7.76125935835357,
25.90960933956));
#59044=CARTESIAN_POINT('Ctrl Pts',(-0.6146216645542,7.7589208015061,25.9105016070156));
#59045=CARTESIAN_POINT('Ctrl Pts',(-0.502558941606541,7.75547308516901,
25.9118170700488));
#59046=CARTESIAN_POINT('Ctrl Pts',(-0.395091323682923,7.75311817417789,
25.9127277681256));
#59047=CARTESIAN_POINT('Ctrl Pts',(-0.292241207601631,7.75162351521975,
25.913310108436));
#59048=CARTESIAN_POINT('Ctrl Pts',(-0.240816149560984,7.75087618574069,
25.9136012785912));
#59049=CARTESIAN_POINT('Ctrl Pts',(-0.19054531473662,7.75034420169172,25.913810266976));
#59050=CARTESIAN_POINT('Ctrl Pts',(-0.141430651316284,7.7500001640364,25.9139459993008));
#59051=CARTESIAN_POINT('Ctrl Pts',(-0.102793828366503,7.74972952140035,
25.9140527752703));
#59052=CARTESIAN_POINT('Ctrl Pts',(-0.0657687540226224,7.74957755785452,
25.9141133378556));
#59053=CARTESIAN_POINT('Ctrl Pts',(-0.0282408776468195,7.74952492844427,
25.9141339361307));
#59054=CARTESIAN_POINT('Ctrl Pts',(-0.0188695811777211,7.74951178605909,
25.9141390798415));
#59055=CARTESIAN_POINT('Ctrl Pts',(-0.00946693103737975,7.74950507576206,
25.9141416457731));
#59056=CARTESIAN_POINT('Ctrl Pts',(9.29034748332288E-13,7.74950497091013,
25.9141415602278));
#59057=CARTESIAN_POINT('Ctrl Pts',(0.000814034408002238,7.74950496189421,
25.914141552872));
#59058=CARTESIAN_POINT('Ctrl Pts',(0.00162854409452201,7.74950500183509,
25.9141415258694));
#59059=CARTESIAN_POINT('Ctrl Pts',(0.00244354999465827,7.74950509090949,
25.9141414791492));
#59060=CARTESIAN_POINT('Ctrl Pts',(0.132296585289549,7.74951928293074,25.9141340353286));
#59061=CARTESIAN_POINT('Ctrl Pts',(0.269950165813914,7.75078018591596,25.9136311334706));
#59062=CARTESIAN_POINT('Ctrl Pts',(0.415338008371231,7.75379326809187,25.9124697500803));
#59063=CARTESIAN_POINT('Ctrl Pts',(0.562124815418347,7.75683534302876,25.9112971915182));
#59064=CARTESIAN_POINT('Ctrl Pts',(0.716795443280676,7.76166350274542,25.9094534038994));
#59065=CARTESIAN_POINT('Ctrl Pts',(0.879281676902341,7.76884826647791,25.9067525338815));
#59066=CARTESIAN_POINT('Ctrl Pts',(1.03425298681161,7.7757007377439,25.9041765780282));
#59067=CARTESIAN_POINT('Ctrl Pts',(1.19633368294311,7.78469728741838,25.900820828321));
#59068=CARTESIAN_POINT('Ctrl Pts',(1.36546458400579,7.79637447397498,25.8965091992107));
#59069=CARTESIAN_POINT('Ctrl Pts',(1.56040862413761,7.80983385904544,25.8915395195541));
#59070=CARTESIAN_POINT('Ctrl Pts',(1.76469848348762,7.82685195067153,25.8852992336672));
#59071=CARTESIAN_POINT('Ctrl Pts',(1.97810882769652,7.84828951177721,25.877498195159));
#59072=CARTESIAN_POINT('Ctrl Pts',(2.05047989003362,7.85555935184465,25.8748527308715));
#59073=CARTESIAN_POINT('Ctrl Pts',(2.12389981084038,7.86333785656272,25.8720276315337));
#59074=CARTESIAN_POINT('Ctrl Pts',(2.19835980240383,7.87165986000744,25.8690111431811));
#59075=CARTESIAN_POINT('Ctrl Pts',(2.34537492442379,7.88809097054327,25.863055335318));
#59076=CARTESIAN_POINT('Ctrl Pts',(2.49643931797058,7.90664055205604,25.8563543239282));
#59077=CARTESIAN_POINT('Ctrl Pts',(2.65146457128827,7.9275790342485,25.8488159962454));
#59078=CARTESIAN_POINT('Ctrl Pts',(2.72897719794712,7.93804827534472,25.845046832404));
#59079=CARTESIAN_POINT('Ctrl Pts',(2.80748002846577,7.94911480280078,25.8410682634669));
#59080=CARTESIAN_POINT('Ctrl Pts',(2.88696074174985,7.96081263315031,25.8368685087714));
#59081=CARTESIAN_POINT('Ctrl Pts',(2.9267010983919,7.96666154832508,25.8347686314237));
#59082=CARTESIAN_POINT('Ctrl Pts',(2.96668592478411,7.97266829189018,25.8326134542077));
#59083=CARTESIAN_POINT('Ctrl Pts',(3.00691356216396,7.97883714334385,25.8304015173849));
#59084=CARTESIAN_POINT('Ctrl Pts',(3.02702738085389,7.98192156907068,25.8292955489735));
#59085=CARTESIAN_POINT('Ctrl Pts',(3.04720190226842,7.98504652189608,25.828175390503));
#59086=CARTESIAN_POINT('Ctrl Pts',(3.06743691470062,7.98821253678811,25.8270408588531));
#59087=CARTESIAN_POINT('Ctrl Pts',(3.07755442091672,7.98979554423412,25.8264735930282));
#59088=CARTESIAN_POINT('Ctrl Pts',(3.08768704988573,7.9913888172036,25.8259027338999));
#59089=CARTESIAN_POINT('Ctrl Pts',(3.09783477468347,7.99299242260474,25.8253282586107));
#59090=CARTESIAN_POINT('Ctrl Pts',(3.1079824994812,7.99459602800587,25.8247537833214));
#59091=CARTESIAN_POINT('Ctrl Pts',(3.11649259020815,7.99594619889963,25.8242701557867));
#59092=CARTESIAN_POINT('Ctrl Pts',(3.12832320949474,7.99783430303326,25.8235939613969));
#59093=CARTESIAN_POINT('Ctrl Pts',(3.31761311808016,8.02804396917128,25.8127748511597));
#59094=CARTESIAN_POINT('Ctrl Pts',(3.49939719834751,8.05986842387775,25.8014674996312));
#59095=CARTESIAN_POINT('Ctrl Pts',(3.67375234747637,8.09268657565345,25.789880031812));
#59096=CARTESIAN_POINT('Ctrl Pts',(3.84164845972872,8.12428896951435,25.7787218250862));
#59097=CARTESIAN_POINT('Ctrl Pts',(4.00265585952441,8.15681325436566,25.7673037128964));
#59098=CARTESIAN_POINT('Ctrl Pts',(4.15684321068927,8.18975608782384,25.7557927511104));
#59099=CARTESIAN_POINT('Ctrl Pts',(4.31992804411597,8.22459990910065,25.7436175417222));
#59100=CARTESIAN_POINT('Ctrl Pts',(4.47538300777857,8.25991157362596,25.7313386112449));
#59101=CARTESIAN_POINT('Ctrl Pts',(4.62328935151025,8.29515455818551,25.7191318794806));
#59102=CARTESIAN_POINT('Ctrl Pts',(4.77119569524193,8.33039754274507,25.7069251477163));
#59103=CARTESIAN_POINT('Ctrl Pts',(4.91155341904269,8.36557198094537,25.6947905665999));
#59104=CARTESIAN_POINT('Ctrl Pts',(5.04444377274572,8.40020003885417,25.6828823980407));
#59105=CARTESIAN_POINT('Ctrl Pts',(5.17491740965991,8.43419835798525,25.6711907889991));
#59106=CARTESIAN_POINT('Ctrl Pts',(5.29821637053551,8.46768019613915,25.6597182023876));
#59107=CARTESIAN_POINT('Ctrl Pts',(5.4144320887901,8.50026217361815,25.6485965003309));
#59108=CARTESIAN_POINT('Ctrl Pts',(5.52974605649533,8.53259133834057,25.6375610946986));
#59109=CARTESIAN_POINT('Ctrl Pts',(5.6380862768788,8.56403474748396,25.626871076913));
#59110=CARTESIAN_POINT('Ctrl Pts',(5.73954207145701,8.59426848248594,25.6166368019706));
#59111=CARTESIAN_POINT('Ctrl Pts',(5.84223096597527,8.62486968015452,25.6062781390239));
#59112=CARTESIAN_POINT('Ctrl Pts',(5.93786707024696,8.65423164742993,25.5963863521321));
#59113=CARTESIAN_POINT('Ctrl Pts',(6.02654300239053,8.68206912588511,25.5870574344231));
#59114=CARTESIAN_POINT('Ctrl Pts',(6.11514461892748,8.70988327490863,25.5777363348915));
#59115=CARTESIAN_POINT('Ctrl Pts',(6.19679772450881,8.73617562297342,25.5689771098566));
#59116=CARTESIAN_POINT('Ctrl Pts',(6.27159470458989,8.76071047653694,25.5608577605037));
#59117=CARTESIAN_POINT('Ctrl Pts',(-6.27159552384839,8.76070944182917,25.5608567088099));
#59118=CARTESIAN_POINT('Ctrl Pts',(-6.27195777361699,8.56459406830873,25.4158727684));
#59119=CARTESIAN_POINT('Ctrl Pts',(-6.2722903133114,8.37478235054355,25.2662940221908));
#59120=CARTESIAN_POINT('Ctrl Pts',(-6.27259314317768,8.1913536795449,25.1127468866755));
#59121=CARTESIAN_POINT('Ctrl Pts',(-6.2728986358801,8.00631208806859,24.9578495842652));
#59122=CARTESIAN_POINT('Ctrl Pts',(-6.27317389396976,7.82776621191305,24.7989137498099));
#59123=CARTESIAN_POINT('Ctrl Pts',(-6.2734189176993,7.65576229132537,24.636542046575));
#59124=CARTESIAN_POINT('Ctrl Pts',(-6.27366754287355,7.4812301967884,24.4717837470997));
#59125=CARTESIAN_POINT('Ctrl Pts',(-6.27388503836533,7.31343373081403,24.3034878218648));
#59126=CARTESIAN_POINT('Ctrl Pts',(-6.27407140443858,7.1523860062935,24.1322428455118));
#59127=CARTESIAN_POINT('Ctrl Pts',(-6.2742180449349,7.02566702872147,23.99750025053));
#59128=CARTESIAN_POINT('Ctrl Pts',(-6.27434541261665,6.90312560578793,23.8609310108925));
#59129=CARTESIAN_POINT('Ctrl Pts',(-6.27445350761239,6.78475354200027,23.7228045339272));
#59130=CARTESIAN_POINT('Ctrl Pts',(-6.27450262993924,6.73096093886088,23.6600348016045));
#59131=CARTESIAN_POINT('Ctrl Pts',(-6.27454777221241,6.67802917492449,23.596943288945));
#59132=CARTESIAN_POINT('Ctrl Pts',(-6.27458893444397,6.62595269073056,23.5335577352352));
#59133=CARTESIAN_POINT('Ctrl Pts',(-6.27470712624797,6.47642208026929,23.3515546548168));
#59134=CARTESIAN_POINT('Ctrl Pts',(-6.2747925032677,6.33394460102529,23.1671310836941));
#59135=CARTESIAN_POINT('Ctrl Pts',(-6.27484506550317,6.19837397944143,22.9809084183222));
#59136=CARTESIAN_POINT('Ctrl Pts',(-6.27489762773865,6.06280335785757,22.7946857529503));
#59137=CARTESIAN_POINT('Ctrl Pts',(-6.27491737518986,5.93413948700878,22.6066638313622));
#59138=CARTESIAN_POINT('Ctrl Pts',(-6.2749043078568,5.8122156331048,22.4174136415825));
#59139=CARTESIAN_POINT('Ctrl Pts',(-6.27489476774449,5.72320227013048,22.2792471114374));
#59140=CARTESIAN_POINT('Ctrl Pts',(-6.27486753879387,5.63762486509131,22.1401744339752));
#59141=CARTESIAN_POINT('Ctrl Pts',(-6.27482283819033,5.55559553449373,22.0006684995205));
#59142=CARTESIAN_POINT('Ctrl Pts',(-6.27477792069608,5.47316819138009,21.8604856717208));
#59143=CARTESIAN_POINT('Ctrl Pts',(-6.27471536159001,5.39432351602081,21.719865714071));
#59144=CARTESIAN_POINT('Ctrl Pts',(-6.27463538123425,5.31912418999798,21.579301685377));
#59145=CARTESIAN_POINT('Ctrl Pts',(-6.27457691148509,5.26414961920891,21.476542158736));
#59146=CARTESIAN_POINT('Ctrl Pts',(-6.27450913119094,5.21112218524964,21.3738128162492));
#59147=CARTESIAN_POINT('Ctrl Pts',(-6.27443212644733,5.16004899754176,21.2713091693909));
#59148=CARTESIAN_POINT('Ctrl Pts',(-6.27435635475634,5.10979362863869,21.1704468810169));
#59149=CARTESIAN_POINT('Ctrl Pts',(-6.27427024761671,5.06062331622896,21.0681861191557));
#59150=CARTESIAN_POINT('Ctrl Pts',(-6.27417380502847,5.01262251510087,20.9645377933533));
#59151=CARTESIAN_POINT('Ctrl Pts',(-6.27399075539136,4.92151619592085,20.7678115464762));
#59152=CARTESIAN_POINT('Ctrl Pts',(-6.27377047264002,4.83462175639446,20.5660838236771));
#59153=CARTESIAN_POINT('Ctrl Pts',(-6.27351295677444,4.75246063087173,20.359496943365));
#59154=CARTESIAN_POINT('Ctrl Pts',(-6.27325823305762,4.67119034787724,20.1551500077663));
#59155=CARTESIAN_POINT('Ctrl Pts',(-6.27296707925897,4.59455128074756,19.9460486010722));
#59156=CARTESIAN_POINT('Ctrl Pts',(-6.27263949537848,4.52307269166766,19.7323746340451));
#59157=CARTESIAN_POINT('Ctrl Pts',(-6.27231699866829,4.45270411982966,19.5220188884686));
#59158=CARTESIAN_POINT('Ctrl Pts',(-6.27195919456296,4.38733700196248,19.3072314291763));
#59159=CARTESIAN_POINT('Ctrl Pts',(-6.27156608306249,4.32750028726097,19.0882301610031));
#59160=CARTESIAN_POINT('Ctrl Pts',(-6.27136275163803,4.29655058362445,18.9749548186019));
#59161=CARTESIAN_POINT('Ctrl Pts',(-6.271149974317,4.2670808390044,18.8605528781773));
#59162=CARTESIAN_POINT('Ctrl Pts',(-6.2709277510994,4.23916681564939,18.7450593575327));
#59163=CARTESIAN_POINT('Ctrl Pts',(-6.27050608302727,4.18620001703831,18.5259106532752));
#59164=CARTESIAN_POINT('Ctrl Pts',(-6.27005040565995,4.13883316994885,18.3028289465057));
#59165=CARTESIAN_POINT('Ctrl Pts',(-6.26956071854046,4.09760165659947,18.0760878674739));
#59166=CARTESIAN_POINT('Ctrl Pts',(-6.26938505201858,4.08281058643722,17.9947485486814));
#59167=CARTESIAN_POINT('Ctrl Pts',(-6.26920500882359,4.06880928510534,17.9129387397966));
#59168=CARTESIAN_POINT('Ctrl Pts',(-6.26902058893439,4.05562321457744,17.8306725394457));
#59169=CARTESIAN_POINT('Ctrl Pts',(-6.26850854166759,4.01901170047753,17.6022580055087));
#59170=CARTESIAN_POINT('Ctrl Pts',(-6.26796275395663,3.98868443887669,17.3703213887534));
#59171=CARTESIAN_POINT('Ctrl Pts',(-6.26738322534997,3.96507786816877,17.1352143265461));
#59172=CARTESIAN_POINT('Ctrl Pts',(-6.26681231314397,3.94182227870524,16.9036028237013));
#59173=CARTESIAN_POINT('Ctrl Pts',(-6.26620865589936,3.92508904508753,16.6689144045329));
#59174=CARTESIAN_POINT('Ctrl Pts',(-6.26557225318442,3.91530350242448,16.4315347899381));
#59175=CARTESIAN_POINT('Ctrl Pts',(-6.26502584174864,3.90690169600378,16.2277221207056));
#59176=CARTESIAN_POINT('Ctrl Pts',(-6.26445529089762,3.90362174274592,16.02192627987));
#59177=CARTESIAN_POINT('Ctrl Pts',(-6.26386060035812,3.90573752918775,15.8144217504419));
#59178=CARTESIAN_POINT('Ctrl Pts',(-6.09387055512539,9.75736361516117,25.6953077691695));
#59179=CARTESIAN_POINT('Ctrl Pts',(-6.05578069227928,9.74451714524749,25.6998076991855));
#59180=CARTESIAN_POINT('Ctrl Pts',(-5.7118011452561,9.62959716207432,25.7401664910213));
#59181=CARTESIAN_POINT('Ctrl Pts',(-5.02575508002472,9.41991852694549,25.8155531544346));
#59182=CARTESIAN_POINT('Ctrl Pts',(-3.98545756790916,9.15752992500609,25.9125296973922));
#59183=CARTESIAN_POINT('Ctrl Pts',(-2.81199940005833,8.93210922179495,25.9977998207745));
#59184=CARTESIAN_POINT('Ctrl Pts',(-1.52033800454874,8.77271519431179,26.0595632938288));
#59185=CARTESIAN_POINT('Ctrl Pts',(-0.189364146702586,8.70902521570103,
26.0852161182419));
#59186=CARTESIAN_POINT('Ctrl Pts',(1.08600948443229,8.74409647810586,26.0709736512751));
#59187=CARTESIAN_POINT('Ctrl Pts',(2.24105687247373,8.85467761705376,26.0276782166891));
#59188=CARTESIAN_POINT('Ctrl Pts',(3.2726709241743,9.01596244605114,25.9659557725239));
#59189=CARTESIAN_POINT('Ctrl Pts',(4.19957173728585,9.2102230477197,25.8929883674436));
#59190=CARTESIAN_POINT('Ctrl Pts',(5.05653935127232,9.43093766095788,25.8116628442957));
#59191=CARTESIAN_POINT('Ctrl Pts',(5.67993901992691,9.61982782716416,25.7436848816572));
#59192=CARTESIAN_POINT('Ctrl Pts',(6.0218052874218,9.73305033543495,25.7038225890372));
#59193=CARTESIAN_POINT('Ctrl Pts',(6.09373583888459,9.75730938060936,25.6953260385087));
#59194=CARTESIAN_POINT('Ctrl Pts',(-6.21813195904801,9.42872268326465,25.8362993824541));
#59195=CARTESIAN_POINT('Ctrl Pts',(-6.17931198320937,9.41558743764238,25.8407694982643));
#59196=CARTESIAN_POINT('Ctrl Pts',(-5.82873515267428,9.29807096860313,25.8808306633429));
#59197=CARTESIAN_POINT('Ctrl Pts',(-5.12944745498144,9.08342540207168,25.9551345139311));
#59198=CARTESIAN_POINT('Ctrl Pts',(-4.06852260420401,8.8143072231865,26.0496506589018));
#59199=CARTESIAN_POINT('Ctrl Pts',(-2.87108324194528,8.58268008383095,26.1318474967083));
#59200=CARTESIAN_POINT('Ctrl Pts',(-1.55234198144858,8.41859936175768,26.1906370912154));
#59201=CARTESIAN_POINT('Ctrl Pts',(-0.193311005377795,8.35288471919688,
26.2145712771427));
#59202=CARTESIAN_POINT('Ctrl Pts',(1.10882136147559,8.38908730322682,26.2013369838684));
#59203=CARTESIAN_POINT('Ctrl Pts',(2.28821900828739,8.50299476126,26.160351622698));
#59204=CARTESIAN_POINT('Ctrl Pts',(3.34121045601103,8.66886917024187,26.1012117007145));
#59205=CARTESIAN_POINT('Ctrl Pts',(4.2868974775528,8.86836587472699,26.0306330877797));
#59206=CARTESIAN_POINT('Ctrl Pts',(5.16080887717921,9.09469004474556,25.9512681740581));
#59207=CARTESIAN_POINT('Ctrl Pts',(5.79625990804498,9.28807268518097,25.8843031567456));
#59208=CARTESIAN_POINT('Ctrl Pts',(6.144685049683,9.40386174784378,25.8447556017848));
#59209=CARTESIAN_POINT('Ctrl Pts',(6.21799459468972,9.42866605228754,25.836314917434));
#59210=CARTESIAN_POINT('Ctrl Pts',(-6.32901962278943,9.07127866903577,25.7779388186334));
#59211=CARTESIAN_POINT('Ctrl Pts',(-6.28949395526499,9.05793150332501,25.7823663832484));
#59212=CARTESIAN_POINT('Ctrl Pts',(-5.93255281589158,8.93852936550552,25.822012056803));
#59213=CARTESIAN_POINT('Ctrl Pts',(-5.22070660987746,8.72061347463833,25.8949526569753));
#59214=CARTESIAN_POINT('Ctrl Pts',(-4.14072872696723,8.44768011879346,25.9865501773639));
#59215=CARTESIAN_POINT('Ctrl Pts',(-2.92175304970983,8.21303070472776,26.0652056115562));
#59216=CARTESIAN_POINT('Ctrl Pts',(-1.57937527961094,8.04705905770207,26.1206423805555));
#59217=CARTESIAN_POINT('Ctrl Pts',(-0.196590777430159,7.98076752197201,
26.1426783013704));
#59218=CARTESIAN_POINT('Ctrl Pts',(1.12799798891678,8.01726693809018,26.1305544980894));
#59219=CARTESIAN_POINT('Ctrl Pts',(2.32844022148747,8.13240355674583,26.0921550930378));
#59220=CARTESIAN_POINT('Ctrl Pts',(3.40033110933316,8.30032567273698,26.0359566715004));
#59221=CARTESIAN_POINT('Ctrl Pts',(4.36302821848509,8.50249774507351,25.9681511314834));
#59222=CARTESIAN_POINT('Ctrl Pts',(5.25262945577457,8.73205768537551,25.8911219437363));
#59223=CARTESIAN_POINT('Ctrl Pts',(5.89949730737536,8.92837895799797,25.8254258028569));
#59224=CARTESIAN_POINT('Ctrl Pts',(6.25423659942717,9.04601668254853,25.7863121700845));
#59225=CARTESIAN_POINT('Ctrl Pts',(6.32887899044518,9.07122133557283,25.7779513691211));
#59226=CARTESIAN_POINT('Ctrl Pts',(-6.39488356451668,8.78685862461965,25.5363210871781));
#59227=CARTESIAN_POINT('Ctrl Pts',(-6.35487788243824,8.77343702129268,25.5407054600534));
#59228=CARTESIAN_POINT('Ctrl Pts',(-5.99362047734077,8.65339956398283,25.5799359106881));
#59229=CARTESIAN_POINT('Ctrl Pts',(-5.27348111855406,8.43484693326501,25.6516207146261));
#59230=CARTESIAN_POINT('Ctrl Pts',(-4.18146072739243,8.16210843159642,25.740672220695));
#59231=CARTESIAN_POINT('Ctrl Pts',(-2.94954017637816,7.92849121802153,25.8163264943927));
#59232=CARTESIAN_POINT('Ctrl Pts',(-1.59371729035546,7.76397112863256,25.8689863324045));
#59233=CARTESIAN_POINT('Ctrl Pts',(-0.198266597753138,7.69871888560939,
25.8894850580979));
#59234=CARTESIAN_POINT('Ctrl Pts',(1.13806229620182,7.73459374464174,25.8782577446869));
#59235=CARTESIAN_POINT('Ctrl Pts',(2.35023472334337,7.84850622225583,25.8419836867962));
#59236=CARTESIAN_POINT('Ctrl Pts',(3.43315220364043,8.01534345346998,25.7882481148275));
#59237=CARTESIAN_POINT('Ctrl Pts',(4.40622894576758,8.21686044545929,25.7228103861928));
#59238=CARTESIAN_POINT('Ctrl Pts',(5.30578955887226,8.44635339776932,25.6478271591733));
#59239=CARTESIAN_POINT('Ctrl Pts',(5.96018308030503,8.64321743602772,25.5832947728205));
#59240=CARTESIAN_POINT('Ctrl Pts',(6.31919099850295,8.76145692896501,25.5446108624864));
#59241=CARTESIAN_POINT('Ctrl Pts',(6.3947399743137,8.78680248751152,25.5363312532158));
#59242=CARTESIAN_POINT('',(5.98852581355243,9.69456736137294,25.7188095578805));
#59243=CARTESIAN_POINT('Origin',(5.99999764423362,9.33250908123741,24.7867226423621));
#59244=CARTESIAN_POINT('',(-5.98852245733777,9.69456809190998,25.7188096065452));
#59245=CARTESIAN_POINT('Ctrl Pts',(-5.98852261949133,9.69456765143689,25.7188097472679));
#59246=CARTESIAN_POINT('Ctrl Pts',(-5.87209162705512,9.65602993335219,25.7323460956292));
#59247=CARTESIAN_POINT('Ctrl Pts',(-5.74896424736322,9.6164051610127,25.7463642488386));
#59248=CARTESIAN_POINT('Ctrl Pts',(-5.61913822764799,9.57607812122987,25.7607354226545));
#59249=CARTESIAN_POINT('Ctrl Pts',(-5.51166398174339,9.54269407233328,25.7726323526536));
#59250=CARTESIAN_POINT('Ctrl Pts',(-5.39959907267352,9.50882946946539,25.7847708339679));
#59251=CARTESIAN_POINT('Ctrl Pts',(-5.28294523335611,9.47472488475404,25.7970626699146));
#59252=CARTESIAN_POINT('Ctrl Pts',(-5.21062717308089,9.45358218231708,25.8046828368811));
#59253=CARTESIAN_POINT('Ctrl Pts',(-5.13654508001346,9.43235034959351,25.8123606216791));
#59254=CARTESIAN_POINT('Ctrl Pts',(-5.06069907855041,9.41109782338285,25.8200693992105));
#59255=CARTESIAN_POINT('Ctrl Pts',(-5.00147803450858,9.39450371470942,25.8260884621128));
#59256=CARTESIAN_POINT('Ctrl Pts',(-4.9411816374162,9.37789704478032,25.8321263597675));
#59257=CARTESIAN_POINT('Ctrl Pts',(-4.87980975520643,9.36131224719765,25.8381705190934));
#59258=CARTESIAN_POINT('Ctrl Pts',(-4.80982349490603,9.34239954778453,25.8450630583581));
#59259=CARTESIAN_POINT('Ctrl Pts',(-4.73843872583953,9.32351554899608,25.8519636512814));
#59260=CARTESIAN_POINT('Ctrl Pts',(-4.66565544719248,9.30471492867056,25.8588519543252));
#59261=CARTESIAN_POINT('Ctrl Pts',(-4.62926380786896,9.2953146185078,25.8622961058471));
#59262=CARTESIAN_POINT('Ctrl Pts',(-4.5925225411935,9.28593515099749,25.8657371798275));
#59263=CARTESIAN_POINT('Ctrl Pts',(-4.55543164722946,9.276583697005,25.8691724714731));
#59264=CARTESIAN_POINT('Ctrl Pts',(-4.53688620024744,9.27190797000876,25.8708901172959));
#59265=CARTESIAN_POINT('Ctrl Pts',(-4.5182533464447,9.2672392462662,25.8726063172043));
#59266=CARTESIAN_POINT('Ctrl Pts',(-4.49953308583469,9.26257842951481,25.8743207280067));
#59267=CARTESIAN_POINT('Ctrl Pts',(-4.49017295552969,9.26024802113911,25.8751779334078));
#59268=CARTESIAN_POINT('Ctrl Pts',(-4.48079097352291,9.257919589503,25.8760346915106));
#59269=CARTESIAN_POINT('Ctrl Pts',(-4.47138713981614,9.25559324869522,25.8768909588464));
#59270=CARTESIAN_POINT('Ctrl Pts',(-4.46198330610937,9.25326690788744,25.8777472261823));
#59271=CARTESIAN_POINT('Ctrl Pts',(-4.45131619556557,9.25063753651448,25.8787153833017));
#59272=CARTESIAN_POINT('Ctrl Pts',(-4.44311008359767,9.24862061315132,25.879458244869));
#59273=CARTESIAN_POINT('Ctrl Pts',(-4.30892004448045,9.21563897384911,25.8916058518184));
#59274=CARTESIAN_POINT('Ctrl Pts',(-4.17039904010703,9.1830097895467,25.9036805413857));
#59275=CARTESIAN_POINT('Ctrl Pts',(-4.02753916638022,9.15105780377832,25.9155540151468));
#59276=CARTESIAN_POINT('Ctrl Pts',(-3.89083751623016,9.12048316398505,25.9269156621496));
#59277=CARTESIAN_POINT('Ctrl Pts',(-3.7501627969802,9.09052877936022,25.9380928402357));
#59278=CARTESIAN_POINT('Ctrl Pts',(-3.60552271823339,9.06149687437662,25.9489689143327));
#59279=CARTESIAN_POINT('Ctrl Pts',(-3.45762471998779,9.03181104545884,25.9600899646091));
#59280=CARTESIAN_POINT('Ctrl Pts',(-3.30557667061893,9.00309070988402,25.9708958864366));
#59281=CARTESIAN_POINT('Ctrl Pts',(-3.14937857027222,8.97567617574966,25.9812526344922));
#59282=CARTESIAN_POINT('Ctrl Pts',(-3.07127952009887,8.96196890868248,25.98643100852));
#59283=CARTESIAN_POINT('Ctrl Pts',(-2.99214295707096,8.94858831228371,25.9914969566742));
#59284=CARTESIAN_POINT('Ctrl Pts',(-2.91196888033323,8.93557803426197,25.9964329681702));
#59285=CARTESIAN_POINT('Ctrl Pts',(-2.89544646589152,8.93289685333387,25.9974501900822));
#59286=CARTESIAN_POINT('Ctrl Pts',(-2.87887999163314,8.93023139589497,25.9984618940561));
#59287=CARTESIAN_POINT('Ctrl Pts',(-2.86226945200005,8.9275820550892,25.99946792148));
#59288=CARTESIAN_POINT('Ctrl Pts',(-2.83857914202376,8.9238035080758,26.0009027394959));
#59289=CARTESIAN_POINT('Ctrl Pts',(-2.81479919798029,8.92005774359815,26.002326011));
#59290=CARTESIAN_POINT('Ctrl Pts',(-2.79092962977707,8.91634587600413,26.003737295366));
#59291=CARTESIAN_POINT('Ctrl Pts',(-2.7706267321079,8.91318864805257,26.0049377009124));
#59292=CARTESIAN_POINT('Ctrl Pts',(-2.75025898982132,8.91005594735042,26.0061294327482));
#59293=CARTESIAN_POINT('Ctrl Pts',(-2.7298264029262,8.90694846685246,26.0073122162978));
#59294=CARTESIAN_POINT('Ctrl Pts',(-2.71961010947864,8.90539472660348,26.0079036080727));
#59295=CARTESIAN_POINT('Ctrl Pts',(-2.70937760487891,8.9038472914013,26.0084927627642));
#59296=CARTESIAN_POINT('Ctrl Pts',(-2.69912888912821,8.90230624805375,26.0090796459032));
#59297=CARTESIAN_POINT('Ctrl Pts',(-2.68888017337751,8.9007652047062,26.0096665290422));
#59298=CARTESIAN_POINT('Ctrl Pts',(-2.67721604462066,8.89902257795092,26.010330388956));
#59299=CARTESIAN_POINT('Ctrl Pts',(-2.6683341084243,8.89770238042146,26.0108334461247));
#59300=CARTESIAN_POINT('Ctrl Pts',(-2.48253474165827,8.87008544425381,26.0213567938855));
#59301=CARTESIAN_POINT('Ctrl Pts',(-2.2918411092769,8.84458851855033,26.0311242682293));
#59302=CARTESIAN_POINT('Ctrl Pts',(-2.09624736712906,8.8216845816214,26.0399422366958));
#59303=CARTESIAN_POINT('Ctrl Pts',(-1.99263644895492,8.80955179092498,26.0446133360839));
#59304=CARTESIAN_POINT('Ctrl Pts',(-1.88765086776274,8.79814730437633,26.0490176494173));
#59305=CARTESIAN_POINT('Ctrl Pts',(-1.78129230367924,8.78754624690616,26.0531239528998));
#59306=CARTESIAN_POINT('Ctrl Pts',(-1.70032438874362,8.77947594690853,26.0562499713256));
#59307=CARTESIAN_POINT('Ctrl Pts',(-1.61856086797209,8.77187004290322,26.059203690954));
#59308=CARTESIAN_POINT('Ctrl Pts',(-1.53600027727007,8.76475978009922,26.0619717492177));
#59309=CARTESIAN_POINT('Ctrl Pts',(-1.46197046667242,8.75838420303267,26.0644537909187));
#59310=CARTESIAN_POINT('Ctrl Pts',(-1.38729978418251,8.7524071578645,26.0667865511724));
#59311=CARTESIAN_POINT('Ctrl Pts',(-1.31198948711474,8.74685080292186,26.0689596020403));
#59312=CARTESIAN_POINT('Ctrl Pts',(-1.23234002195582,8.74097430639156,26.0712578580043));
#59313=CARTESIAN_POINT('Ctrl Pts',(-1.15197439044148,8.73556841058776,26.073377465122));
#59314=CARTESIAN_POINT('Ctrl Pts',(-1.07089259101654,8.73065879334457,26.0753059915675));
#59315=CARTESIAN_POINT('Ctrl Pts',(-1.03035169130407,8.72820398472298,26.0762702547902));
#59316=CARTESIAN_POINT('Ctrl Pts',(-0.989631749612645,8.72587324436221,
26.0771867436368));
#59317=CARTESIAN_POINT('Ctrl Pts',(-0.948732765844986,8.72366974188885,
26.0780538888504));
#59318=CARTESIAN_POINT('Ctrl Pts',(-0.928283273961157,8.72256799065217,
26.0784874614572));
#59319=CARTESIAN_POINT('Ctrl Pts',(-0.907789021558714,8.72149804879681,
26.0789086978804));
#59320=CARTESIAN_POINT('Ctrl Pts',(-0.887250008635169,8.7204603094842,26.0793174011297));
#59321=CARTESIAN_POINT('Ctrl Pts',(-0.876980502173397,8.7199414398279,26.0795217527544));
#59322=CARTESIAN_POINT('Ctrl Pts',(-0.866699805581386,8.71943062080149,
26.0797229710681));
#59323=CARTESIAN_POINT('Ctrl Pts',(-0.856407918859501,8.71892790132903,
26.0799210314036));
#59324=CARTESIAN_POINT('Ctrl Pts',(-0.846116032137616,8.71842518185657,
26.0801190917392));
#59325=CARTESIAN_POINT('Ctrl Pts',(-0.834124913337858,8.7178509455999,26.0803453710984));
#59326=CARTESIAN_POINT('Ctrl Pts',(-0.825498688304884,8.71744409041346,
26.0805057137582));
#59327=CARTESIAN_POINT('Ctrl Pts',(-0.603586179648995,8.70697760539389,
26.084630582023));
#59328=CARTESIAN_POINT('Ctrl Pts',(-0.379552796555947,8.70066335356724,
26.0871469150606));
#59329=CARTESIAN_POINT('Ctrl Pts',(-0.153393845956384,8.698714469009,26.0879160669694));
#59330=CARTESIAN_POINT('Ctrl Pts',(-0.0982314036651066,8.69823911646739,
26.0881036708545));
#59331=CARTESIAN_POINT('Ctrl Pts',(-0.042942542021569,8.69802366194984,
26.0881872185615));
#59332=CARTESIAN_POINT('Ctrl Pts',(0.0124721856994969,8.69806975931062,
26.0881665546718));
#59333=CARTESIAN_POINT('Ctrl Pts',(0.153776193840033,8.69818730462956,26.0881138630759));
#59334=CARTESIAN_POINT('Ctrl Pts',(0.295901299624064,8.70001019720623,26.087381983723));
#59335=CARTESIAN_POINT('Ctrl Pts',(0.438847517233882,8.70357851179769,26.0859643099591));
#59336=CARTESIAN_POINT('Ctrl Pts',(0.510320626038792,8.70536266909342,26.0852554730772));
#59337=CARTESIAN_POINT('Ctrl Pts',(0.581999012323971,8.70758318342142,26.0843751914009));
#59338=CARTESIAN_POINT('Ctrl Pts',(0.653882676053584,8.71024373540388,26.0833231229802));
#59339=CARTESIAN_POINT('Ctrl Pts',(0.689824507918391,8.71157401139511,26.0827970887698));
#59340=CARTESIAN_POINT('Ctrl Pts',(0.725817659130263,8.71301429695668,26.0822281083633));
#59341=CARTESIAN_POINT('Ctrl Pts',(0.761862129614743,8.71456501226555,26.0816161561889));
#59342=CARTESIAN_POINT('Ctrl Pts',(0.779884364856982,8.71534036991999,26.0813101801018));
#59343=CARTESIAN_POINT('Ctrl Pts',(0.797919429916728,8.71614333502365,26.0809934611126));
#59344=CARTESIAN_POINT('Ctrl Pts',(0.815967324782474,8.71697395525709,26.0806659979335));
#59345=CARTESIAN_POINT('Ctrl Pts',(0.83401521964822,8.71780457549052,26.0803385347544));
#59346=CARTESIAN_POINT('Ctrl Pts',(0.853700655374708,8.71874249564784,26.0799689583905));
#59347=CARTESIAN_POINT('Ctrl Pts',(0.870149498784838,8.71954882757381,26.0796513752337));
#59348=CARTESIAN_POINT('Ctrl Pts',(0.954975880144235,8.72370706640852,26.0780136047657));
#59349=CARTESIAN_POINT('Ctrl Pts',(1.03918186933026,8.7284368786165,26.0761547094014));
#59350=CARTESIAN_POINT('Ctrl Pts',(1.12276164329517,8.73371220957732,26.0740868617806));
#59351=CARTESIAN_POINT('Ctrl Pts',(1.34023325878723,8.74743843413957,26.0687063954145));
#59352=CARTESIAN_POINT('Ctrl Pts',(1.55346394526637,8.76485473917061,26.0619130100553));
#59353=CARTESIAN_POINT('Ctrl Pts',(1.76245348567662,8.78548898909608,26.0539195188657));
#59354=CARTESIAN_POINT('Ctrl Pts',(1.93914916545501,8.80293475604758,26.0471612124127));
#59355=CARTESIAN_POINT('Ctrl Pts',(2.11281359860282,8.82268164254982,26.0395445710804));
#59356=CARTESIAN_POINT('Ctrl Pts',(2.28345799976991,8.84446770250537,26.0311854117516));
#59357=CARTESIAN_POINT('Ctrl Pts',(2.31474293705894,8.84846183014638,26.0296528928199));
#59358=CARTESIAN_POINT('Ctrl Pts',(2.34592639292191,8.85252455266215,26.0280953865591));
#59359=CARTESIAN_POINT('Ctrl Pts',(2.37700846453754,8.85665426172438,26.0265135770043));
#59360=CARTESIAN_POINT('Ctrl Pts',(2.47789359773873,8.87005833124641,26.0213793932338));
#59361=CARTESIAN_POINT('Ctrl Pts',(2.57857877971435,8.88427984309705,26.0159461893127));
#59362=CARTESIAN_POINT('Ctrl Pts',(2.67829454913604,8.89918228045029,26.010268885374));
#59363=CARTESIAN_POINT('Ctrl Pts',(2.78016201893597,8.91440628760413,26.0044690746633));
#59364=CARTESIAN_POINT('Ctrl Pts',(2.88101763983595,8.93034084026915,25.9984145814764));
#59365=CARTESIAN_POINT('Ctrl Pts',(2.9800513379607,8.94678980911212,25.9921818732103));
#59366=CARTESIAN_POINT('Ctrl Pts',(3.01383476948858,8.95240105683015,25.9900557052804));
#59367=CARTESIAN_POINT('Ctrl Pts',(3.04740628009826,8.95807174850422,25.9879089442522));
#59368=CARTESIAN_POINT('Ctrl Pts',(3.08073402057498,8.96379283741397,25.9857450608471));
#59369=CARTESIAN_POINT('Ctrl Pts',(3.15917419640476,8.97725799327511,25.9806521444854));
#59370=CARTESIAN_POINT('Ctrl Pts',(3.23647655748982,8.99103650927858,25.9754514131821));
#59371=CARTESIAN_POINT('Ctrl Pts',(3.31263963066391,9.00508372882959,25.9701602706044));
#59372=CARTESIAN_POINT('Ctrl Pts',(3.45655652485398,9.03162719832913,25.9601621865625));
#59373=CARTESIAN_POINT('Ctrl Pts',(3.59640516989599,9.05912869720995,25.9498420248917));
#59374=CARTESIAN_POINT('Ctrl Pts',(3.73218981795613,9.08729847637573,25.9393136497869));
#59375=CARTESIAN_POINT('Ctrl Pts',(3.83601182259918,9.10883731000034,25.9312635717801));
#59376=CARTESIAN_POINT('Ctrl Pts',(3.93745684683485,9.13076709674976,25.923091594256));
#59377=CARTESIAN_POINT('Ctrl Pts',(4.03652489001273,9.15296524319345,25.9148447710799));
#59378=CARTESIAN_POINT('Ctrl Pts',(4.0612919008072,9.15851477980437,25.9127830652858));
#59379=CARTESIAN_POINT('Ctrl Pts',(4.08692151241491,9.16430499799161,25.9106334161247));
#59380=CARTESIAN_POINT('Ctrl Pts',(4.11487271596183,9.17068852739269,25.9082656521577));
#59381=CARTESIAN_POINT('Ctrl Pts',(4.14282391950875,9.17707205679377,25.9058978881908));
#59382=CARTESIAN_POINT('Ctrl Pts',(4.17059661622636,9.1834801016058,25.9035230642124));
#59383=CARTESIAN_POINT('Ctrl Pts',(4.19819080613438,9.18990996456923,25.9011421988763));
#59384=CARTESIAN_POINT('Ctrl Pts',(4.20585187599977,9.19169510954185,25.9004811910431));
#59385=CARTESIAN_POINT('Ctrl Pts',(4.21349918708703,9.19348193687302,25.8998197172862));
#59386=CARTESIAN_POINT('Ctrl Pts',(4.22113273884194,9.1952703903218,25.8991577987902));
#59387=CARTESIAN_POINT('Ctrl Pts',(4.26848933350235,9.20636549621251,25.8950514264333));
#59388=CARTESIAN_POINT('Ctrl Pts',(4.31531637062675,9.21752315728304,25.8909279539873));
#59389=CARTESIAN_POINT('Ctrl Pts',(4.36161386414175,9.22873008213421,25.8867925860485));
#59390=CARTESIAN_POINT('Ctrl Pts',(4.51956603546999,9.26696450866056,25.8726840394387));
#59391=CARTESIAN_POINT('Ctrl Pts',(4.67135538159587,9.30576725556285,25.8584396044212));
#59392=CARTESIAN_POINT('Ctrl Pts',(4.81697964948199,9.34464732854181,25.8442463695933));
#59393=CARTESIAN_POINT('Ctrl Pts',(4.86961306902873,9.35869987090179,25.8391164658055));
#59394=CARTESIAN_POINT('Ctrl Pts',(4.92144124545563,9.37276293483443,25.8339930114225));
#59395=CARTESIAN_POINT('Ctrl Pts',(4.97246446091363,9.38681474486927,25.8288840498562));
#59396=CARTESIAN_POINT('Ctrl Pts',(5.00468126036627,9.39568726185541,25.8256581773055));
#59397=CARTESIAN_POINT('Ctrl Pts',(5.03657708832332,9.4045544425085,25.8224384021553));
#59398=CARTESIAN_POINT('Ctrl Pts',(5.06815190938425,9.41341154727271,25.8192264433304));
#59399=CARTESIAN_POINT('Ctrl Pts',(5.21039246414893,9.45331167822954,25.8047569771611));
#59400=CARTESIAN_POINT('Ctrl Pts',(5.34611826469743,9.49300395844047,25.7904485750103));
#59401=CARTESIAN_POINT('Ctrl Pts',(5.47532885619636,9.53208557266711,25.7764520422943));
#59402=CARTESIAN_POINT('Ctrl Pts',(5.60705590595806,9.57192832613088,25.762182918222));
#59403=CARTESIAN_POINT('Ctrl Pts',(5.73201169332115,9.61113637645999,25.7482377381105));
#59404=CARTESIAN_POINT('Ctrl Pts',(5.85019776510156,9.64932746814793,25.734746207583));
#59405=CARTESIAN_POINT('Ctrl Pts',(5.86233276528394,9.65324881774198,25.7333609366881));
#59406=CARTESIAN_POINT('Ctrl Pts',(5.87439639539093,9.65715948412718,25.7319804242722));
#59407=CARTESIAN_POINT('Ctrl Pts',(5.88638865699179,9.6610590795782,25.7306047944961));
#59408=CARTESIAN_POINT('Ctrl Pts',(5.92103004145991,9.67232362581519,25.7266310886558));
#59409=CARTESIAN_POINT('Ctrl Pts',(5.95507590117461,9.68349577951184,25.7226981412014));
#59410=CARTESIAN_POINT('Ctrl Pts',(5.98852582160936,9.69456702970002,25.7188089328355));
#59411=CARTESIAN_POINT('Origin',(-5.999994980806,9.33250914740904,24.7867195890732));
#59412=CARTESIAN_POINT('Origin',(5.999999877386,9.33250977407517,24.7867246592848));
#59413=CARTESIAN_POINT('Origin',(6.,9.33250981977681,24.7867247762149));
#59414=CARTESIAN_POINT('Ctrl Pts',(6.9999999999895,10.9278021978942,24.1259274561224));
#59415=CARTESIAN_POINT('Ctrl Pts',(6.9999999999895,10.9277942569348,24.1259309538583));
#59416=CARTESIAN_POINT('Ctrl Pts',(6.9999999999895,10.6629101446723,24.2426037363051));
#59417=CARTESIAN_POINT('Ctrl Pts',(6.9999999999895,10.1335216816106,24.468757012286));
#59418=CARTESIAN_POINT('Ctrl Pts',(6.9999999999895,9.5992651391747,24.6831018468203));
#59419=CARTESIAN_POINT('Ctrl Pts',(6.9999999999895,9.3325057408578,24.7867214499759));
#59420=CARTESIAN_POINT('Ctrl Pts',(7.00000270561806,11.1660644378675,24.6668575635543));
#59421=CARTESIAN_POINT('Ctrl Pts',(7.00000270561806,11.1660563761497,24.6668611144804));
#59422=CARTESIAN_POINT('Ctrl Pts',(7.00000270561806,10.8971441621799,24.7853081441803));
#59423=CARTESIAN_POINT('Ctrl Pts',(7.00000270561804,10.3597134220153,25.0148970046547));
#59424=CARTESIAN_POINT('Ctrl Pts',(7.00000270561804,9.8173405913843,25.2324981642003));
#59425=CARTESIAN_POINT('Ctrl Pts',(7.00000270561804,9.54652457492641,25.3376935135328));
#59426=CARTESIAN_POINT('Ctrl Pts',(6.57967197773943,11.3336093881527,25.0472372157089));
#59427=CARTESIAN_POINT('Ctrl Pts',(6.57967197773943,11.333601241518,25.0472408040382));
#59428=CARTESIAN_POINT('Ctrl Pts',(6.57967197773943,11.0618564842979,25.1669354765322));
#59429=CARTESIAN_POINT('Ctrl Pts',(6.57967197773943,10.5187704505481,25.3989402247821));
#59430=CARTESIAN_POINT('Ctrl Pts',(6.57967197773943,9.97069028206527,25.6188312176277));
#59431=CARTESIAN_POINT('Ctrl Pts',(6.57967197773943,9.69702166972346,25.7251346246858));
#59432=CARTESIAN_POINT('Ctrl Pts',(5.98852435812654,11.3308746780979,25.0410285650898));
#59433=CARTESIAN_POINT('Ctrl Pts',(5.98852435812654,11.3308665328493,25.0410321528085));
#59434=CARTESIAN_POINT('Ctrl Pts',(5.98852435812654,11.0591680090977,25.1607064609686));
#59435=CARTESIAN_POINT('Ctrl Pts',(5.98852435812654,10.5161742824468,25.3926717765052));
#59436=CARTESIAN_POINT('Ctrl Pts',(5.98852435812654,9.96818727053848,25.6125253941221));
#59437=CARTESIAN_POINT('Ctrl Pts',(5.98852435812654,9.69456521897248,25.7188107151854));
#59438=CARTESIAN_POINT('',(6.9999999999401,10.9277762175509,24.1259366383994));
#59439=CARTESIAN_POINT('',(5.98852583813019,11.3308502415552,25.0410393194074));
#59440=CARTESIAN_POINT('Origin',(5.99999999906,10.9277802195584,24.1259421376201));
#59441=CARTESIAN_POINT('Origin',(5.98846854897676,-4.75314842173399,-11.4751152994772));
#59442=CARTESIAN_POINT('Origin',(6.99999997874015,-4.74964876082222,-11.4663999132518));
#59443=CARTESIAN_POINT('Ctrl Pts',(-6.05497710532883,11.6468330260664,24.9009950262097));
#59444=CARTESIAN_POINT('Ctrl Pts',(-4.03665140355255,12.1728066175418,24.6398170408189));
#59445=CARTESIAN_POINT('Ctrl Pts',(7.59695908486568E-7,12.7121751393787,
24.4084894089112));
#59446=CARTESIAN_POINT('Ctrl Pts',(4.0366529229439,12.1728064145219,24.6398171278867));
#59447=CARTESIAN_POINT('Ctrl Pts',(6.05497938441634,11.646832432147,24.9009953211277));
#59448=CARTESIAN_POINT('Ctrl Pts',(-6.05497710532883,10.8985073422741,25.2386054571744));
#59449=CARTESIAN_POINT('Ctrl Pts',(-4.03665140355255,11.070715415319,25.1429517412782));
#59450=CARTESIAN_POINT('Ctrl Pts',(7.59695908486568E-7,11.3017723854694,
25.1799926939185));
#59451=CARTESIAN_POINT('Ctrl Pts',(4.0366529229439,11.0707153283507,25.1429517273329));
#59452=CARTESIAN_POINT('Ctrl Pts',(6.05497938441634,10.8985071478217,25.2386055651884));
#59453=CARTESIAN_POINT('Ctrl Pts',(-6.05497710532883,10.1393897253838,25.5530351225277));
#59454=CARTESIAN_POINT('Ctrl Pts',(-4.03665140355255,9.94970084961926,25.6072791213988));
#59455=CARTESIAN_POINT('Ctrl Pts',(7.59695908486568E-7,9.81221489841592,
25.796939183938));
#59456=CARTESIAN_POINT('Ctrl Pts',(4.0366529229439,9.9497009013654,25.6072790500129));
#59457=CARTESIAN_POINT('Ctrl Pts',(6.05497938441634,10.1393899395764,25.5530350612747));
#59458=CARTESIAN_POINT('Ctrl Pts',(-6.05497710532883,9.37151240627548,25.8434422446624));
#59459=CARTESIAN_POINT('Ctrl Pts',(-4.03665140355255,8.81462746052429,26.0307842227122));
#59460=CARTESIAN_POINT('Ctrl Pts',(7.59695908486568E-7,8.2693467820933,
26.2486239006384));
#59461=CARTESIAN_POINT('Ctrl Pts',(4.0366529229439,8.8146276657733,26.0307841407194));
#59462=CARTESIAN_POINT('Ctrl Pts',(6.05497938441634,9.37151303510997,25.8434420331122));
#59463=CARTESIAN_POINT('',(-5.98852246661619,11.3308498387676,25.041039515264));
#59464=CARTESIAN_POINT('Ctrl Pts',(-5.98852262876941,11.3308502497312,25.0410393033033));
#59465=CARTESIAN_POINT('Ctrl Pts',(-5.94977386272025,11.3431047501248,25.0351557412125));
#59466=CARTESIAN_POINT('Ctrl Pts',(-5.90273483017515,11.357905868771,25.0280623795449));
#59467=CARTESIAN_POINT('Ctrl Pts',(-5.84730745884751,11.3750868173769,25.0198539645138));
#59468=CARTESIAN_POINT('Ctrl Pts',(-5.7980099252371,11.3903676862162,25.0125533365715));
#59469=CARTESIAN_POINT('Ctrl Pts',(-5.74207682856626,11.4075322478359,25.0043703278146));
#59470=CARTESIAN_POINT('Ctrl Pts',(-5.67943916884476,11.4264328448299,24.995387473731));
#59471=CARTESIAN_POINT('Ctrl Pts',(-5.62099151837065,11.4440691277269,24.9870055080244));
#59472=CARTESIAN_POINT('Ctrl Pts',(-5.55670627844591,11.4632175893215,24.9779269258027));
#59473=CARTESIAN_POINT('Ctrl Pts',(-5.48652739029172,11.4837185193206,24.9682369644011));
#59474=CARTESIAN_POINT('Ctrl Pts',(-5.4207988987062,11.5029193821497,24.95916149223));
#59475=CARTESIAN_POINT('Ctrl Pts',(-5.34990054958627,11.5233068590478,24.9495496451382));
#59476=CARTESIAN_POINT('Ctrl Pts',(-5.27378628704188,11.5447078507216,24.9394898133861));
#59477=CARTESIAN_POINT('Ctrl Pts',(-5.23117480484552,11.5566888900854,24.9338579603368));
#59478=CARTESIAN_POINT('Ctrl Pts',(-5.18692857181283,11.5689867928501,24.9280860442334));
#59479=CARTESIAN_POINT('Ctrl Pts',(-5.14103950690912,11.5815645387794,24.9221924626799));
#59480=CARTESIAN_POINT('Ctrl Pts',(-5.08921127757209,11.5957701518582,24.9155361079032));
#59481=CARTESIAN_POINT('Ctrl Pts',(-5.03528346648521,11.6103415053243,24.9087206071008));
#59482=CARTESIAN_POINT('Ctrl Pts',(-4.97924174038057,11.625228677746,24.901770743559));
#59483=CARTESIAN_POINT('Ctrl Pts',(-4.97223652461749,11.6270895742988,24.9009020106163));
#59484=CARTESIAN_POINT('Ctrl Pts',(-4.96519827893489,11.6289554054276,24.9000311780376));
#59485=CARTESIAN_POINT('Ctrl Pts',(-4.9581269707769,11.6308260577858,24.8991583011216));
#59486=CARTESIAN_POINT('Ctrl Pts',(-4.95105566261891,11.6326967101439,24.8982854242056));
#59487=CARTESIAN_POINT('Ctrl Pts',(-4.95002336600476,11.6329683362338,24.8981587538712));
#59488=CARTESIAN_POINT('Ctrl Pts',(-4.9467512886278,11.6338319100799,24.8977558964836));
#59489=CARTESIAN_POINT('Ctrl Pts',(-4.94020713387388,11.635559057772,24.8969501817086));
#59490=CARTESIAN_POINT('Ctrl Pts',(-4.93353444378895,11.6373165853176,24.8961304666749));
#59491=CARTESIAN_POINT('Ctrl Pts',(-4.92673308920624,11.639104084663,24.8952969595343));
#59492=CARTESIAN_POINT('Ctrl Pts',(-4.91313038004081,11.6426790833538,24.8936299452533));
#59493=CARTESIAN_POINT('Ctrl Pts',(-4.89901301288448,11.6463739691115,24.8919077622549));
#59494=CARTESIAN_POINT('Ctrl Pts',(-4.88438006285243,11.6501860013663,24.8901318453057));
#59495=CARTESIAN_POINT('Ctrl Pts',(-4.829421636142,11.6645032302801,24.8834618572798));
#59496=CARTESIAN_POINT('Ctrl Pts',(-4.76719038225856,11.6804723613988,24.8760340871454));
#59497=CARTESIAN_POINT('Ctrl Pts',(-4.69762431072455,11.6978935667144,24.8679498539363));
#59498=CARTESIAN_POINT('Ctrl Pts',(-4.69310115448302,11.6990262860389,24.8674242205479));
#59499=CARTESIAN_POINT('Ctrl Pts',(-4.68854698997108,11.700165127177,24.8668958197986));
#59500=CARTESIAN_POINT('Ctrl Pts',(-4.6839618001492,11.7013100279032,24.8663646829141));
#59501=CARTESIAN_POINT('Ctrl Pts',(-4.61785866763921,11.7178156748562,24.8587074618991));
#59502=CARTESIAN_POINT('Ctrl Pts',(-4.54530722999598,11.7355836340615,24.8504802696492));
#59503=CARTESIAN_POINT('Ctrl Pts',(-4.46624869967402,11.7544058575354,24.8417863906958));
#59504=CARTESIAN_POINT('Ctrl Pts',(-4.45548217444166,11.7569691475831,24.8406024214677));
#59505=CARTESIAN_POINT('Ctrl Pts',(-4.44459496772472,11.7595519176375,24.8394098294196));
#59506=CARTESIAN_POINT('Ctrl Pts',(-4.43358693104393,11.7621535716983,24.8382089068316));
#59507=CARTESIAN_POINT('Ctrl Pts',(-4.38766693898259,11.7730063638249,24.8331992618504));
#59508=CARTESIAN_POINT('Ctrl Pts',(-4.33964418259454,11.7841883687306,24.8280443854871));
#59509=CARTESIAN_POINT('Ctrl Pts',(-4.28950715573058,11.7956542720061,24.8227663700682));
#59510=CARTESIAN_POINT('Ctrl Pts',(-4.26443864229859,11.8013872236439,24.8201273623587));
#59511=CARTESIAN_POINT('Ctrl Pts',(-4.23884156124774,11.8071911491883,24.817457568396));
#59512=CARTESIAN_POINT('Ctrl Pts',(-4.21271443784642,11.8130598792849,24.8147599693042));
#59513=CARTESIAN_POINT('Ctrl Pts',(-4.19965087614576,11.8159942443332,24.8134111697584));
#59514=CARTESIAN_POINT('Ctrl Pts',(-4.18645480385771,11.8189448104674,24.8120554188158));
#59515=CARTESIAN_POINT('Ctrl Pts',(-4.17312603658067,11.821910791555,24.8106930950912));
#59516=CARTESIAN_POINT('Ctrl Pts',(-4.16646165294215,11.8233937820988,24.8100119332289));
#59517=CARTESIAN_POINT('Ctrl Pts',(-4.15976409555639,11.8248806263771,24.8093291281626));
#59518=CARTESIAN_POINT('Ctrl Pts',(-4.15303334128542,11.8263712242906,24.8086447280003));
#59519=CARTESIAN_POINT('Ctrl Pts',(-4.14630258701445,11.827861822204,24.807960327838));
#59520=CARTESIAN_POINT('Ctrl Pts',(-4.13831907940943,11.8296249476383,24.8071509729098));
#59521=CARTESIAN_POINT('Ctrl Pts',(-4.13274146466081,11.8308541782705,24.8065867905511));
#59522=CARTESIAN_POINT('Ctrl Pts',(-4.01469641459156,11.8568697060672,24.7946463934847));
#59523=CARTESIAN_POINT('Ctrl Pts',(-3.89907535590093,11.8813165391594,24.7834646730415));
#59524=CARTESIAN_POINT('Ctrl Pts',(-3.7859303789415,11.9043055522377,24.7729779011038));
#59525=CARTESIAN_POINT('Ctrl Pts',(-3.72800057606713,11.9160758405147,24.767608713293));
#59526=CARTESIAN_POINT('Ctrl Pts',(-3.67071985363078,11.9274648234898,24.7624213665553));
#59527=CARTESIAN_POINT('Ctrl Pts',(-3.61409520292724,11.9384921739262,24.7574053705903));
#59528=CARTESIAN_POINT('Ctrl Pts',(-3.53048496112061,11.9547748251218,24.7499989030834));
#59529=CARTESIAN_POINT('Ctrl Pts',(-3.44830456978397,11.9702644006063,24.7429681554761));
#59530=CARTESIAN_POINT('Ctrl Pts',(-3.36757331113062,11.9850131712523,24.7362852046435));
#59531=CARTESIAN_POINT('Ctrl Pts',(-3.32720768180394,11.9923875565753,24.7329437292272));
#59532=CARTESIAN_POINT('Ctrl Pts',(-3.28720433568016,11.999576745109,24.7296892123884));
#59533=CARTESIAN_POINT('Ctrl Pts',(-3.2475654491488,12.0065871586355,24.7265182809435));
#59534=CARTESIAN_POINT('Ctrl Pts',(-3.2124930980483,12.0127899485237,24.7237126516567));
#59535=CARTESIAN_POINT('Ctrl Pts',(-3.17911908413293,12.0186098553888,24.7210821798983));
#59536=CARTESIAN_POINT('Ctrl Pts',(-3.14369422059917,12.0246963262419,24.71833322792));
#59537=CARTESIAN_POINT('Ctrl Pts',(-3.13908178689044,12.0254888047592,24.7179753053339));
#59538=CARTESIAN_POINT('Ctrl Pts',(-3.13443458534099,12.0262857371774,24.7176154050858));
#59539=CARTESIAN_POINT('Ctrl Pts',(-3.12974434028523,12.0270884968926,24.7172529074598));
#59540=CARTESIAN_POINT('Ctrl Pts',(-2.96689344872027,12.0549612698035,24.7046665583719));
#59541=CARTESIAN_POINT('Ctrl Pts',(-2.80360512101477,12.0808137172381,24.6930389394681));
#59542=CARTESIAN_POINT('Ctrl Pts',(-2.63993695717176,12.1046081287205,24.6823718917912));
#59543=CARTESIAN_POINT('Ctrl Pts',(-2.55810287525025,12.1165053344617,24.6770383679527));
#59544=CARTESIAN_POINT('Ctrl Pts',(-2.47617400265685,12.1278883711933,24.6719448369763));
#59545=CARTESIAN_POINT('Ctrl Pts',(-2.39415787710936,12.1387531871149,24.6670912522717));
#59546=CARTESIAN_POINT('Ctrl Pts',(-2.35314981433562,12.1441855950756,24.6646644599195));
#59547=CARTESIAN_POINT('Ctrl Pts',(-2.31211993832262,12.1494884478784,24.6622976542637));
#59548=CARTESIAN_POINT('Ctrl Pts',(-2.27106919241763,12.1546612385219,24.6599908297852));
#59549=CARTESIAN_POINT('Ctrl Pts',(-2.23514978975077,12.159187430335,24.6579723583666));
#59550=CARTESIAN_POINT('Ctrl Pts',(-2.19921440857278,12.1636140433123,24.6559998100488));
#59551=CARTESIAN_POINT('Ctrl Pts',(-2.16326368103987,12.1679407375121,24.6540731808108));
#59552=CARTESIAN_POINT('Ctrl Pts',(-2.15812786282088,12.1685588366835,24.6537979480625));
#59553=CARTESIAN_POINT('Ctrl Pts',(-2.15095354419729,12.1694185453608,24.653415181293));
#59554=CARTESIAN_POINT('Ctrl Pts',(-2.14785528866281,12.1697889165532,24.6532502939249));
#59555=CARTESIAN_POINT('Ctrl Pts',(-2.07187460693358,12.1788717876642,24.6492066459772));
#59556=CARTESIAN_POINT('Ctrl Pts',(-1.98856296642531,12.1882955082351,24.6450211910771));
#59557=CARTESIAN_POINT('Ctrl Pts',(-1.89789453975114,12.1977714412891,24.6408247447902));
#59558=CARTESIAN_POINT('Ctrl Pts',(-1.80764463495196,12.2072036338106,24.6366476691336));
#59559=CARTESIAN_POINT('Ctrl Pts',(-1.71010570450369,12.2166876251517,24.6324597596906));
#59560=CARTESIAN_POINT('Ctrl Pts',(-1.60525227702567,12.2258907031711,24.6284092714104));
#59561=CARTESIAN_POINT('Ctrl Pts',(-1.54053826031317,12.2315707096246,24.6259093687123));
#59562=CARTESIAN_POINT('Ctrl Pts',(-1.47303802030777,12.2371427568608,24.6234621923046));
#59563=CARTESIAN_POINT('Ctrl Pts',(-1.40274556876306,12.2425193369782,24.6211060655178));
#59564=CARTESIAN_POINT('Ctrl Pts',(-1.28716646499202,12.2513598354625,24.617231979234));
#59565=CARTESIAN_POINT('Ctrl Pts',(-1.16403957039885,12.2596745372903,24.613603241472));
#59566=CARTESIAN_POINT('Ctrl Pts',(-1.0333545078798,12.2670275652562,24.6104067966571));
#59567=CARTESIAN_POINT('Ctrl Pts',(-0.995223826797064,12.2691729976335,
24.6094741528225));
#59568=CARTESIAN_POINT('Ctrl Pts',(-0.956449697259837,12.2712362342796,
24.6085784122977));
#59569=CARTESIAN_POINT('Ctrl Pts',(-0.917031861504277,12.273205652951,24.6077244509902));
#59570=CARTESIAN_POINT('Ctrl Pts',(-0.829774683487843,12.277565250892,24.6058340820138));
#59571=CARTESIAN_POINT('Ctrl Pts',(-0.739363747682051,12.2814654079063,
24.6041484487088));
#59572=CARTESIAN_POINT('Ctrl Pts',(-0.645800341501278,12.2847716669504,
24.6027230440238));
#59573=CARTESIAN_POINT('Ctrl Pts',(-0.599018638410892,12.2864247964724,
24.6020103416812));
#59574=CARTESIAN_POINT('Ctrl Pts',(-0.551448817581928,12.2879294374135,
24.6013626681618));
#59575=CARTESIAN_POINT('Ctrl Pts',(-0.503092201724354,12.2892678057657,
24.6007872112589));
#59576=CARTESIAN_POINT('Ctrl Pts',(-0.478913893795567,12.2899369899417,
24.6004994828075));
#59577=CARTESIAN_POINT('Ctrl Pts',(-0.454538887106797,12.2905646049275,
24.6002298064347));
#59578=CARTESIAN_POINT('Ctrl Pts',(-0.429967428839181,12.291148405519,24.5999790751891));
#59579=CARTESIAN_POINT('Ctrl Pts',(-0.417681699705374,12.2914403058147,
24.5998537095663));
#59580=CARTESIAN_POINT('Ctrl Pts',(-0.405346857677343,12.2917212524407,
24.5997330800844));
#59581=CARTESIAN_POINT('Ctrl Pts',(-0.39296293297194,12.291990960342,24.5996172994885));
#59582=CARTESIAN_POINT('Ctrl Pts',(-0.386770970619239,12.2921258142927,
24.5995594091905));
#59583=CARTESIAN_POINT('Ctrl Pts',(-0.380566737597225,12.2922578585576,
24.5995027311048));
#59584=CARTESIAN_POINT('Ctrl Pts',(-0.374350237930138,12.292387057274,24.5994472793692));
#59585=CARTESIAN_POINT('Ctrl Pts',(-0.36813373826305,12.2925162559905,24.5993918276337));
#59586=CARTESIAN_POINT('Ctrl Pts',(-0.359901584797702,12.2926822439143,
24.5993205939438));
#59587=CARTESIAN_POINT('Ctrl Pts',(-0.355663943074357,12.2927660808317,
24.5992846173454));
#59588=CARTESIAN_POINT('Ctrl Pts',(-0.236599314602959,12.2951216389641,
24.5982737861797));
#59589=CARTESIAN_POINT('Ctrl Pts',(-0.118032132646121,12.2962965905457,
24.5977734526346));
#59590=CARTESIAN_POINT('Ctrl Pts',(-6.22613072209788E-13,12.2963134975005,
24.5977650017124));
#59591=CARTESIAN_POINT('Ctrl Pts',(0.150825086921002,12.2963351017271,24.5977542028642));
#59592=CARTESIAN_POINT('Ctrl Pts',(0.300776517831056,12.2944653694354,24.5985470676585));
#59593=CARTESIAN_POINT('Ctrl Pts',(0.449775834204791,12.2907821275701,24.6001284130191));
#59594=CARTESIAN_POINT('Ctrl Pts',(0.582577156369656,12.287499297813,24.6015378473695));
#59595=CARTESIAN_POINT('Ctrl Pts',(0.714626434474783,12.2827727566975,24.6035750839994));
#59596=CARTESIAN_POINT('Ctrl Pts',(0.845889638816335,12.2766488845794,24.6062309232188));
#59597=CARTESIAN_POINT('Ctrl Pts',(0.911521240987111,12.2735869485203,24.6075588428285));
#59598=CARTESIAN_POINT('Ctrl Pts',(0.976956324341615,12.270175664687,24.6090413829613));
#59599=CARTESIAN_POINT('Ctrl Pts',(1.04219086193149,12.2664207372365,24.6106772326368));
#59600=CARTESIAN_POINT('Ctrl Pts',(1.07480813072642,12.2645432735113,24.6114951574745));
#59601=CARTESIAN_POINT('Ctrl Pts',(1.1073752630609,12.2625798981021,24.6123514080813));
#59602=CARTESIAN_POINT('Ctrl Pts',(1.13989176180785,12.2605313191956,24.613245811462));
#59603=CARTESIAN_POINT('Ctrl Pts',(1.15615001118132,12.2595070297423,24.6136930131524));
#59604=CARTESIAN_POINT('Ctrl Pts',(1.17239560215684,12.2584614393706,24.6141497529425));
#59605=CARTESIAN_POINT('Ctrl Pts',(1.18862847336251,12.2573946363024,24.6146160086764));
#59606=CARTESIAN_POINT('Ctrl Pts',(1.19674490896535,12.2568612347683,24.6148491365434));
#59607=CARTESIAN_POINT('Ctrl Pts',(1.20485816462567,12.2563225300575,24.6150846433906));
#59608=CARTESIAN_POINT('Ctrl Pts',(1.21296823271956,12.2557785331572,24.6153225264273));
#59609=CARTESIAN_POINT('Ctrl Pts',(1.2170232667665,12.2555065347071,24.6154414679457));
#59610=CARTESIAN_POINT('Ctrl Pts',(1.22107750392184,12.2552332132094,24.615561003511));
#59611=CARTESIAN_POINT('Ctrl Pts',(1.22513094323861,12.2549585701678,24.6156811327076));
#59612=CARTESIAN_POINT('Ctrl Pts',(1.22715766289699,12.254821248647,24.6157411973059));
#59613=CARTESIAN_POINT('Ctrl Pts',(1.22918418309573,12.2546835967402,24.6158014103119));
#59614=CARTESIAN_POINT('Ctrl Pts',(1.23121050371738,12.2545456146664,24.6158617716582));
#59615=CARTESIAN_POINT('Ctrl Pts',(1.23323682433902,12.2544076325926,24.6159221330045));
#59616=CARTESIAN_POINT('Ctrl Pts',(1.23664151732613,12.2541749789446,24.6160239184199));
#59617=CARTESIAN_POINT('Ctrl Pts',(1.23728886673302,12.2541306781364,24.6160433006635));
#59618=CARTESIAN_POINT('Ctrl Pts',(1.27899082428633,12.2512768400026,24.6172918960758));
#59619=CARTESIAN_POINT('Ctrl Pts',(1.329632197791,12.2476963537022,24.6188585341755));
#59620=CARTESIAN_POINT('Ctrl Pts',(1.3891670989942,12.243136392662,24.6208588486595));
#59621=CARTESIAN_POINT('Ctrl Pts',(1.45035959118757,12.238449471634,24.6229148565803));
#59622=CARTESIAN_POINT('Ctrl Pts',(1.52094773855851,12.23272755589,24.625429066743));
#59623=CARTESIAN_POINT('Ctrl Pts',(1.60088171223753,12.2256437990597,24.6285505871955));
#59624=CARTESIAN_POINT('Ctrl Pts',(1.68763810646718,12.2179554386303,24.6319385316014));
#59625=CARTESIAN_POINT('Ctrl Pts',(1.78540375455881,12.2086627108728,24.6360417972231));
#59626=CARTESIAN_POINT('Ctrl Pts',(1.89411494890352,12.1972887482862,24.641079110611));
#59627=CARTESIAN_POINT('Ctrl Pts',(1.97505001713986,12.1888208766599,24.6448293711544));
#59628=CARTESIAN_POINT('Ctrl Pts',(2.06205192313041,12.1791979832714,24.6490980028743));
#59629=CARTESIAN_POINT('Ctrl Pts',(2.15509437759377,12.1682070553229,24.6539839983181));
#59630=CARTESIAN_POINT('Ctrl Pts',(2.28390882697447,12.1529904497419,24.6607485104582));
#59631=CARTESIAN_POINT('Ctrl Pts',(2.42428242791866,12.1351252395717,24.6687090764788));
#59632=CARTESIAN_POINT('Ctrl Pts',(2.57602975677601,12.1138166138051,24.6782447930643));
#59633=CARTESIAN_POINT('Ctrl Pts',(2.68650546919738,12.0983034207228,24.6851870245432));
#59634=CARTESIAN_POINT('Ctrl Pts',(2.80300947452861,12.0809646523758,24.6929643411522));
#59635=CARTESIAN_POINT('Ctrl Pts',(2.92547022396319,12.0615113539224,24.7017176516046));
#59636=CARTESIAN_POINT('Ctrl Pts',(3.04051821297009,12.0432355971843,24.7099411090744));
#59637=CARTESIAN_POINT('Ctrl Pts',(3.16081857299903,12.0230822496991,24.71903140512));
#59638=CARTESIAN_POINT('Ctrl Pts',(3.28628241049585,12.0007593860875,24.7291338183826));
#59639=CARTESIAN_POINT('Ctrl Pts',(3.31931172104303,11.9948827222676,24.7317933555973));
#59640=CARTESIAN_POINT('Ctrl Pts',(3.35269888418365,11.98885595359,24.7345229380971));
#59641=CARTESIAN_POINT('Ctrl Pts',(3.38644227805871,11.9826743497142,24.7373249864784));
#59642=CARTESIAN_POINT('Ctrl Pts',(3.46740213813978,11.9678429493306,24.7440478859512));
#59643=CARTESIAN_POINT('Ctrl Pts',(3.55041195750174,11.952116979161,24.7511894115549));
#59644=CARTESIAN_POINT('Ctrl Pts',(3.6354448591658,11.9354211828935,24.7587882878275));
#59645=CARTESIAN_POINT('Ctrl Pts',(3.67796130999782,11.9270732847597,24.7625877259637));
#59646=CARTESIAN_POINT('Ctrl Pts',(3.72098353143885,11.9184829356168,24.7665015135186));
#59647=CARTESIAN_POINT('Ctrl Pts',(3.7645077837846,11.9096404763391,24.7705347060947));
#59648=CARTESIAN_POINT('Ctrl Pts',(3.78626990995747,11.9052192467003,24.7725513023827));
#59649=CARTESIAN_POINT('Ctrl Pts',(3.80815754385888,11.900734989943,24.7745977508124));
#59650=CARTESIAN_POINT('Ctrl Pts',(3.8301702057321,11.8961864945343,24.7766746921987));
#59651=CARTESIAN_POINT('Ctrl Pts',(3.84117653666871,11.8939122468299,24.7777131628918));
#59652=CARTESIAN_POINT('Ctrl Pts',(3.85221412459836,11.8916219394916,24.7787592568861));
#59653=CARTESIAN_POINT('Ctrl Pts',(3.86328290819419,11.889315420327,24.7798130551019));
#59654=CARTESIAN_POINT('Ctrl Pts',(3.86881729999211,11.8881621607447,24.7803399542098));
#59655=CARTESIAN_POINT('Ctrl Pts',(3.87435949070658,11.8870048482077,24.7808687793772));
#59656=CARTESIAN_POINT('Ctrl Pts',(3.87990947258041,11.8858434636443,24.7813995407716));
#59657=CARTESIAN_POINT('Ctrl Pts',(3.88545945445423,11.8846820790809,24.7819303021661));
#59658=CARTESIAN_POINT('Ctrl Pts',(3.89320613467674,11.8830566448808,24.7826732727751));
#59659=CARTESIAN_POINT('Ctrl Pts',(3.89658278389481,11.8823470747937,24.7829976438288));
#59660=CARTESIAN_POINT('Ctrl Pts',(4.05478128241934,11.8491031945051,24.7981946661861));
#59661=CARTESIAN_POINT('Ctrl Pts',(4.20725187154444,11.8150833635526,24.813808149887));
#59662=CARTESIAN_POINT('Ctrl Pts',(4.35406646400287,11.7807204817787,24.829644840975));
#59663=CARTESIAN_POINT('Ctrl Pts',(4.49799162540886,11.7470338895751,24.8451698530518));
#59664=CARTESIAN_POINT('Ctrl Pts',(4.63648122865026,11.7130177567802,24.8609093236835));
#59665=CARTESIAN_POINT('Ctrl Pts',(4.7696030235706,11.6790336138896,24.876700411352));
#59666=CARTESIAN_POINT('Ctrl Pts',(4.9002562079937,11.6456796729275,24.8921986690988));
#59667=CARTESIAN_POINT('Ctrl Pts',(5.02573881948381,11.6123566061781,24.9077466533623));
#59668=CARTESIAN_POINT('Ctrl Pts',(5.14611490828662,11.5793596951519,24.9232094066191));
#59669=CARTESIAN_POINT('Ctrl Pts',(5.26571077368129,11.5465766551913,24.938571937297));
#59670=CARTESIAN_POINT('Ctrl Pts',(5.380266098206,11.5141156414518,24.9538503395685));
#59671=CARTESIAN_POINT('Ctrl Pts',(5.48984369472711,11.4822186912238,24.9689311707428));
#59672=CARTESIAN_POINT('Ctrl Pts',(5.59891528315245,11.4504690349279,24.9839423615626));
#59673=CARTESIAN_POINT('Ctrl Pts',(5.70305500979413,11.4192782828121,24.9987578168915));
#59674=CARTESIAN_POINT('Ctrl Pts',(5.80232482135773,11.3888369471314,25.0132843278572));
#59675=CARTESIAN_POINT('Ctrl Pts',(5.86641621843993,11.3691831601231,25.0226630540566));
#59676=CARTESIAN_POINT('Ctrl Pts',(5.92847766024371,11.3498407748922,25.0319217160901));
#59677=CARTESIAN_POINT('Ctrl Pts',(5.98852581792974,11.3308502649382,25.0410393365944));
#59678=CARTESIAN_POINT('Origin',(-5.98852353411075,-4.75229019515312,-11.473043446859));
#59679=CARTESIAN_POINT('Ctrl Pts',(-6.39567215186926,11.8440001009078,24.265774917167));
#59680=CARTESIAN_POINT('Ctrl Pts',(-6.35564925265182,11.85659016276,24.2594187697523));
#59681=CARTESIAN_POINT('Ctrl Pts',(-5.98524772032908,11.9719915346492,24.201263545813));
#59682=CARTESIAN_POINT('Ctrl Pts',(-5.25616196134156,12.1789688183688,24.0987560784236));
#59683=CARTESIAN_POINT('Ctrl Pts',(-4.17575456655968,12.4300259295094,23.9769539472116));
#59684=CARTESIAN_POINT('Ctrl Pts',(-3.01936369311187,12.6350416910811,23.8792984905102));
#59685=CARTESIAN_POINT('Ctrl Pts',(-1.83578568452794,12.7756187374379,23.8136687753784));
#59686=CARTESIAN_POINT('Ctrl Pts',(-0.697928666899182,12.8441379077251,
23.7825584029238));
#59687=CARTESIAN_POINT('Ctrl Pts',(0.331398824709615,12.8512035850883,23.7794557664846));
#59688=CARTESIAN_POINT('Ctrl Pts',(1.24579451141582,12.8144580444262,23.7959563368043));
#59689=CARTESIAN_POINT('Ctrl Pts',(2.07028251458803,12.7465829770363,23.8272311099001));
#59690=CARTESIAN_POINT('Ctrl Pts',(2.81704923736738,12.6564423117063,23.8693916417645));
#59691=CARTESIAN_POINT('Ctrl Pts',(3.49016613607229,12.5517067197984,23.9189795923457));
#59692=CARTESIAN_POINT('Ctrl Pts',(4.0949553302766,12.4387818440348,23.9729931464066));
#59693=CARTESIAN_POINT('Ctrl Pts',(4.65003900301249,12.3195562907933,24.0305528564122));
#59694=CARTESIAN_POINT('Ctrl Pts',(5.180490898606,12.1916432061588,24.092883824788));
#59695=CARTESIAN_POINT('Ctrl Pts',(5.70541362588262,12.0514986413341,24.1618778453152));
#59696=CARTESIAN_POINT('Ctrl Pts',(6.10977777422788,11.9329745555922,24.2209465726705));
#59697=CARTESIAN_POINT('Ctrl Pts',(6.34031405438408,11.8614134775702,24.2569833946951));
#59698=CARTESIAN_POINT('Ctrl Pts',(6.39541676810711,11.8440802193301,24.2657356932574));
#59699=CARTESIAN_POINT('Ctrl Pts',(-6.33011224179481,11.8152698388501,24.6389123673273));
#59700=CARTESIAN_POINT('Ctrl Pts',(-6.29056405060346,11.8278254058075,24.6326369136256));
#59701=CARTESIAN_POINT('Ctrl Pts',(-5.92452851936487,11.9429205323235,24.5752163287446));
#59702=CARTESIAN_POINT('Ctrl Pts',(-5.20357136152678,12.1495103384449,24.4739420826815));
#59703=CARTESIAN_POINT('Ctrl Pts',(-4.13460886818725,12.4003002415022,24.3535497596591));
#59704=CARTESIAN_POINT('Ctrl Pts',(-2.9900914803837,12.6052169620649,24.2569987045062));
#59705=CARTESIAN_POINT('Ctrl Pts',(-1.81832885962656,12.745786877442,24.1920958956842));
#59706=CARTESIAN_POINT('Ctrl Pts',(-0.691524096675534,12.8143243855958,
24.1613192188688));
#59707=CARTESIAN_POINT('Ctrl Pts',(0.32839667136552,12.8213935876436,24.1582483778528));
#59708=CARTESIAN_POINT('Ctrl Pts',(1.23407752119641,12.7846352465759,24.1745745145462));
#59709=CARTESIAN_POINT('Ctrl Pts',(2.05048413456686,12.7167522286949,24.2055078846837));
#59710=CARTESIAN_POINT('Ctrl Pts',(2.78978431718345,12.6266205777662,24.2472006090323));
#59711=CARTESIAN_POINT('Ctrl Pts',(3.45605929775469,12.5219212851974,24.2962312061184));
#59712=CARTESIAN_POINT('Ctrl Pts',(4.05460643170645,12.4090658151592,24.3496307103682));
#59713=CARTESIAN_POINT('Ctrl Pts',(4.60386797000098,12.2899482805146,24.4065282055716));
#59714=CARTESIAN_POINT('Ctrl Pts',(5.12864846123703,12.1621933780158,24.4681316577684));
#59715=CARTESIAN_POINT('Ctrl Pts',(5.64781590092389,12.0222780918086,24.5363045861396));
#59716=CARTESIAN_POINT('Ctrl Pts',(6.04758532775613,11.9040090244283,24.5946499786562));
#59717=CARTESIAN_POINT('Ctrl Pts',(6.27541087928418,11.8326354722664,24.6302324927227));
#59718=CARTESIAN_POINT('Ctrl Pts',(6.32985956424417,11.8153497944645,24.6388735577287));
#59719=CARTESIAN_POINT('Ctrl Pts',(-6.21909721196556,11.6041667995241,24.9345589552791));
#59720=CARTESIAN_POINT('Ctrl Pts',(-6.18025379385954,11.6165919593275,24.9284549741306));
#59721=CARTESIAN_POINT('Ctrl Pts',(-5.82072765592081,11.7304974169554,24.8726034547386));
#59722=CARTESIAN_POINT('Ctrl Pts',(-5.11236921789459,11.9350420954516,24.7741000987782));
#59723=CARTESIAN_POINT('Ctrl Pts',(-4.06203918887106,12.1834236616043,24.6570690059104));
#59724=CARTESIAN_POINT('Ctrl Pts',(-2.93761905916863,12.3863982267026,24.5632789748405));
#59725=CARTESIAN_POINT('Ctrl Pts',(-1.78654249655019,12.5256445065243,24.5002681039227));
#59726=CARTESIAN_POINT('Ctrl Pts',(-0.679607685364788,12.5935428444393,
24.4703931528392));
#59727=CARTESIAN_POINT('Ctrl Pts',(0.322770033085937,12.6005472441068,24.4674113481417));
#59728=CARTESIAN_POINT('Ctrl Pts',(1.21259297328069,12.5641298285676,24.483260547359));
#59729=CARTESIAN_POINT('Ctrl Pts',(2.01460081624777,12.4968834095009,24.5132884775637));
#59730=CARTESIAN_POINT('Ctrl Pts',(2.74085389058468,12.4076008364804,24.5537690843015));
#59731=CARTESIAN_POINT('Ctrl Pts',(3.39540207428237,12.3038918865634,24.6013888811208));
#59732=CARTESIAN_POINT('Ctrl Pts',(3.98345489728963,12.1921091082277,24.6532698675774));
#59733=CARTESIAN_POINT('Ctrl Pts',(4.52311935809495,12.0741314785244,24.7085682944355));
#59734=CARTESIAN_POINT('Ctrl Pts',(5.03874789287724,11.9476113810817,24.7684595170186));
#59735=CARTESIAN_POINT('Ctrl Pts',(5.54885110815234,11.8090692255007,24.8347559275283));
#59736=CARTESIAN_POINT('Ctrl Pts',(5.94159338885824,11.6919892200842,24.8915060754566));
#59737=CARTESIAN_POINT('Ctrl Pts',(6.16537079301529,11.6213520344321,24.9261162878907));
#59738=CARTESIAN_POINT('Ctrl Pts',(6.21884874455077,11.6042459796829,24.9345211260386));
#59739=CARTESIAN_POINT('Ctrl Pts',(-6.09442747551374,11.2712687731348,25.068247785561));
#59740=CARTESIAN_POINT('Ctrl Pts',(-6.05631707756792,11.2835050162748,25.0623569142849));
#59741=CARTESIAN_POINT('Ctrl Pts',(-5.70357968237373,11.3956786059711,25.0084592116254));
#59742=CARTESIAN_POINT('Ctrl Pts',(-5.00868192961402,11.5971072515952,24.9134702394146));
#59743=CARTESIAN_POINT('Ctrl Pts',(-3.9788351244146,11.8416305120833,24.8007883278658));
#59744=CARTESIAN_POINT('Ctrl Pts',(-2.87697914274819,12.0413773094681,24.7106244572076));
#59745=CARTESIAN_POINT('Ctrl Pts',(-1.74953331073714,12.1783634704876,24.6501281720072));
#59746=CARTESIAN_POINT('Ctrl Pts',(-0.665593611714366,12.2451486628473,
24.6214644543181));
#59747=CARTESIAN_POINT('Ctrl Pts',(0.316131026122826,12.2520385424126,24.6186033990537));
#59748=CARTESIAN_POINT('Ctrl Pts',(1.18749622986108,12.2162178808641,24.6338098959915));
#59749=CARTESIAN_POINT('Ctrl Pts',(1.97291294062881,12.1500698270089,24.6626279294911));
#59750=CARTESIAN_POINT('Ctrl Pts',(2.68427596727038,12.0622326265172,24.7014995980027));
#59751=CARTESIAN_POINT('Ctrl Pts',(3.32557172596527,11.9601837655491,24.747259581196));
#59752=CARTESIAN_POINT('Ctrl Pts',(3.90188404781945,11.8501690615632,24.7971528788433));
#59753=CARTESIAN_POINT('Ctrl Pts',(4.43092541213141,11.7340360652914,24.8503737539427));
#59754=CARTESIAN_POINT('Ctrl Pts',(4.93654273176015,11.6094730471387,24.9080588205053));
#59755=CARTESIAN_POINT('Ctrl Pts',(5.43686879684977,11.4730538901245,24.9719611389093));
#59756=CARTESIAN_POINT('Ctrl Pts',(5.8221639465597,11.3577558829121,25.0267013366178));
#59757=CARTESIAN_POINT('Ctrl Pts',(6.04171502508226,11.2881926952705,25.0600999046611));
#59758=CARTESIAN_POINT('Ctrl Pts',(6.09418351640657,11.271346787654,25.0682112217091));
#59759=CARTESIAN_POINT('',(6.27159454904393,11.8794923467406,24.2690137147172));
#59760=CARTESIAN_POINT('Origin',(5.999999949012,10.9277802669415,24.1259420051707));
#59761=CARTESIAN_POINT('',(-6.27159362679375,11.8794975540956,24.2690120913865));
#59762=CARTESIAN_POINT('Ctrl Pts',(-6.27159387327999,11.8794984953294,24.2690123753742));
#59763=CARTESIAN_POINT('Ctrl Pts',(-6.13239665975347,11.9224692155082,24.2474082746545));
#59764=CARTESIAN_POINT('Ctrl Pts',(-5.98564494831062,11.9663158668838,24.2255025468638));
#59765=CARTESIAN_POINT('Ctrl Pts',(-5.83132868240695,12.0105538899393,24.203534985663));
#59766=CARTESIAN_POINT('Ctrl Pts',(-5.67907415991493,12.0542008706181,24.1818609221977));
#59767=CARTESIAN_POINT('Ctrl Pts',(-5.51945557022787,12.0982288673079,24.1601268955012));
#59768=CARTESIAN_POINT('Ctrl Pts',(-5.35247255846345,12.1421228213731,24.1385690083634));
#59769=CARTESIAN_POINT('Ctrl Pts',(-5.32566531741069,12.1491695011218,24.1351081324875));
#59770=CARTESIAN_POINT('Ctrl Pts',(-5.29866830053705,12.1562126203553,24.1316518043049));
#59771=CARTESIAN_POINT('Ctrl Pts',(-5.27148153698936,12.1632499256716,24.128201008766));
#59772=CARTESIAN_POINT('Ctrl Pts',(-5.14595062003312,12.1957436569577,24.1122674634778));
#59773=CARTESIAN_POINT('Ctrl Pts',(-5.01637391730844,12.2281146709243,24.0964515384637));
#59774=CARTESIAN_POINT('Ctrl Pts',(-4.88275740018152,12.2601325340667,24.0808623975426));
#59775=CARTESIAN_POINT('Ctrl Pts',(-4.71106411325276,12.3012745446621,24.0608308108594));
#59776=CARTESIAN_POINT('Ctrl Pts',(-4.53269557213984,12.3418362253296,24.0411729460729));
#59777=CARTESIAN_POINT('Ctrl Pts',(-4.34764559027276,12.3812950570725,24.0221340647503));
#59778=CARTESIAN_POINT('Ctrl Pts',(-4.2958379438806,12.3923421762419,24.016803831149));
#59779=CARTESIAN_POINT('Ctrl Pts',(-4.2435067021697,12.4033025668906,24.0115221856858));
#59780=CARTESIAN_POINT('Ctrl Pts',(-4.19065197808048,12.4141640869762,24.0062946755803));
#59781=CARTESIAN_POINT('Ctrl Pts',(-4.14337959060077,12.4238784501661,24.0016192773539));
#59782=CARTESIAN_POINT('Ctrl Pts',(-4.09568845748379,12.4335137197591,23.9969871831794));
#59783=CARTESIAN_POINT('Ctrl Pts',(-4.04757900720712,12.4430611393021,23.9924025369345));
#59784=CARTESIAN_POINT('Ctrl Pts',(-3.90056248959711,12.4722368701677,23.9783924262074));
#59785=CARTESIAN_POINT('Ctrl Pts',(-3.74963598878708,12.5005941082547,23.9648249569629));
#59786=CARTESIAN_POINT('Ctrl Pts',(-3.59479968040675,12.5278747688691,23.951821468078));
#59787=CARTESIAN_POINT('Ctrl Pts',(-3.51738152621659,12.5415150991762,23.9453197236355));
#59788=CARTESIAN_POINT('Ctrl Pts',(-3.43898591152213,12.5548860349274,23.93895906991));
#59789=CARTESIAN_POINT('Ctrl Pts',(-3.35961280896348,12.5679537407706,23.9327552496512));
#59790=CARTESIAN_POINT('Ctrl Pts',(-3.31992625768416,12.5744875936921,23.9296533395218));
#59791=CARTESIAN_POINT('Ctrl Pts',(-3.2799953320476,12.5809456233232,23.9265906359475));
#59792=CARTESIAN_POINT('Ctrl Pts',(-3.23982002808293,12.5873234942267,23.9235691515302));
#59793=CARTESIAN_POINT('Ctrl Pts',(-3.2197323761006,12.5905124296784,23.9220584093215));
#59794=CARTESIAN_POINT('Ctrl Pts',(-3.19958362938644,12.5936813244136,23.9205579717845));
#59795=CARTESIAN_POINT('Ctrl Pts',(-3.17937378695259,12.5968296299603,23.9190680913502));
#59796=CARTESIAN_POINT('Ctrl Pts',(-3.16169017482297,12.5995843973137,23.9177644459701));
#59797=CARTESIAN_POINT('Ctrl Pts',(-3.14395978627424,12.6023234010082,23.9164688833649));
#59798=CARTESIAN_POINT('Ctrl Pts',(-3.12618262055138,12.6050462707541,23.9151815734085));
#59799=CARTESIAN_POINT('Ctrl Pts',(-3.12364302544811,12.6054352521464,23.9149976719862));
#59800=CARTESIAN_POINT('Ctrl Pts',(-3.11986205084656,12.6060134313777,23.9147243474001));
#59801=CARTESIAN_POINT('Ctrl Pts',(-3.11856097133547,12.6062122260373,23.9146303749287));
#59802=CARTESIAN_POINT('Ctrl Pts',(-3.09161078795331,12.6103300009199,23.9126838564297));
#59803=CARTESIAN_POINT('Ctrl Pts',(-3.06343524023067,12.6145814696381,23.9106763719954));
#59804=CARTESIAN_POINT('Ctrl Pts',(-3.03403435500432,12.6189513764305,23.9086151433588));
#59805=CARTESIAN_POINT('Ctrl Pts',(-2.9619677253846,12.6296627700452,23.9035627172304));
#59806=CARTESIAN_POINT('Ctrl Pts',(-2.88253900653253,12.6410890424655,23.898185873917));
#59807=CARTESIAN_POINT('Ctrl Pts',(-2.79574783276679,12.6529730518689,23.892606171807));
#59808=CARTESIAN_POINT('Ctrl Pts',(-2.70928691593848,12.6648118403543,23.8870477015258));
#59809=CARTESIAN_POINT('Ctrl Pts',(-2.61551922198365,12.6771049175497,23.8812879491854));
#59810=CARTESIAN_POINT('Ctrl Pts',(-2.51444548334207,12.689550941705,23.8754684237424));
#59811=CARTESIAN_POINT('Ctrl Pts',(-2.50258801369576,12.6910110475211,23.8747857058848));
#59812=CARTESIAN_POINT('Ctrl Pts',(-2.49062999607805,12.6924732044915,23.8741021892436));
#59813=CARTESIAN_POINT('Ctrl Pts',(-2.47857143521673,12.6939368830162,23.8734181212848));
#59814=CARTESIAN_POINT('Ctrl Pts',(-2.37688557180676,12.7062796008792,23.8676496019884));
#59815=CARTESIAN_POINT('Ctrl Pts',(-2.26804971895943,12.7187343238039,23.8618405702272));
#59816=CARTESIAN_POINT('Ctrl Pts',(-2.1520626700025,12.7309579651534,23.8561524935622));
#59817=CARTESIAN_POINT('Ctrl Pts',(-2.11969727196408,12.7343688892291,23.8545652744115));
#59818=CARTESIAN_POINT('Ctrl Pts',(-2.08677509095584,12.7377615371318,23.8529875939479));
#59819=CARTESIAN_POINT('Ctrl Pts',(-2.05329622092775,12.7411277927086,23.8514232396551));
#59820=CARTESIAN_POINT('Ctrl Pts',(-1.97656810089333,12.7488427024934,23.8478379942793));
#59821=CARTESIAN_POINT('Ctrl Pts',(-1.8969155054141,12.7564195734445,23.8443225602372));
#59822=CARTESIAN_POINT('Ctrl Pts',(-1.81433838927152,12.7637550206789,23.8409252157065));
#59823=CARTESIAN_POINT('Ctrl Pts',(-1.81240102804,12.7639271193396,23.8408455098038));
#59824=CARTESIAN_POINT('Ctrl Pts',(-1.81046205708854,12.7640990847574,23.8407658688772));
#59825=CARTESIAN_POINT('Ctrl Pts',(-1.80852147639801,12.7642709155407,23.8406862936122));
#59826=CARTESIAN_POINT('Ctrl Pts',(-1.76910488671214,12.7677610994404,23.83906998073));
#59827=CARTESIAN_POINT('Ctrl Pts',(-1.72902415885956,12.7711957707857,23.8374807465779));
#59828=CARTESIAN_POINT('Ctrl Pts',(-1.6882793161297,12.7745632609372,23.8359241922724));
#59829=CARTESIAN_POINT('Ctrl Pts',(-1.66690390775258,12.7763299011392,23.8351075985218));
#59830=CARTESIAN_POINT('Ctrl Pts',(-1.64534571912912,12.7780780455687,23.8342999980866));
#59831=CARTESIAN_POINT('Ctrl Pts',(-1.62360475111848,12.7798059673452,23.8335022084597));
#59832=CARTESIAN_POINT('Ctrl Pts',(-1.61273426711316,12.7806699282335,23.8331033136463));
#59833=CARTESIAN_POINT('Ctrl Pts',(-1.60181808822608,12.7815288330184,23.8327068714887));
#59834=CARTESIAN_POINT('Ctrl Pts',(-1.59085621455979,12.7823824630006,23.8323129855334));
#59835=CARTESIAN_POINT('Ctrl Pts',(-1.58537527772664,12.7828092779917,23.8321160425557));
#59836=CARTESIAN_POINT('Ctrl Pts',(-1.57988291719653,12.7832347742544,23.8319197386257));
#59837=CARTESIAN_POINT('Ctrl Pts',(-1.5743791329824,12.7836589242724,23.8317240867766));
#59838=CARTESIAN_POINT('Ctrl Pts',(-1.56887534876828,12.7840830742904,23.8315284349275));
#59839=CARTESIAN_POINT('Ctrl Pts',(-1.56205962342448,12.7846050482238,23.831287704659));
#59840=CARTESIAN_POINT('Ctrl Pts',(-1.55783350929622,12.7849273079608,23.8311391005259));
#59841=CARTESIAN_POINT('Ctrl Pts',(-1.33210029545101,12.8021404555285,23.8232015750512));
#59842=CARTESIAN_POINT('Ctrl Pts',(-1.11005370632018,12.8153351626569,23.817122034248));
#59843=CARTESIAN_POINT('Ctrl Pts',(-0.891696800345942,12.8248709230765,
23.8127291041508));
#59844=CARTESIAN_POINT('Ctrl Pts',(-0.84842062124671,12.8267608164779,23.811858468854));
#59845=CARTESIAN_POINT('Ctrl Pts',(-0.805289264854227,12.8285068913263,
23.8110541618022));
#59846=CARTESIAN_POINT('Ctrl Pts',(-0.762302602899293,12.8301118023318,
23.8103149645275));
#59847=CARTESIAN_POINT('Ctrl Pts',(-0.724718063253752,12.8315150246005,
23.8096686619766));
#59848=CARTESIAN_POINT('Ctrl Pts',(-0.687244120817588,12.8328103362796,
23.8090721006341));
#59849=CARTESIAN_POINT('Ctrl Pts',(-0.649880973381661,12.8339994885111,
23.8085243488097));
#59850=CARTESIAN_POINT('Ctrl Pts',(-0.558068160819892,12.8369216034407,
23.8071783531151));
#59851=CARTESIAN_POINT('Ctrl Pts',(-0.466924415806544,12.8392027555537,
23.8061270509237));
#59852=CARTESIAN_POINT('Ctrl Pts',(-0.376448972902625,12.8408704266499,
23.8053581698283));
#59853=CARTESIAN_POINT('Ctrl Pts',(-0.312801798465681,12.8420435908783,
23.8048172815206));
#59854=CARTESIAN_POINT('Ctrl Pts',(-0.249485511111982,12.8429131416853,
23.8044160900822));
#59855=CARTESIAN_POINT('Ctrl Pts',(-0.18650011116102,12.8434883988289,23.8041502792515));
#59856=CARTESIAN_POINT('Ctrl Pts',(-0.155007411185538,12.8437760274007,
23.8040173738361));
#59857=CARTESIAN_POINT('Ctrl Pts',(-0.123597432937689,12.8439900795162,
23.8039183132638));
#59858=CARTESIAN_POINT('Ctrl Pts',(-0.0922701760386044,12.8441317020175,
23.8038525590397));
#59859=CARTESIAN_POINT('Ctrl Pts',(-0.0647193034850948,12.8442562524528,
23.8037947312428));
#59860=CARTESIAN_POINT('Ctrl Pts',(-0.0383382064328693,12.8443236938424,
23.8037631762405));
#59861=CARTESIAN_POINT('Ctrl Pts',(-0.0102093966394934,12.8443378683841,
23.8037560877189));
#59862=CARTESIAN_POINT('Ctrl Pts',(-0.00635379472499661,12.8443398112815,
23.8037551160988));
#59863=CARTESIAN_POINT('Ctrl Pts',(-0.0024653565932188,12.844340680764,
23.803754636878));
#59864=CARTESIAN_POINT('Ctrl Pts',(0.00146343106551837,12.8443404157949,
23.8037546773412));
#59865=CARTESIAN_POINT('Ctrl Pts',(0.123994138919106,12.8443321519592,23.8037559393069));
#59866=CARTESIAN_POINT('Ctrl Pts',(0.24652145032575,12.8432200851129,23.8042791685664));
#59867=CARTESIAN_POINT('Ctrl Pts',(0.36905046775366,12.8410042079906,23.8053127231307));
#59868=CARTESIAN_POINT('Ctrl Pts',(0.644865199825655,12.8360162339772,23.8076392705984));
#59869=CARTESIAN_POINT('Ctrl Pts',(0.920688389422045,12.8254382930282,23.8125501318452));
#59870=CARTESIAN_POINT('Ctrl Pts',(1.19650944973774,12.8092731224474,23.8200734126678));
#59871=CARTESIAN_POINT('Ctrl Pts',(1.22210575983819,12.8077729878364,23.820771576284));
#59872=CARTESIAN_POINT('Ctrl Pts',(1.24770205338369,12.8062247032809,23.8214922543273));
#59873=CARTESIAN_POINT('Ctrl Pts',(1.27329832267905,12.8046282506351,23.8222354795427));
#59874=CARTESIAN_POINT('Ctrl Pts',(1.37081820380044,12.798545884864,23.8250671123017));
#59875=CARTESIAN_POINT('Ctrl Pts',(1.46833773422664,12.7917643882597,23.8282260014275));
#59876=CARTESIAN_POINT('Ctrl Pts',(1.56585686708111,12.7842847837547,23.8317101403452));
#59877=CARTESIAN_POINT('Ctrl Pts',(1.7401743530888,12.7709148345407,23.8379381114033));
#59878=CARTESIAN_POINT('Ctrl Pts',(1.91449222409226,12.7553144041715,23.8452066434151));
#59879=CARTESIAN_POINT('Ctrl Pts',(2.08880964225459,12.737482741405,23.8535154632649));
#59880=CARTESIAN_POINT('Ctrl Pts',(2.17522432420784,12.7286430196898,23.8576344092216));
#59881=CARTESIAN_POINT('Ctrl Pts',(2.26163887766306,12.7192548608822,23.8620090644269));
#59882=CARTESIAN_POINT('Ctrl Pts',(2.3480535937233,12.7093187481637,23.8666392624854));
#59883=CARTESIAN_POINT('Ctrl Pts',(2.47841969523524,12.6943290295331,23.8736244254025));
#59884=CARTESIAN_POINT('Ctrl Pts',(2.60878583587792,12.6780923252995,23.8811913884638));
#59885=CARTESIAN_POINT('Ctrl Pts',(2.73915198832477,12.6606086880375,23.8893399954516));
#59886=CARTESIAN_POINT('Ctrl Pts',(2.77253967456891,12.6561310058757,23.8914269108689));
#59887=CARTESIAN_POINT('Ctrl Pts',(2.80592736751217,12.6515715264161,23.8935519669626));
#59888=CARTESIAN_POINT('Ctrl Pts',(2.83931504872826,12.6469302299745,23.8957151760613));
#59889=CARTESIAN_POINT('Ctrl Pts',(2.87111043391928,12.6425102821742,23.8977752192879));
#59890=CARTESIAN_POINT('Ctrl Pts',(2.90290580844884,12.6380161351086,23.8998698632239));
#59891=CARTESIAN_POINT('Ctrl Pts',(2.93470118833342,12.6334478142511,23.901999091622));
#59892=CARTESIAN_POINT('Ctrl Pts',(2.98358847997979,12.626423748651,23.9052729071906));
#59893=CARTESIAN_POINT('Ctrl Pts',(3.03247576815835,12.6192243312319,23.9086285033686));
#59894=CARTESIAN_POINT('Ctrl Pts',(3.08136305876389,12.6118496254351,23.9120658773373));
#59895=CARTESIAN_POINT('Ctrl Pts',(3.09765882229907,12.6093913901695,23.9132116686601));
#59896=CARTESIAN_POINT('Ctrl Pts',(3.11203761249439,12.6072074380347,23.9142296219463));
#59897=CARTESIAN_POINT('Ctrl Pts',(3.13025035019709,12.6044164907937,23.9155305102362));
#59898=CARTESIAN_POINT('Ctrl Pts',(3.25876627310765,12.5847225180193,23.924710066979));
#59899=CARTESIAN_POINT('Ctrl Pts',(3.38586269051035,12.56402720794,23.934421740979));
#59900=CARTESIAN_POINT('Ctrl Pts',(3.51152584085004,12.542411839432,23.9446264834151));
#59901=CARTESIAN_POINT('Ctrl Pts',(3.71378615759454,12.5076209618424,23.9610514610783));
#59902=CARTESIAN_POINT('Ctrl Pts',(3.91233263338801,12.4704476520642,23.9787535291653));
#59903=CARTESIAN_POINT('Ctrl Pts',(4.10713150515215,12.4312229146291,23.9975737301052));
#59904=CARTESIAN_POINT('Ctrl Pts',(4.29248338111171,12.3939004260449,24.015481223709));
#59905=CARTESIAN_POINT('Ctrl Pts',(4.4744426089921,12.3547205225641,24.0344011133741));
#59906=CARTESIAN_POINT('Ctrl Pts',(4.65299936796426,12.3139554246983,24.0542036567935));
#59907=CARTESIAN_POINT('Ctrl Pts',(4.83064040150767,12.2733993899727,24.0739046431917));
#59908=CARTESIAN_POINT('Ctrl Pts',(5.0049139245582,12.2312743461914,24.0944793585985));
#59909=CARTESIAN_POINT('Ctrl Pts',(5.17582589534808,12.1878340421094,24.1158100264904));
#59910=CARTESIAN_POINT('Ctrl Pts',(5.35319905371138,12.1427515127834,24.1379470828739));
#59911=CARTESIAN_POINT('Ctrl Pts',(5.52695177479932,12.0962524555958,24.1608985086487));
#59912=CARTESIAN_POINT('Ctrl Pts',(5.69710560176435,12.0486025329149,24.1845471907116));
#59913=CARTESIAN_POINT('Ctrl Pts',(5.87743847974876,11.9981020660959,24.2096105993519));
#59914=CARTESIAN_POINT('Ctrl Pts',(6.05372901480326,11.9463090227909,24.2354575530271));
#59915=CARTESIAN_POINT('Ctrl Pts',(6.22601604554166,11.8935163209721,24.2619703523821));
#59916=CARTESIAN_POINT('Ctrl Pts',(6.24124062221443,11.8888511611329,24.2643132225614));
#59917=CARTESIAN_POINT('Ctrl Pts',(6.25643394241564,11.8841781814134,24.2666612898628));
#59918=CARTESIAN_POINT('Ctrl Pts',(6.27159604047703,11.8794975711571,24.2690144967149));
#59919=CARTESIAN_POINT('Origin',(-5.999994993362,10.9277770074801,24.1259380195517));
#59920=CARTESIAN_POINT('Origin',(5.99999999906,10.9277802195584,24.1259421376201));
#59921=CARTESIAN_POINT('Origin',(5.99996968668208,10.9277552850209,24.1259230381653));
#59922=CARTESIAN_POINT('Ctrl Pts',(6.25331147241795,8.42894521849349,13.948377678764));
#59923=CARTESIAN_POINT('Ctrl Pts',(6.30255402214553,8.40744222105348,13.9453310478153));
#59924=CARTESIAN_POINT('Ctrl Pts',(6.44286889530678,8.33601401238666,13.9419588806518));
#59925=CARTESIAN_POINT('Ctrl Pts',(6.65934670592776,8.1750683081117,13.9631279626853));
#59926=CARTESIAN_POINT('Ctrl Pts',(6.87326007648327,7.92769689971508,14.0292863828931));
#59927=CARTESIAN_POINT('Ctrl Pts',(7.02774581839624,7.63652467033211,14.1338750541619));
#59928=CARTESIAN_POINT('Ctrl Pts',(7.09502298419993,7.37242077306597,14.2481499818927));
#59929=CARTESIAN_POINT('Ctrl Pts',(7.10386618336956,7.21380101513048,14.3251097596679));
#59930=CARTESIAN_POINT('Ctrl Pts',(7.10318236346192,7.16033603230201,14.352035876389));
#59931=CARTESIAN_POINT('Ctrl Pts',(6.05603900145848,8.02832546593723,13.4854857122089));
#59932=CARTESIAN_POINT('Ctrl Pts',(6.09977809654048,8.00942840821252,13.48252913969));
#59933=CARTESIAN_POINT('Ctrl Pts',(6.22466181234398,7.94659667061775,13.4786408662298));
#59934=CARTESIAN_POINT('Ctrl Pts',(6.41837418436726,7.80451142267422,13.4954440662563));
#59935=CARTESIAN_POINT('Ctrl Pts',(6.61083155733378,7.58521226783456,13.5518110042824));
#59936=CARTESIAN_POINT('Ctrl Pts',(6.7503372588355,7.32644368001614,13.6428774049336));
#59937=CARTESIAN_POINT('Ctrl Pts',(6.81114777276548,7.09176064198665,13.7435290137315));
#59938=CARTESIAN_POINT('Ctrl Pts',(6.81910616842577,6.95129282556063,13.8115623985171));
#59939=CARTESIAN_POINT('Ctrl Pts',(6.81849079330802,6.90404543882402,13.8353666299144));
#59940=CARTESIAN_POINT('Ctrl Pts',(6.04665680408591,8.08800353272693,12.8453843521092));
#59941=CARTESIAN_POINT('Ctrl Pts',(6.10683798511585,8.0623848792519,12.841560624492));
#59942=CARTESIAN_POINT('Ctrl Pts',(6.27752443201705,7.97777606934776,12.837110603505));
#59943=CARTESIAN_POINT('Ctrl Pts',(6.53754543161355,7.78998742220227,12.8615274272874));
#59944=CARTESIAN_POINT('Ctrl Pts',(6.79117844125654,7.5057761358831,12.9376338739102));
#59945=CARTESIAN_POINT('Ctrl Pts',(6.9727101644675,7.17465351943412,13.0568546025352));
#59946=CARTESIAN_POINT('Ctrl Pts',(7.05158421179892,6.87547066530062,13.1864794295886));
#59947=CARTESIAN_POINT('Ctrl Pts',(7.06206245935511,6.69496529079826,13.2740717028483));
#59948=CARTESIAN_POINT('Ctrl Pts',(7.06125212490234,6.63390802281003,13.304820049174));
#59949=CARTESIAN_POINT('Ctrl Pts',(6.23115653270046,8.56708401712786,12.4587093936205));
#59950=CARTESIAN_POINT('Ctrl Pts',(6.31863448173896,8.52995082214717,12.4536458922549));
#59951=CARTESIAN_POINT('Ctrl Pts',(6.56546156683406,8.40788311970759,12.4489662200631));
#59952=CARTESIAN_POINT('Ctrl Pts',(6.93613642272148,8.14066201853445,12.4878374168353));
#59953=CARTESIAN_POINT('Ctrl Pts',(7.29230959064227,7.74235076973145,12.5998939031533));
#59954=CARTESIAN_POINT('Ctrl Pts',(7.54452359386327,7.28293596703667,12.7699474219303));
#59955=CARTESIAN_POINT('Ctrl Pts',(7.65380606172403,6.86885355188191,12.9515917840878));
#59956=CARTESIAN_POINT('Ctrl Pts',(7.66850900399649,6.61713607686126,13.0740309563524));
#59957=CARTESIAN_POINT('Ctrl Pts',(7.66737181947984,6.5315594617666,13.1171039874949));
#59958=CARTESIAN_POINT('',(6.9999916354347,6.97709969495907,13.9487325181045));
#59959=CARTESIAN_POINT('',(7.00000025951341,8.04447732699761,12.5220641950641));
#59960=CARTESIAN_POINT('Ctrl Pts',(7.,6.97709969493429,13.94873251817));
#59961=CARTESIAN_POINT('Ctrl Pts',(7.,7.02062865649979,13.8481984403386));
#59962=CARTESIAN_POINT('Ctrl Pts',(7.,7.06182311179943,13.7584316945066));
#59963=CARTESIAN_POINT('Ctrl Pts',(7.,7.09986953085516,13.6808089002891));
#59964=CARTESIAN_POINT('Ctrl Pts',(7.,7.11889274038302,13.6419975031804));
#59965=CARTESIAN_POINT('Ctrl Pts',(7.,7.13709521427333,13.6061961582339));
#59966=CARTESIAN_POINT('Ctrl Pts',(7.,7.15421673583155,13.5734556202725));
#59967=CARTESIAN_POINT('Ctrl Pts',(7.,7.16277749661066,13.5570853512918));
#59968=CARTESIAN_POINT('Ctrl Pts',(7.,7.17106680179347,13.5414792765318));
#59969=CARTESIAN_POINT('Ctrl Pts',(7.,7.17904737612002,13.5266383750259));
#59970=CARTESIAN_POINT('Ctrl Pts',(7.,7.1830376632833,13.5192179242729));
#59971=CARTESIAN_POINT('Ctrl Pts',(7.,7.18695076773252,13.5119887668335));
#59972=CARTESIAN_POINT('Ctrl Pts',(7.,7.1907818958336,13.5049506945816));
#59973=CARTESIAN_POINT('Ctrl Pts',(7.,7.19269745988415,13.5014316584557));
#59974=CARTESIAN_POINT('Ctrl Pts',(7.,7.19459252984766,13.4979603936266));
#59975=CARTESIAN_POINT('Ctrl Pts',(7.,7.19646651204854,13.4945368678279));
#59976=CARTESIAN_POINT('Ctrl Pts',(7.,7.19834049424942,13.4911133420292));
#59977=CARTESIAN_POINT('Ctrl Pts',(7.,7.19942602526282,13.4891321804845));
#59978=CARTESIAN_POINT('Ctrl Pts',(7.,7.20202460170296,13.4844094706777));
#59979=CARTESIAN_POINT('Ctrl Pts',(7.,7.24360182474522,13.408846113769));
#59980=CARTESIAN_POINT('Ctrl Pts',(7.,7.28586258548639,13.3375859005503));
#59981=CARTESIAN_POINT('Ctrl Pts',(7.,7.328413443107,13.2711285919118));
#59982=CARTESIAN_POINT('Ctrl Pts',(7.,7.37096430072761,13.2046712832734));
#59983=CARTESIAN_POINT('Ctrl Pts',(7.,7.41282803400312,13.144309635631));
#59984=CARTESIAN_POINT('Ctrl Pts',(7.,7.45598818177928,13.0863402094606));
#59985=CARTESIAN_POINT('Ctrl Pts',(7.,7.5423084773316,12.9704013571197));
#59986=CARTESIAN_POINT('Ctrl Pts',(7.,7.63586174972797,12.8624663289328));
#59987=CARTESIAN_POINT('Ctrl Pts',(7.,7.73521543344203,12.7672008088884));
#59988=CARTESIAN_POINT('Ctrl Pts',(7.,7.83456911715609,12.6719352888439));
#59989=CARTESIAN_POINT('Ctrl Pts',(7.,7.93954239456337,12.5894748091373));
#59990=CARTESIAN_POINT('Ctrl Pts',(7.,8.04447653888369,12.5220644911691));
#59991=CARTESIAN_POINT('',(6.24994452403135,8.55169657613351,12.4626509071323));
#59992=CARTESIAN_POINT('Ctrl Pts',(6.24994457521983,8.55169667629553,12.4626510531007));
#59993=CARTESIAN_POINT('Ctrl Pts',(6.29978446790311,8.52998434340969,12.4600718849041));
#59994=CARTESIAN_POINT('Ctrl Pts',(6.34860942389968,8.50674633505747,12.458637151969));
#59995=CARTESIAN_POINT('Ctrl Pts',(6.39644290451949,8.48204920681093,12.45829327108));
#59996=CARTESIAN_POINT('Ctrl Pts',(6.425658215371,8.46696491293324,12.4580832385477));
#59997=CARTESIAN_POINT('Ctrl Pts',(6.454503509566,8.45133541296467,12.4582806915151));
#59998=CARTESIAN_POINT('Ctrl Pts',(6.48298161554681,8.43516819850334,12.458878450293));
#59999=CARTESIAN_POINT('Ctrl Pts',(6.53032984027627,8.40828828928185,12.4598722950721));
#60000=CARTESIAN_POINT('Ctrl Pts',(6.57666452439768,8.3799238482972,12.4619712726638));
#60001=CARTESIAN_POINT('Ctrl Pts',(6.62201867977745,8.3500909877409,12.4651442021191));
#60002=CARTESIAN_POINT('Ctrl Pts',(6.63083239554454,8.34429353982768,12.465760800491));
#60003=CARTESIAN_POINT('Ctrl Pts',(6.63960900365929,8.33844052794818,12.466418038111));
#60004=CARTESIAN_POINT('Ctrl Pts',(6.64834862719593,8.33253191639426,12.4671158030968));
#60005=CARTESIAN_POINT('Ctrl Pts',(6.69477098455228,8.30114707746084,12.470822129277));
#60006=CARTESIAN_POINT('Ctrl Pts',(6.74013197243143,8.26820234249192,12.475673311407));
#60007=CARTESIAN_POINT('Ctrl Pts',(6.78442186677646,8.23368098850016,12.481666533661));
#60008=CARTESIAN_POINT('Ctrl Pts',(6.82871176112148,8.1991596345084,12.487659755915));
#60009=CARTESIAN_POINT('Ctrl Pts',(6.87193117326179,8.16306120631539,12.4947951523366));
#60010=CARTESIAN_POINT('Ctrl Pts',(6.91402897842334,8.12534103701035,12.5030954937722));
#60011=CARTESIAN_POINT('Ctrl Pts',(6.94323288792411,8.09917396234908,12.5088535711632));
#60012=CARTESIAN_POINT('Ctrl Pts',(6.97189609944987,8.07222583883693,12.5151728308876));
#60013=CARTESIAN_POINT('Ctrl Pts',(7.00000077683936,8.04447756164977,12.5220630299184));
#60014=CARTESIAN_POINT('',(6.26385807711555,8.42072586779743,13.9442710283615));
#60015=CARTESIAN_POINT('Origin',(6.52772556344856,9.09520187390111,13.2547574611158));
#60016=CARTESIAN_POINT('Ctrl Pts',(6.26385545879972,8.42071917467894,13.9442778706664));
#60017=CARTESIAN_POINT('Ctrl Pts',(6.30496680145664,8.39385467933137,13.9337310194281));
#60018=CARTESIAN_POINT('Ctrl Pts',(6.34565967410041,8.36408702383874,13.9242414338528));
#60019=CARTESIAN_POINT('Ctrl Pts',(6.38553796953683,8.3314258597232,13.9158860764687));
#60020=CARTESIAN_POINT('Ctrl Pts',(6.43022288687479,8.29482797100472,13.9065236288025));
#60021=CARTESIAN_POINT('Ctrl Pts',(6.47388545279323,8.25459587635117,13.8985855268188));
#60022=CARTESIAN_POINT('Ctrl Pts',(6.51600797558017,8.21087401920264,13.8921009540601));
#60023=CARTESIAN_POINT('Ctrl Pts',(6.52844998279364,8.1979596060565,13.8901855630601));
#60024=CARTESIAN_POINT('Ctrl Pts',(6.54075731479757,8.18474082982893,13.888397071652));
#60025=CARTESIAN_POINT('Ctrl Pts',(6.55291581058607,8.1712216559871,13.8867364803161));
#60026=CARTESIAN_POINT('Ctrl Pts',(6.57257265518867,8.14936498029407,13.8840517743783));
#60027=CARTESIAN_POINT('Ctrl Pts',(6.59184067821734,8.12672309019558,13.8817013219084));
#60028=CARTESIAN_POINT('Ctrl Pts',(6.61065772423113,8.10331314446322,13.8796902373481));
#60029=CARTESIAN_POINT('Ctrl Pts',(6.63494501282913,8.07309776912488,13.8770945169));
#60030=CARTESIAN_POINT('Ctrl Pts',(6.65848117657335,8.04160268323559,13.8750641472367));
#60031=CARTESIAN_POINT('Ctrl Pts',(6.68115250257791,8.00889137467638,13.8735913556586));
#60032=CARTESIAN_POINT('Ctrl Pts',(6.70127068946919,7.97986386129141,13.8722844230066));
#60033=CARTESIAN_POINT('Ctrl Pts',(6.72070781417969,7.9498786944054,13.8714165516457));
#60034=CARTESIAN_POINT('Ctrl Pts',(6.73937916399641,7.91898200451403,13.8709840640806));
#60035=CARTESIAN_POINT('Ctrl Pts',(6.74871483890477,7.90353365956835,13.870767820298));
#60036=CARTESIAN_POINT('Ctrl Pts',(6.75785902080652,7.8878574044475,13.8706604547887));
#60037=CARTESIAN_POINT('Ctrl Pts',(6.76680054007733,7.87195919711844,13.8706617016596));
#60038=CARTESIAN_POINT('Ctrl Pts',(6.77127129971274,7.8640100934539,13.870662325095));
#60039=CARTESIAN_POINT('Ctrl Pts',(6.7756913901382,7.85600549948828,13.8706901040865));
#60040=CARTESIAN_POINT('Ctrl Pts',(6.78005938330691,7.84794615914813,13.870745019926));
#60041=CARTESIAN_POINT('Ctrl Pts',(6.78279756125055,7.84289397451614,13.8707794451952));
#60042=CARTESIAN_POINT('Ctrl Pts',(6.78584184729762,7.83720799132701,13.8708299285122));
#60043=CARTESIAN_POINT('Ctrl Pts',(6.78857536488141,7.83203835562467,13.8708875817803));
#60044=CARTESIAN_POINT('Ctrl Pts',(6.7902024061723,7.82896129082126,13.8709218980943));
#60045=CARTESIAN_POINT('Ctrl Pts',(6.7917202829825,7.82606777959187,13.8709582453095));
#60046=CARTESIAN_POINT('Ctrl Pts',(6.79300562079399,7.8236046403435,13.8709911695315));
#60047=CARTESIAN_POINT('Ctrl Pts',(6.79345272558942,7.82274783728371,13.8710026222231));
#60048=CARTESIAN_POINT('Ctrl Pts',(6.79389954821732,7.82188983815143,13.8710143691982));
#60049=CARTESIAN_POINT('Ctrl Pts',(6.79434608427298,7.82103064210005,13.8710264118769));
#60050=CARTESIAN_POINT('Ctrl Pts',(6.81252333387961,7.78605514372952,13.8715166360683));
#60051=CARTESIAN_POINT('Ctrl Pts',(6.83022894062228,7.74909367512641,13.8724970484977));
#60052=CARTESIAN_POINT('Ctrl Pts',(6.84717623523151,7.71012612079511,13.8740440457161));
#60053=CARTESIAN_POINT('Ctrl Pts',(6.86323327632808,7.67320555997651,13.8755097780637));
#60054=CARTESIAN_POINT('Ctrl Pts',(6.87860976086485,7.63448416891028,13.877484028969));
#60055=CARTESIAN_POINT('Ctrl Pts',(6.89302553076019,7.59397247530125,13.8800306971348));
#60056=CARTESIAN_POINT('Ctrl Pts',(6.90424943002053,7.56243068660491,13.8820134942487));
#60057=CARTESIAN_POINT('Ctrl Pts',(6.91489035793338,7.52980412810098,13.8843432466388));
#60058=CARTESIAN_POINT('Ctrl Pts',(6.92479798906295,7.49611033022436,13.8870502692081));
#60059=CARTESIAN_POINT('Ctrl Pts',(6.92907683310261,7.48155886940268,13.8882193607129));
#60060=CARTESIAN_POINT('Ctrl Pts',(6.93321866944701,7.46680848796475,13.8894588320564));
#60061=CARTESIAN_POINT('Ctrl Pts',(6.93721230138223,7.4518625562698,13.8907701671218));
#60062=CARTESIAN_POINT('Ctrl Pts',(6.9484442045095,7.40982782205596,13.8944582356921));
#60063=CARTESIAN_POINT('Ctrl Pts',(6.95850648009574,7.36624350871026,13.8987151208828));
#60064=CARTESIAN_POINT('Ctrl Pts',(6.96712753753733,7.32120898892648,13.9035711092745));
#60065=CARTESIAN_POINT('Ctrl Pts',(6.97532946869924,7.27836389321998,13.9081910161458));
#60066=CARTESIAN_POINT('Ctrl Pts',(6.9822272334274,7.2342062429364,13.9133530784423));
#60067=CARTESIAN_POINT('Ctrl Pts',(6.98755254580326,7.18885404781863,13.9190811460232));
#60068=CARTESIAN_POINT('Ctrl Pts',(6.98923555651714,7.1745209486699,13.9208914434157));
#60069=CARTESIAN_POINT('Ctrl Pts',(6.99076122017395,7.1600687861646,13.9227582632191));
#60070=CARTESIAN_POINT('Ctrl Pts',(6.99212021289044,7.14550199364052,13.9246823352425));
#60071=CARTESIAN_POINT('Ctrl Pts',(6.99623922944679,7.10135101413096,13.9305140696029));
#60072=CARTESIAN_POINT('Ctrl Pts',(6.99882923224073,7.05614391289398,13.9368721862835));
#60073=CARTESIAN_POINT('Ctrl Pts',(6.99967290755981,7.0100657634129,13.9437477057266));
#60074=CARTESIAN_POINT('Ctrl Pts',(6.99987322812676,6.9991250604913,13.9453802152024));
#60075=CARTESIAN_POINT('Ctrl Pts',(6.99997495712425,6.98813543089333,13.9470418721719));
#60076=CARTESIAN_POINT('Ctrl Pts',(6.99997490630447,6.97709969502297,13.9487325180188));
#60077=CARTESIAN_POINT('Ctrl Pts',(6.99990207204853,6.87914589968496,13.8881633252755));
#60078=CARTESIAN_POINT('Ctrl Pts',(6.99990207204853,7.13651903111862,14.0922344622602));
#60079=CARTESIAN_POINT('Ctrl Pts',(6.99990207204853,7.80837747144884,14.6760282815914));
#60080=CARTESIAN_POINT('Ctrl Pts',(6.99990207204853,8.78348339483348,15.7555617435629));
#60081=CARTESIAN_POINT('Ctrl Pts',(6.99990207204853,9.70999136997589,17.1681316968964));
#60082=CARTESIAN_POINT('Ctrl Pts',(6.99990207204853,10.4111900158817,18.7078358093743));
#60083=CARTESIAN_POINT('Ctrl Pts',(6.99990207204853,10.8675506644196,20.3372588457581));
#60084=CARTESIAN_POINT('Ctrl Pts',(6.99990207204853,11.0696787430501,22.0150965875122));
#60085=CARTESIAN_POINT('Ctrl Pts',(6.99990207204853,11.0250235947296,23.3220448130867));
#60086=CARTESIAN_POINT('Ctrl Pts',(6.99990207204853,10.9251663319762,24.0577252196839));
#60087=CARTESIAN_POINT('Ctrl Pts',(6.99990207204853,10.8963460242105,24.2367460192875));
#60088=CARTESIAN_POINT('Ctrl Pts',(7.00660351962175,7.17662270770088,13.5129633937184));
#60089=CARTESIAN_POINT('Ctrl Pts',(7.00660351962175,7.44526632069181,13.7259689543078));
#60090=CARTESIAN_POINT('Ctrl Pts',(7.00660351962175,8.14635256616599,14.3351781181045));
#60091=CARTESIAN_POINT('Ctrl Pts',(7.00660351962175,9.16384720170705,15.4616262299551));
#60092=CARTESIAN_POINT('Ctrl Pts',(7.00660351962175,10.1310075548848,16.9361119525886));
#60093=CARTESIAN_POINT('Ctrl Pts',(7.00660351962175,10.8627090938492,18.5429270809962));
#60094=CARTESIAN_POINT('Ctrl Pts',(7.00660351962175,11.3389908857068,20.2432827124676));
#60095=CARTESIAN_POINT('Ctrl Pts',(7.00660351962175,11.5499472237732,21.9946879765234));
#60096=CARTESIAN_POINT('Ctrl Pts',(7.00660351962175,11.5033434054452,23.3583635329505));
#60097=CARTESIAN_POINT('Ctrl Pts',(7.00660351962175,11.39915283926,24.1260290318526));
#60098=CARTESIAN_POINT('Ctrl Pts',(7.00660351962175,11.3690777000579,24.3128491557423));
#60099=CARTESIAN_POINT('Ctrl Pts',(6.71669448330701,7.4134869680442,13.214212526843));
#60100=CARTESIAN_POINT('Ctrl Pts',(6.71669448330701,7.69110463953127,13.4343320727304));
#60101=CARTESIAN_POINT('Ctrl Pts',(6.71669448330701,8.4154633629351,14.0637780637606));
#60102=CARTESIAN_POINT('Ctrl Pts',(6.71669448330701,9.46670977568878,15.2275817056569));
#60103=CARTESIAN_POINT('Ctrl Pts',(6.71669448330701,10.4662393596655,16.7513675165855));
#60104=CARTESIAN_POINT('Ctrl Pts',(6.71669448330701,11.2222286582395,18.4116194196232));
#60105=CARTESIAN_POINT('Ctrl Pts',(6.71669448330701,11.714372550101,20.1684547369726));
#60106=CARTESIAN_POINT('Ctrl Pts',(6.71669448330701,11.932358340829,21.9784377330904));
#60107=CARTESIAN_POINT('Ctrl Pts',(6.71669448330701,11.8842029048076,23.3872821124319));
#60108=CARTESIAN_POINT('Ctrl Pts',(6.71669448330701,11.7765619697793,24.1804155638817));
#60109=CARTESIAN_POINT('Ctrl Pts',(6.71669448330701,11.7454876779928,24.3734458565265));
#60110=CARTESIAN_POINT('Ctrl Pts',(6.25325583820154,7.48886254419364,13.1191432298515));
#60111=CARTESIAN_POINT('Ctrl Pts',(6.25325583820154,7.76933596448606,13.3415266070968));
#60112=CARTESIAN_POINT('Ctrl Pts',(6.25325583820154,8.50110051783243,13.977412415217));
#60113=CARTESIAN_POINT('Ctrl Pts',(6.25325583820154,9.56308751107701,15.1531034334399));
#60114=CARTESIAN_POINT('Ctrl Pts',(6.25325583820154,10.5729177179411,16.6925776498335));
#60115=CARTESIAN_POINT('Ctrl Pts',(6.25325583820154,11.3366359320959,18.3698343457033));
#60116=CARTESIAN_POINT('Ctrl Pts',(6.25325583820154,11.8338275036932,20.1446427791995));
#60117=CARTESIAN_POINT('Ctrl Pts',(6.25325583820154,12.0540502255857,21.9732665373202));
#60118=CARTESIAN_POINT('Ctrl Pts',(6.25325583820154,12.0054010296428,23.3964846598617));
#60119=CARTESIAN_POINT('Ctrl Pts',(6.25325583820154,11.8966621090471,24.197722591042));
#60120=CARTESIAN_POINT('Ctrl Pts',(6.25325583820154,11.8652698642546,24.3927291001344));
#60121=CARTESIAN_POINT('Ctrl Pts',(6.99999999999964,6.9770996949353,13.9487325181688));
#60122=CARTESIAN_POINT('Ctrl Pts',(6.99999999999964,7.10630919510342,14.0533969802629));
#60123=CARTESIAN_POINT('Ctrl Pts',(6.9999999999822,7.23276302591308,14.1606658502628));
#60124=CARTESIAN_POINT('Ctrl Pts',(6.99999999939354,7.35656040710902,14.2705574401669));
#60125=CARTESIAN_POINT('Ctrl Pts',(6.99999999894868,7.45011564810677,14.3536038994521));
#60126=CARTESIAN_POINT('Ctrl Pts',(6.99999999821258,7.54215320932168,14.4381491461423));
#60127=CARTESIAN_POINT('Ctrl Pts',(6.99999999796688,7.63270310594372,14.5242160801555));
#60128=CARTESIAN_POINT('Ctrl Pts',(6.99999999764081,7.75286913175653,14.6384329020413));
#60129=CARTESIAN_POINT('Ctrl Pts',(6.99999999919465,7.87041678058885,14.7553285309957));
#60130=CARTESIAN_POINT('Ctrl Pts',(6.99999999987621,7.98540560911135,14.8750121804876));
#60131=CARTESIAN_POINT('Ctrl Pts',(6.99999999995187,7.99817037168945,14.8882981091284));
#60132=CARTESIAN_POINT('Ctrl Pts',(6.99999999999966,8.0109035611319,14.9016184278241));
#60133=CARTESIAN_POINT('Ctrl Pts',(6.99999999999966,8.02360522778826,14.9149733106003));
#60134=CARTESIAN_POINT('Ctrl Pts',(6.99999999999966,8.16383226758317,15.0624118892664));
#60135=CARTESIAN_POINT('Ctrl Pts',(6.99999999555676,8.30026050838411,15.2139928575566));
#60136=CARTESIAN_POINT('Ctrl Pts',(6.9999999949331,8.43247331547347,15.3693638375008));
#60137=CARTESIAN_POINT('Ctrl Pts',(6.9999999944045,8.54453604154188,15.5010552821329));
#60138=CARTESIAN_POINT('Ctrl Pts',(6.99999999611176,8.65357075339724,15.6354687272598));
#60139=CARTESIAN_POINT('Ctrl Pts',(6.99999999794596,8.75934445476941,15.7723688164645));
#60140=CARTESIAN_POINT('Ctrl Pts',(6.99999999900076,8.82017273892882,15.8510972472518));
#60141=CARTESIAN_POINT('Ctrl Pts',(6.99999999999966,8.87992292103336,15.9306477113447));
#60142=CARTESIAN_POINT('Ctrl Pts',(6.99999999999966,8.93856128342716,16.0109662939737));
#60143=CARTESIAN_POINT('Ctrl Pts',(6.99999999999966,9.09304441859853,16.2225661059487));
#60144=CARTESIAN_POINT('Ctrl Pts',(6.99999999747658,9.23974414863281,16.4395584290727));
#60145=CARTESIAN_POINT('Ctrl Pts',(6.99999999839567,9.37848092351118,16.6614642208066));
#60146=CARTESIAN_POINT('Ctrl Pts',(6.99999999910204,9.48510581806906,16.832007911664));
#60147=CARTESIAN_POINT('Ctrl Pts',(6.9999999999434,9.58702683609379,17.0054547377811));
#60148=CARTESIAN_POINT('Ctrl Pts',(6.99999999999483,9.6841487530217,17.1816030217134));
#60149=CARTESIAN_POINT('Ctrl Pts',(6.99999999999816,9.69044305714598,17.1930188885446));
#60150=CARTESIAN_POINT('Ctrl Pts',(6.99999999999966,9.69671719993505,17.204446106161));
#60151=CARTESIAN_POINT('Ctrl Pts',(6.99999999999966,9.70297115744669,17.2158846182766));
#60152=CARTESIAN_POINT('Ctrl Pts',(6.99999999999966,9.87483116551721,17.5302172278029));
#60153=CARTESIAN_POINT('Ctrl Pts',(7.00000000000773,10.0314645880133,17.8530584345459));
#60154=CARTESIAN_POINT('Ctrl Pts',(6.99999999997817,10.1719515132473,18.18283371903));
#60155=CARTESIAN_POINT('Ctrl Pts',(6.99999999996847,10.2181007081393,18.291163115868));
#60156=CARTESIAN_POINT('Ctrl Pts',(6.99999999999966,10.2625076901965,18.4002403628134));
#60157=CARTESIAN_POINT('Ctrl Pts',(6.99999999999966,10.3051403168605,18.5100085133683));
#60158=CARTESIAN_POINT('Ctrl Pts',(6.99999999999966,10.3319503563143,18.5790375335677));
#60159=CARTESIAN_POINT('Ctrl Pts',(6.99999999997182,10.358061234196,18.6483391264715));
#60160=CARTESIAN_POINT('Ctrl Pts',(6.99999999993242,10.3834658664667,18.7178989075883));
#60161=CARTESIAN_POINT('Ctrl Pts',(6.99999999971846,10.5214375580093,19.0956757067867));
#60162=CARTESIAN_POINT('Ctrl Pts',(6.99999999999966,10.6385735736358,19.481068218458));
#60163=CARTESIAN_POINT('Ctrl Pts',(6.99999999999966,10.7343189353094,19.8715618853161));
#60164=CARTESIAN_POINT('Ctrl Pts',(6.99999999999966,10.7726975056961,20.0280873651628));
#60165=CARTESIAN_POINT('Ctrl Pts',(6.99999999962326,10.8076377716897,20.185433198903));
#60166=CARTESIAN_POINT('Ctrl Pts',(6.99999999912715,10.8391033444699,20.3434768176547));
#60167=CARTESIAN_POINT('Ctrl Pts',(6.99999999825489,10.8944266540483,20.6213518179981));
#60168=CARTESIAN_POINT('Ctrl Pts',(6.99999999886813,10.9390114311113,20.901384532212));
#60169=CARTESIAN_POINT('Ctrl Pts',(6.99999999981999,10.9726752761601,21.1829081638845));
#60170=CARTESIAN_POINT('Ctrl Pts',(6.99999999992605,10.9764261391342,21.2142758393488));
#60171=CARTESIAN_POINT('Ctrl Pts',(6.99999999999966,10.9800413701157,21.2456620137402));
#60172=CARTESIAN_POINT('Ctrl Pts',(6.99999999999966,10.9835206775455,21.2770657559186));
#60173=CARTESIAN_POINT('Ctrl Pts',(6.99999999999966,11.0078800144039,21.4969297230345));
#60174=CARTESIAN_POINT('Ctrl Pts',(6.99999999634613,11.0256232012553,21.7176567471409));
#60175=CARTESIAN_POINT('Ctrl Pts',(6.99999999542162,11.0366759629532,21.9386384483813));
#60176=CARTESIAN_POINT('Ctrl Pts',(6.99999999531135,11.0379943367139,21.9649971526099));
#60177=CARTESIAN_POINT('Ctrl Pts',(6.99999999523594,11.0392175818929,21.991359479604));
#60178=CARTESIAN_POINT('Ctrl Pts',(6.99999999520043,11.0403456220732,22.017724397347));
#60179=CARTESIAN_POINT('Ctrl Pts',(6.99999999489237,11.0501296267264,22.2463992995019));
#60180=CARTESIAN_POINT('Ctrl Pts',(6.99999999999966,11.0527466422052,22.4752684797614));
#60181=CARTESIAN_POINT('Ctrl Pts',(6.99999999999966,11.0482982700561,22.7036632710443));
#60182=CARTESIAN_POINT('Ctrl Pts',(6.99999999999966,11.04498338064,22.8738611436468));
#60183=CARTESIAN_POINT('Ctrl Pts',(6.99999999741397,11.0376887143849,23.0437872743491));
#60184=CARTESIAN_POINT('Ctrl Pts',(6.999999997457,11.0264496314453,23.2135421338117));
#60185=CARTESIAN_POINT('Ctrl Pts',(6.99999999749808,11.015721453047,23.3755803024133));
#60186=CARTESIAN_POINT('Ctrl Pts',(6.999999998651,11.0013989616562,23.5374627543917));
#60187=CARTESIAN_POINT('Ctrl Pts',(6.99999999924032,10.9834686167949,23.6992764926476));
#60188=CARTESIAN_POINT('Ctrl Pts',(6.99999999975843,10.9677048395953,23.8415378789977));
#60189=CARTESIAN_POINT('Ctrl Pts',(6.99999999990829,10.9491517993076,23.9837463392033));
#60190=CARTESIAN_POINT('Ctrl Pts',(6.99999999989363,10.927773309634,24.1259362011891));
#60191=CARTESIAN_POINT('Ctrl Pts',(6.26386081937142,8.42073287750616,13.9442638621487));
#60192=CARTESIAN_POINT('Ctrl Pts',(6.26460715755161,8.6058952350089,14.1256648827888));
#60193=CARTESIAN_POINT('Ctrl Pts',(6.26531568582214,8.78358439506317,14.3114857095034));
#60194=CARTESIAN_POINT('Ctrl Pts',(6.26598638726736,8.95374370287065,14.501085754477));
#60195=CARTESIAN_POINT('Ctrl Pts',(6.26666473794233,9.12584364707761,14.6928481539722));
#60196=CARTESIAN_POINT('Ctrl Pts',(6.26730439407986,9.29024105734324,14.8884764945959));
#60197=CARTESIAN_POINT('Ctrl Pts',(6.26790534152617,9.44691000884794,15.0873499596924));
#60198=CARTESIAN_POINT('Ctrl Pts',(6.26800176663185,9.47204834714509,15.1192602290592));
#60199=CARTESIAN_POINT('Ctrl Pts',(6.26809719515578,9.49698777632441,15.1512541330831));
#60200=CARTESIAN_POINT('Ctrl Pts',(6.26819162704677,9.52172826504943,15.1833292053216));
#60201=CARTESIAN_POINT('Ctrl Pts',(6.26876871480417,9.67292118308826,15.3793448872247));
#60202=CARTESIAN_POINT('Ctrl Pts',(6.26930858191222,9.81668277327996,15.5783878909095));
#60203=CARTESIAN_POINT('Ctrl Pts',(6.26981121816768,9.95308962999951,15.7798039214011));
#60204=CARTESIAN_POINT('Ctrl Pts',(6.27017912420821,10.0529330177616,15.9272309592898));
#60205=CARTESIAN_POINT('Ctrl Pts',(6.27052708368989,10.1488365136903,16.0759303990776));
#60206=CARTESIAN_POINT('Ctrl Pts',(6.27085509339984,10.2408369655875,16.2256619541204));
#60207=CARTESIAN_POINT('Ctrl Pts',(6.2712113779156,10.3407679598827,16.3883005375646));
#60208=CARTESIAN_POINT('Ctrl Pts',(6.27154412378864,10.4360939213311,16.5521566168677));
#60209=CARTESIAN_POINT('Ctrl Pts',(6.2718533269388,10.5268693884646,16.7169400098764));
#60210=CARTESIAN_POINT('Ctrl Pts',(6.27227096849388,10.6494800644449,16.9395133972145));
#60211=CARTESIAN_POINT('Ctrl Pts',(6.27264565867609,10.7637884966596,17.1637765277338));
#60212=CARTESIAN_POINT('Ctrl Pts',(6.27297738955254,10.8699989601779,17.3890723859027));
#60213=CARTESIAN_POINT('Ctrl Pts',(6.27330912042898,10.9762094236961,17.6143682440716));
#60214=CARTESIAN_POINT('Ctrl Pts',(6.27359789201885,11.0743220034987,17.8406970067989));
#60215=CARTESIAN_POINT('Ctrl Pts',(6.27384369853182,11.1645577069347,18.067457721897));
#60216=CARTESIAN_POINT('Ctrl Pts',(6.27395596472971,11.2057706887037,18.1710252108335));
#60217=CARTESIAN_POINT('Ctrl Pts',(6.27405926854011,11.2453407879993,18.2746835591084));
#60218=CARTESIAN_POINT('Ctrl Pts',(6.27415361658734,11.2832901518629,18.3783792666538));
#60219=CARTESIAN_POINT('Ctrl Pts',(6.27415652014011,11.2844580401626,18.3815704928362));
#60220=CARTESIAN_POINT('Ctrl Pts',(6.27415941515016,11.2856243934921,18.3847617544467));
#60221=CARTESIAN_POINT('Ctrl Pts',(6.2741623016233,11.28678921251,18.3879530499727));
#60222=CARTESIAN_POINT('Ctrl Pts',(6.27420631168118,11.3045492088017,18.436610734845));
#60223=CARTESIAN_POINT('Ctrl Pts',(6.27424833715608,11.3219525216513,18.4852762942839));
#60224=CARTESIAN_POINT('Ctrl Pts',(6.27428839865745,11.339002369061,18.5339441294818));
#60225=CARTESIAN_POINT('Ctrl Pts',(6.2743178505947,11.3515368727312,18.5697231686864));
#60226=CARTESIAN_POINT('Ctrl Pts',(6.27434670178379,11.3640966427874,18.6061341459457));
#60227=CARTESIAN_POINT('Ctrl Pts',(6.27437398807154,11.3762335233597,18.6418700169536));
#60228=CARTESIAN_POINT('Ctrl Pts',(6.27438625179296,11.3816883995814,18.6579313724119));
#60229=CARTESIAN_POINT('Ctrl Pts',(6.27439819940099,11.3870585284997,18.6738561212743));
#60230=CARTESIAN_POINT('Ctrl Pts',(6.27440974336018,11.3923064605535,18.6895245117215));
#60231=CARTESIAN_POINT('Ctrl Pts',(6.274560647478,11.4609081026565,18.8943437248441));
#60232=CARTESIAN_POINT('Ctrl Pts',(6.27467736549451,11.5248696283609,19.1037519752928));
#60233=CARTESIAN_POINT('Ctrl Pts',(6.27475989567,11.5836612122644,19.3175737252288));
#60234=CARTESIAN_POINT('Ctrl Pts',(6.27484107236027,11.6414886210769,19.5278888235064));
#60235=CARTESIAN_POINT('Ctrl Pts',(6.27488917337323,11.6943142587797,19.7424739301517));
#60236=CARTESIAN_POINT('Ctrl Pts',(6.27490419802558,11.7416106438955,19.9611171627007));
#60237=CARTESIAN_POINT('Ctrl Pts',(6.27490863189467,11.7555681036062,20.025640151125));
#60238=CARTESIAN_POINT('Ctrl Pts',(6.27491018522552,11.7690438774239,20.0905162465538));
#60239=CARTESIAN_POINT('Ctrl Pts',(6.27490885801623,11.7820240141381,20.1557392229126));
#60240=CARTESIAN_POINT('Ctrl Pts',(6.27490450962152,11.8245514121042,20.3694321549065));
#60241=CARTESIAN_POINT('Ctrl Pts',(6.27486924020097,11.8617597650821,20.5868522809959));
#60242=CARTESIAN_POINT('Ctrl Pts',(6.27480305022229,11.8931690681274,20.8077236719151));
#60243=CARTESIAN_POINT('Ctrl Pts',(6.27475277155223,11.9170279364352,20.9755001240474));
#60244=CARTESIAN_POINT('Ctrl Pts',(6.2746846514378,11.9375403381901,21.1452670712505));
#60245=CARTESIAN_POINT('Ctrl Pts',(6.27459869040533,11.9544888397465,21.3168846885222));
#60246=CARTESIAN_POINT('Ctrl Pts',(6.27448994587059,11.9759294490948,21.5339886181507));
#60247=CARTESIAN_POINT('Ctrl Pts',(6.27435264873577,11.9916671385014,21.7540557993486));
#60248=CARTESIAN_POINT('Ctrl Pts',(6.27418680148104,12.0012474181871,21.9767636838325));
#60249=CARTESIAN_POINT('Ctrl Pts',(6.27401315166475,12.0112784181575,22.2099492333138));
#60250=CARTESIAN_POINT('Ctrl Pts',(6.27380820214771,12.0145579386257,22.4460299249337));
#60251=CARTESIAN_POINT('Ctrl Pts',(6.27357195670799,12.0106606480893,22.6846258656287));
#60252=CARTESIAN_POINT('Ctrl Pts',(6.27333930431345,12.0068226312514,22.9195930124892));
#60253=CARTESIAN_POINT('Ctrl Pts',(6.27307630070905,11.9960244157004,23.1569995372925));
#60254=CARTESIAN_POINT('Ctrl Pts',(6.27278295049408,11.9778553213893,23.3964324270879));
#60255=CARTESIAN_POINT('Ctrl Pts',(6.27261681839334,11.9675656755929,23.5320296993485));
#60256=CARTESIAN_POINT('Ctrl Pts',(6.27244095336116,11.9549119178812,23.6682759604467));
#60257=CARTESIAN_POINT('Ctrl Pts',(6.27225535638668,11.9398188605389,23.8050887673585));
#60258=CARTESIAN_POINT('Ctrl Pts',(6.27204648360782,11.9228329757344,23.9590593331134));
#60259=CARTESIAN_POINT('Ctrl Pts',(6.27182528484552,11.9027576373191,24.1137477342554));
#60260=CARTESIAN_POINT('Ctrl Pts',(6.27159176169286,11.8794807213832,24.2690119676737));
#60261=CARTESIAN_POINT('Ctrl Pts',(-6.390310997221,8.13937950336677,13.724966055094));
#60262=CARTESIAN_POINT('Ctrl Pts',(-4.26020733148,9.11426650158535,13.8221738588783));
#60263=CARTESIAN_POINT('Ctrl Pts',(0.0001535202090341,10.090263157491,13.9182984617449));
#60264=CARTESIAN_POINT('Ctrl Pts',(4.260514371898,9.11419615983807,13.8221669310127));
#60265=CARTESIAN_POINT('Ctrl Pts',(6.390771557848,8.13916871046851,13.7249450365314));
#60266=CARTESIAN_POINT('Ctrl Pts',(-6.390310997221,8.71309690457886,14.2543287817288));
#60267=CARTESIAN_POINT('Ctrl Pts',(-4.26020733148,9.62713419180251,14.3567676707055));
#60268=CARTESIAN_POINT('Ctrl Pts',(0.0001535202090341,10.5425537312226,
14.4578350530826));
#60269=CARTESIAN_POINT('Ctrl Pts',(4.260514371898,9.62706821595377,14.3567603866072));
#60270=CARTESIAN_POINT('Ctrl Pts',(6.390771557848,8.71289926878235,14.2543066320824));
#60271=CARTESIAN_POINT('Ctrl Pts',(-6.390310997221,9.96973300996386,15.6641218054972));
#60272=CARTESIAN_POINT('Ctrl Pts',(-4.26020733148,10.7489906364333,15.7526919792829));
#60273=CARTESIAN_POINT('Ctrl Pts',(0.0001535202090341,11.5273040839031,
15.8421753984647));
#60274=CARTESIAN_POINT('Ctrl Pts',(4.260514371898,10.7489345420516,15.7526855300649));
#60275=CARTESIAN_POINT('Ctrl Pts',(6.390771557848,9.96956451660001,15.6641026546034));
#60276=CARTESIAN_POINT('Ctrl Pts',(-6.390310997221,11.387980958516,18.3168609124995));
#60277=CARTESIAN_POINT('Ctrl Pts',(-4.26020733148,12.0191857141961,18.305065900394));
#60278=CARTESIAN_POINT('Ctrl Pts',(0.0001535202090341,12.6510838649606,
18.2929947853334));
#60279=CARTESIAN_POINT('Ctrl Pts',(4.260514371898,12.0191401722118,18.3050667703745));
#60280=CARTESIAN_POINT('Ctrl Pts',(6.390771557848,11.3878444775859,18.3168634628528));
#60281=CARTESIAN_POINT('Ctrl Pts',(-6.390310997221,12.0713618431303,21.4528914163341));
#60282=CARTESIAN_POINT('Ctrl Pts',(-4.26020733148,12.6592425324047,21.2792389757137));
#60283=CARTESIAN_POINT('Ctrl Pts',(0.0001535202090341,13.2456889758127,
21.1056340488841));
#60284=CARTESIAN_POINT('Ctrl Pts',(4.260514371898,12.6592002662047,21.2792514877189));
#60285=CARTESIAN_POINT('Ctrl Pts',(6.390771557848,12.07123472984,21.4529289639673));
#60286=CARTESIAN_POINT('Ctrl Pts',(-6.390310997221,11.9720502124569,23.5458951845851));
#60287=CARTESIAN_POINT('Ctrl Pts',(-4.26020733148,12.6077625569466,23.2652553028773));
#60288=CARTESIAN_POINT('Ctrl Pts',(0.0001535202090341,13.2461450660892,
22.9846380445134));
#60289=CARTESIAN_POINT('Ctrl Pts',(4.260514371898,12.6077165476319,23.2652755274378));
#60290=CARTESIAN_POINT('Ctrl Pts',(6.390771557848,11.9719127569025,23.5459558653499));
#60291=CARTESIAN_POINT('Ctrl Pts',(-6.390310997221,11.8061936875927,24.5118462831628));
#60292=CARTESIAN_POINT('Ctrl Pts',(-4.26020733148,12.4817978962268,24.1870546128076));
#60293=CARTESIAN_POINT('Ctrl Pts',(0.0001535202090341,13.1582606881552,
23.8622603664262));
#60294=CARTESIAN_POINT('Ctrl Pts',(4.260514371898,12.4817491423946,24.1870780212883));
#60295=CARTESIAN_POINT('Ctrl Pts',(6.390771557848,11.8060476064905,24.5119165105573));
#60296=CARTESIAN_POINT('',(-6.26385899039824,8.42070725657994,13.944262563225));
#60297=CARTESIAN_POINT('Ctrl Pts',(-6.26386059994869,8.4207113711049,13.9442583573388));
#60298=CARTESIAN_POINT('Ctrl Pts',(-6.26455152048013,8.59292042455144,14.1129910531294));
#60299=CARTESIAN_POINT('Ctrl Pts',(-6.26520985692811,8.75834812375439,14.2852422441848));
#60300=CARTESIAN_POINT('Ctrl Pts',(-6.26583560983094,8.91699593500101,14.4604068244786));
#60301=CARTESIAN_POINT('Ctrl Pts',(-6.26647066381859,9.07800186035863,14.6381750213322));
#60302=CARTESIAN_POINT('Ctrl Pts',(-6.26707215842975,9.23202489931598,14.8189438733917));
#60303=CARTESIAN_POINT('Ctrl Pts',(-6.26764009422708,9.37909856275395,15.0021245936472));
#60304=CARTESIAN_POINT('Ctrl Pts',(-6.26812468345807,9.50458865124676,15.1584229019757));
#60305=CARTESIAN_POINT('Ctrl Pts',(-6.26858484087964,9.62501996429814,15.3164778898243));
#60306=CARTESIAN_POINT('Ctrl Pts',(-6.2690205668413,9.7404307958954,15.4759481442773));
#60307=CARTESIAN_POINT('Ctrl Pts',(-6.26953467307883,9.87660222845387,15.6641045997745));
#60308=CARTESIAN_POINT('Ctrl Pts',(-6.27001476762018,10.005784944435,15.8542296366687));
#60309=CARTESIAN_POINT('Ctrl Pts',(-6.27046085103946,10.1281582269328,16.0457333774502));
#60310=CARTESIAN_POINT('Ctrl Pts',(-6.27062083324975,10.1720458662577,16.1144137865495));
#60311=CARTESIAN_POINT('Ctrl Pts',(-6.27077644092214,10.215057822839,16.1832719922629));
#60312=CARTESIAN_POINT('Ctrl Pts',(-6.27092767408311,10.2572028653329,16.2522823290061));
#60313=CARTESIAN_POINT('Ctrl Pts',(-6.27136815432473,10.3799541083887,16.4532811681964));
#60314=CARTESIAN_POINT('Ctrl Pts',(-6.27177152391562,10.4953498718875,16.6555664402298));
#60315=CARTESIAN_POINT('Ctrl Pts',(-6.27213778285578,10.6036187611275,16.8585419856448));
#60316=CARTESIAN_POINT('Ctrl Pts',(-6.27250404179594,10.7118876503675,17.0615175310597));
#60317=CARTESIAN_POINT('Ctrl Pts',(-6.27283319008536,10.8130297690453,17.2651835383498));
#60318=CARTESIAN_POINT('Ctrl Pts',(-6.27312522772406,10.9072902654271,17.4689981447037));
#60319=CARTESIAN_POINT('Ctrl Pts',(-6.27334042077645,10.9767477642208,17.6191825095052));
#60320=CARTESIAN_POINT('Ctrl Pts',(-6.27353526317237,11.0423479808087,17.769176079745));
#60321=CARTESIAN_POINT('Ctrl Pts',(-6.27370997657693,11.1043415438198,17.919075764095));
#60322=CARTESIAN_POINT('Ctrl Pts',(-6.27388468998149,11.1663351068308,18.068975448445));
#60323=CARTESIAN_POINT('Ctrl Pts',(-6.2740392743947,11.2247220604115,18.2187816725573));
#60324=CARTESIAN_POINT('Ctrl Pts',(-6.27417395148167,11.2797074208758,18.3686262123368));
#60325=CARTESIAN_POINT('Ctrl Pts',(-6.27427013678984,11.3189775295513,18.4756439951042));
#60326=CARTESIAN_POINT('Ctrl Pts',(-6.27435616796176,11.3565116921192,18.5826820367218));
#60327=CARTESIAN_POINT('Ctrl Pts',(-6.27443212574741,11.3923815531531,18.6897932929545));
#60328=CARTESIAN_POINT('Ctrl Pts',(-6.27457884479819,11.4616673007278,18.8966879741109));
#60329=CARTESIAN_POINT('Ctrl Pts',(-6.27469165460118,11.5261460216362,19.1080571548633));
#60330=CARTESIAN_POINT('Ctrl Pts',(-6.27477055515638,11.5853122037843,19.3236966635228));
#60331=CARTESIAN_POINT('Ctrl Pts',(-6.27484862828138,11.643857910118,19.5370747604283));
#60332=CARTESIAN_POINT('Ctrl Pts',(-6.27489349964197,11.6972019214643,19.754634199829));
#60333=CARTESIAN_POINT('Ctrl Pts',(-6.27490516923817,11.7448338369295,19.9761313157618));
#60334=CARTESIAN_POINT('Ctrl Pts',(-6.27491664524404,11.7916755726868,20.1939539515765));
#60335=CARTESIAN_POINT('Ctrl Pts',(-6.2748960119357,11.8329931410015,20.4155847540337));
#60336=CARTESIAN_POINT('Ctrl Pts',(-6.27484326931315,11.8682812208486,20.6407462755647));
#60337=CARTESIAN_POINT('Ctrl Pts',(-6.27479056675521,11.9035424949843,20.8657367587512));
#60338=CARTESIAN_POINT('Ctrl Pts',(-6.27470580364662,11.9327834716963,21.0942527726353));
#60339=CARTESIAN_POINT('Ctrl Pts',(-6.27458897998737,11.9554797474119,21.3259696114708));
#60340=CARTESIAN_POINT('Ctrl Pts',(-6.2745478138118,11.9634774327867,21.4076217026017));
#60341=CARTESIAN_POINT('Ctrl Pts',(-6.27450266669875,11.9706622713164,21.4896707935314));
#60342=CARTESIAN_POINT('Ctrl Pts',(-6.27445353863612,11.9770107062091,21.5721011963808));
#60343=CARTESIAN_POINT('Ctrl Pts',(-6.27431624106106,11.9947525968845,21.8024684003303));
#60344=CARTESIAN_POINT('Ctrl Pts',(-6.27414785116559,12.0059621132111,22.0358174529015));
#60345=CARTESIAN_POINT('Ctrl Pts',(-6.27394836868557,12.0102364706698,22.2717644772196));
#60346=CARTESIAN_POINT('Ctrl Pts',(-6.27375072726245,12.0144713793746,22.5055339073128));
#60347=CARTESIAN_POINT('Ctrl Pts',(-6.27352256452363,12.0118985251308,22.7418536687606));
#60348=CARTESIAN_POINT('Ctrl Pts',(-6.27326388021221,12.0021219229472,22.9802999805628));
#60349=CARTESIAN_POINT('Ctrl Pts',(-6.27300884387037,11.9924831905364,23.2153837193321));
#60350=CARTESIAN_POINT('Ctrl Pts',(-6.27272414071743,11.975842425797,23.4525344972157));
#60351=CARTESIAN_POINT('Ctrl Pts',(-6.27240977050724,11.9518163952354,23.6912960224347));
#60352=CARTESIAN_POINT('Ctrl Pts',(-6.27215746727189,11.9325338899391,23.8829182033343));
#60353=CARTESIAN_POINT('Ctrl Pts',(-6.27188605506393,11.9084943551137,24.0755769702775));
#60354=CARTESIAN_POINT('Ctrl Pts',(-6.27159553375607,11.879498052505,24.2690121689631));
#60355=CARTESIAN_POINT('Ctrl Pts',(-6.26386059994846,8.42071137104667,13.9442583572817));
#60356=CARTESIAN_POINT('Ctrl Pts',(-5.93717696836598,8.56158840445482,13.9570575565163));
#60357=CARTESIAN_POINT('Ctrl Pts',(-5.60632732377181,8.69216934607849,13.9678446821751));
#60358=CARTESIAN_POINT('Ctrl Pts',(-5.27194469098664,8.81191899897469,13.9769587750825));
#60359=CARTESIAN_POINT('Ctrl Pts',(-4.97209615130009,8.91930124622187,13.9851315902377));
#60360=CARTESIAN_POINT('Ctrl Pts',(-4.66940669402091,9.01797284387651,13.991959419582));
#60361=CARTESIAN_POINT('Ctrl Pts',(-4.36433277146454,9.10758639984849,13.9977003959948));
#60362=CARTESIAN_POINT('Ctrl Pts',(-4.0887152634072,9.18854731836354,14.0028870523943));
#60363=CARTESIAN_POINT('Ctrl Pts',(-3.81115152413417,9.26211453872501,14.0071867723874));
#60364=CARTESIAN_POINT('Ctrl Pts',(-3.53197814314358,9.32807438052413,14.0107986489402));
#60365=CARTESIAN_POINT('Ctrl Pts',(-3.4190946039569,9.35474519118688,14.0122591084114));
#60366=CARTESIAN_POINT('Ctrl Pts',(-3.30594789109754,9.3801727576117,14.013607200518));
#60367=CARTESIAN_POINT('Ctrl Pts',(-3.19256025663433,9.40434542805185,14.0148564684661));
#60368=CARTESIAN_POINT('Ctrl Pts',(-2.94892827982676,9.45628438516944,14.0175407260678));
#60369=CARTESIAN_POINT('Ctrl Pts',(-2.70418858676455,9.50244713954166,14.019792523974));
#60370=CARTESIAN_POINT('Ctrl Pts',(-2.45859671448438,9.54266471038575,14.0216629006831));
#60371=CARTESIAN_POINT('Ctrl Pts',(-2.21908138008969,9.58188720109698,14.0234869997413));
#60372=CARTESIAN_POINT('Ctrl Pts',(-1.97875551474025,9.61545500774489,14.0249483422051));
#60373=CARTESIAN_POINT('Ctrl Pts',(-1.73785615309579,9.64326071165928,14.0260991718243));
#60374=CARTESIAN_POINT('Ctrl Pts',(-1.49989746871486,9.67072698918109,14.0272359531768));
#60375=CARTESIAN_POINT('Ctrl Pts',(-1.2613792040085,9.69257085714106,14.0280697696858));
#60376=CARTESIAN_POINT('Ctrl Pts',(-1.0225298186672,9.7087390174652,14.0286555606451));
#60377=CARTESIAN_POINT('Ctrl Pts',(-0.787286942176469,9.72466304647947,
14.0292325064476));
#60378=CARTESIAN_POINT('Ctrl Pts',(-0.551722869076018,9.73508141111193,
14.0295688746588));
#60379=CARTESIAN_POINT('Ctrl Pts',(-0.316055865644371,9.73999356983431,
14.0297214195832));
#60380=CARTESIAN_POINT('Ctrl Pts',(-0.21080646463155,9.74218735070173,14.0297895464813));
#60381=CARTESIAN_POINT('Ctrl Pts',(-0.105536533801802,9.74328358190328,
14.0298210651924));
#60382=CARTESIAN_POINT('Ctrl Pts',(-0.000265515525107667,9.74328558134228,
14.0298213016319));
#60383=CARTESIAN_POINT('Ctrl Pts',(-0.000177010350108755,9.74328558302328,
14.0298213018307));
#60384=CARTESIAN_POINT('Ctrl Pts',(-8.8505175545061E-5,9.74328558393097,
14.0298213020073));
#60385=CARTESIAN_POINT('Ctrl Pts',(-1.42996123777008E-12,9.74328558406533,
14.0298213021619));
#60386=CARTESIAN_POINT('Ctrl Pts',(0.235250051412205,9.74328594120638,14.0298217130422));
#60387=CARTESIAN_POINT('Ctrl Pts',(0.470496939858318,9.73781829803784,14.0296656159884));
#60388=CARTESIAN_POINT('Ctrl Pts',(0.705523626716445,9.72685975003266,14.029294704648));
#60389=CARTESIAN_POINT('Ctrl Pts',(0.944752984767102,9.7157052448167,14.028917160791));
#60390=CARTESIAN_POINT('Ctrl Pts',(1.18375419567222,9.69886173425948,14.0283170354621));
#60391=CARTESIAN_POINT('Ctrl Pts',(1.42229836833,9.67635915367304,14.0274372869502));
#60392=CARTESIAN_POINT('Ctrl Pts',(1.66374043057524,9.6535832065514,14.0265468510506));
#60393=CARTESIAN_POINT('Ctrl Pts',(1.90471428271175,9.6250099765416,14.0253699432079));
#60394=CARTESIAN_POINT('Ctrl Pts',(2.14498259002289,9.5907242399444,14.0238521563959));
#60395=CARTESIAN_POINT('Ctrl Pts',(2.39034044630107,9.55571223637827,14.0223022186507));
#60396=CARTESIAN_POINT('Ctrl Pts',(2.63496255037747,9.51474323025704,14.0203967857286));
#60397=CARTESIAN_POINT('Ctrl Pts',(2.87859616357419,9.46796179871245,14.0180831143291));
#60398=CARTESIAN_POINT('Ctrl Pts',(2.9833098709974,9.44785514318441,14.017088698547));
#60399=CARTESIAN_POINT('Ctrl Pts',(3.08784097650595,9.4266754343928,14.0160189359209));
#60400=CARTESIAN_POINT('Ctrl Pts',(3.1921694136428,9.40443706680239,14.0148699389744));
#60401=CARTESIAN_POINT('Ctrl Pts',(3.47744261700037,9.34362900205935,14.0117281489836));
#60402=CARTESIAN_POINT('Ctrl Pts',(3.7611942824795,9.27487280401547,14.0079602275019));
#60403=CARTESIAN_POINT('Ctrl Pts',(4.04306981736332,9.19837143643058,14.0033530332897));
#60404=CARTESIAN_POINT('Ctrl Pts',(4.3441061229289,9.11666981206661,13.9984326604549));
#60405=CARTESIAN_POINT('Ctrl Pts',(4.64300256509685,9.02613498942633,13.9925549084651));
#60406=CARTESIAN_POINT('Ctrl Pts',(4.93932721295378,8.92707680407218,13.9854712892336));
#60407=CARTESIAN_POINT('Ctrl Pts',(5.28135521912764,8.81274047101008,13.9772951345338));
#60408=CARTESIAN_POINT('Ctrl Pts',(5.6199569361215,8.6870497021254,13.9675119701404));
#60409=CARTESIAN_POINT('Ctrl Pts',(5.95446816838324,8.55054995909253,13.9557592260817));
#60410=CARTESIAN_POINT('Ctrl Pts',(6.05799647460643,8.50830448021714,13.9521218543928));
#60411=CARTESIAN_POINT('Ctrl Pts',(6.16113297437773,8.4650240396021,13.9482959819136));
#60412=CARTESIAN_POINT('Ctrl Pts',(6.26385797790307,8.4207256142375,13.944271287676));
#60413=CARTESIAN_POINT('Ctrl Pts',(-6.38404538826909,8.37116243072582,13.9421882754888));
#60414=CARTESIAN_POINT('Ctrl Pts',(-5.83050262796989,8.62265888536472,13.9723470810333));
#60415=CARTESIAN_POINT('Ctrl Pts',(-4.53016629286474,9.12937227622254,14.0254998662653));
#60416=CARTESIAN_POINT('Ctrl Pts',(-2.39024486123905,9.65381240370912,14.0662444267208));
#60417=CARTESIAN_POINT('Ctrl Pts',(0.000832361431650141,9.85055455252627,
14.0780418370757));
#60418=CARTESIAN_POINT('Ctrl Pts',(2.39185021568528,9.65354673660712,14.0662272090006));
#60419=CARTESIAN_POINT('Ctrl Pts',(4.53118408442122,9.12901549215188,14.0254666479336));
#60420=CARTESIAN_POINT('Ctrl Pts',(5.83097915587935,8.62244285400822,13.972321193994));
#60421=CARTESIAN_POINT('Ctrl Pts',(6.38405559839713,8.37115779336739,13.9421877126995));
#60422=CARTESIAN_POINT('Ctrl Pts',(-6.17704425963179,7.96381194474042,13.469457267312));
#60423=CARTESIAN_POINT('Ctrl Pts',(-5.64115395945954,8.20569173180422,13.5001727964708));
#60424=CARTESIAN_POINT('Ctrl Pts',(-4.38244641924109,8.6930773017877,13.5546902039183));
#60425=CARTESIAN_POINT('Ctrl Pts',(-2.31188356464167,9.19745367496022,13.5973133398307));
#60426=CARTESIAN_POINT('Ctrl Pts',(0.000805005365969324,9.38662212148953,
13.6099340037559));
#60427=CARTESIAN_POINT('Ctrl Pts',(2.31343653166433,9.19719821279148,13.597295055307));
#60428=CARTESIAN_POINT('Ctrl Pts',(4.38343153533807,8.69273412120314,13.554655889156));
#60429=CARTESIAN_POINT('Ctrl Pts',(5.64161529098573,8.20548395793609,13.5001464313595));
#60430=CARTESIAN_POINT('Ctrl Pts',(6.17705414513472,7.96380748312364,13.4694566948018));
#60431=CARTESIAN_POINT('Ctrl Pts',(-6.17529619645408,8.03269332841907,12.8173794683781));
#60432=CARTESIAN_POINT('Ctrl Pts',(-5.64080537297811,8.27163446441592,12.8477800372787));
#60433=CARTESIAN_POINT('Ctrl Pts',(-4.38470620031409,8.75357501952359,12.9017719820197));
#60434=CARTESIAN_POINT('Ctrl Pts',(-2.31484672892392,9.25351908787722,12.9440117423692));
#60435=CARTESIAN_POINT('Ctrl Pts',(0.000806324308182919,9.4413973955616,
12.9565148963448));
#60436=CARTESIAN_POINT('Ctrl Pts',(2.31640066515831,9.25326551722142,12.9439936229367));
#60437=CARTESIAN_POINT('Ctrl Pts',(4.38568966269628,8.75323537235754,12.901737984911));
#60438=CARTESIAN_POINT('Ctrl Pts',(5.64126549941951,8.27142921664869,12.8477539377952));
#60439=CARTESIAN_POINT('Ctrl Pts',(6.17530605203147,8.03268892390896,12.8173789001941));
#60440=CARTESIAN_POINT('Ctrl Pts',(-6.3774727247386,8.52454337342127,12.4367962200776));
#60441=CARTESIAN_POINT('Ctrl Pts',(-5.82736598295725,8.7691633154091,12.4662375870123));
#60442=CARTESIAN_POINT('Ctrl Pts',(-4.53354138556052,9.26311663296809,12.5181988107581));
#60443=CARTESIAN_POINT('Ctrl Pts',(-2.39609281858094,9.77711650863112,12.558084900948));
#60444=CARTESIAN_POINT('Ctrl Pts',(0.000835057210998115,9.97079836899108,
12.5696222296354));
#60445=CARTESIAN_POINT('Ctrl Pts',(2.39769975586005,9.7768553172162,12.5580680497235));
#60446=CARTESIAN_POINT('Ctrl Pts',(4.5345549711749,9.26276814234134,12.5181663094043));
#60447=CARTESIAN_POINT('Ctrl Pts',(5.82783955217292,8.76895319507773,12.4662123049363));
#60448=CARTESIAN_POINT('Ctrl Pts',(6.37748286204222,8.52453886954492,12.4367956671127));
#60449=CARTESIAN_POINT('',(-6.249945884441,8.55169184623365,12.462653724233));
#60450=CARTESIAN_POINT('Ctrl Pts',(-6.24994577295826,8.55169162808957,12.4626534063286));
#60451=CARTESIAN_POINT('Ctrl Pts',(-5.97414683512782,8.67183837135021,12.476926751268));
#60452=CARTESIAN_POINT('Ctrl Pts',(-5.69345325622611,8.7852362693789,12.4896158765507));
#60453=CARTESIAN_POINT('Ctrl Pts',(-5.40803913489735,8.8912995328883,12.5009061876321));
#60454=CARTESIAN_POINT('Ctrl Pts',(-5.2203826970391,8.96103488489237,12.508329434772));
#60455=CARTESIAN_POINT('Ctrl Pts',(-5.03068593865463,9.0275986149699,12.5151481565809));
#60456=CARTESIAN_POINT('Ctrl Pts',(-4.83900279328378,9.09081292957561,12.5214173229241));
#60457=CARTESIAN_POINT('Ctrl Pts',(-4.78610405895494,9.10825816310221,12.5231474226896));
#60458=CARTESIAN_POINT('Ctrl Pts',(-4.73305460290303,9.12544877501386,12.5248351566563));
#60459=CARTESIAN_POINT('Ctrl Pts',(-4.67985525062854,9.14238145556753,12.5264814015791));
#60460=CARTESIAN_POINT('Ctrl Pts',(-4.4900707310435,9.20278746629457,12.5323542513119));
#60461=CARTESIAN_POINT('Ctrl Pts',(-4.29837839943429,9.25991178170323,12.537698995585));
#60462=CARTESIAN_POINT('Ctrl Pts',(-4.10484844319214,9.31360787682988,12.5425507056659));
#60463=CARTESIAN_POINT('Ctrl Pts',(-3.98095883883625,9.34798182135955,12.5456565630435));
#60464=CARTESIAN_POINT('Ctrl Pts',(-3.85631586549759,9.38095127312882,12.5485600232877));
#60465=CARTESIAN_POINT('Ctrl Pts',(-3.7309389117039,9.41247972892901,12.5512670848039));
#60466=CARTESIAN_POINT('Ctrl Pts',(-3.66825043480706,9.42824395682911,12.552620615562));
#60467=CARTESIAN_POINT('Ctrl Pts',(-3.60537845978922,9.44364792669368,12.5539250344385));
#60468=CARTESIAN_POINT('Ctrl Pts',(-3.54232557106459,9.45868722349521,12.555180829398));
#60469=CARTESIAN_POINT('Ctrl Pts',(-3.51079912670227,9.46620687189598,12.5558087268778));
#60470=CARTESIAN_POINT('Ctrl Pts',(-3.47922745375773,9.47363535146565,12.5564244676311));
#60471=CARTESIAN_POINT('Ctrl Pts',(-3.44761087944285,9.48097211313099,12.5570281024581));
#60472=CARTESIAN_POINT('Ctrl Pts',(-3.43180259228541,9.48464049396366,12.5573299198716));
#60473=CARTESIAN_POINT('Ctrl Pts',(-3.41598307977717,9.48828594528422,12.5576287107566));
#60474=CARTESIAN_POINT('Ctrl Pts',(-3.40015238340376,9.49190839899051,12.5579244804943));
#60475=CARTESIAN_POINT('Ctrl Pts',(-3.38432168703035,9.49553085269679,12.558220250232));
#60476=CARTESIAN_POINT('Ctrl Pts',(-3.36983043489144,9.49882561136923,12.5584883145983));
#60477=CARTESIAN_POINT('Ctrl Pts',(-3.35262678433449,9.5027066992511,12.5588027312502));
#60478=CARTESIAN_POINT('Ctrl Pts',(-3.03782920764183,9.57372401363455,12.5645560217955));
#60479=CARTESIAN_POINT('Ctrl Pts',(-2.72122916966243,9.63497186079253,12.5691453737108));
#60480=CARTESIAN_POINT('Ctrl Pts',(-2.40317289992791,9.68615982574975,12.5728383075911));
#60481=CARTESIAN_POINT('Ctrl Pts',(-2.09865862325337,9.73516834281624,12.5763740061337));
#60482=CARTESIAN_POINT('Ctrl Pts',(-1.79280890371693,9.77495539237363,12.5790876950664));
#60483=CARTESIAN_POINT('Ctrl Pts',(-1.48603152505855,9.80541199434123,12.5810916990609));
#60484=CARTESIAN_POINT('Ctrl Pts',(-1.18132021538454,9.83566347870542,12.5830822065893));
#60485=CARTESIAN_POINT('Ctrl Pts',(-0.875693114117407,9.85670979197821,
12.5843724777896));
#60486=CARTESIAN_POINT('Ctrl Pts',(-0.569548332777583,9.86839321701482,
12.585068453806));
#60487=CARTESIAN_POINT('Ctrl Pts',(-0.379870270103967,9.87563191439401,
12.5854996595312));
#60488=CARTESIAN_POINT('Ctrl Pts',(-0.189993493543507,9.87927550563717,
12.5857026581081));
#60489=CARTESIAN_POINT('Ctrl Pts',(-1.38566163258134E-5,9.87927649678122,
12.5857020423665));
#60490=CARTESIAN_POINT('Ctrl Pts',(0.000267316804323126,9.87927649824813,
12.5857020414552));
#60491=CARTESIAN_POINT('Ctrl Pts',(0.000548489975148814,9.87927649178495,
12.5857020400583));
#60492=CARTESIAN_POINT('Ctrl Pts',(0.000829662895873392,9.87927647739157,
12.5857020381761));
#60493=CARTESIAN_POINT('Ctrl Pts',(0.298695167394001,9.87926122951397,12.5857000441388));
#60494=CARTESIAN_POINT('Ctrl Pts',(0.596280588157101,9.87035061745305,12.5851534870738));
#60495=CARTESIAN_POINT('Ctrl Pts',(0.893243902548241,9.8526544670475,12.5840196522909));
#60496=CARTESIAN_POINT('Ctrl Pts',(1.15817186246262,9.83686731490417,12.5830081316035));
#60497=CARTESIAN_POINT('Ctrl Pts',(1.4226048826074,9.81408706026283,12.5815292139631));
#60498=CARTESIAN_POINT('Ctrl Pts',(1.6862923402662,9.78435764326541,12.5795502474415));
#60499=CARTESIAN_POINT('Ctrl Pts',(1.92647727742504,9.7572780156764,12.5777476666366));
#60500=CARTESIAN_POINT('Ctrl Pts',(2.16604769956152,9.72445009753053,12.5755159664622));
#60501=CARTESIAN_POINT('Ctrl Pts',(2.40481940572151,9.68596137852757,12.5727677736108));
#60502=CARTESIAN_POINT('Ctrl Pts',(2.44417119287767,9.67961808139879,12.5723148459926));
#60503=CARTESIAN_POINT('Ctrl Pts',(2.48350129415924,9.67312097694517,12.5718478849593));
#60504=CARTESIAN_POINT('Ctrl Pts',(2.52280914060445,9.66647082366531,12.571366243551));
#60505=CARTESIAN_POINT('Ctrl Pts',(2.66171560913018,9.64297044420424,12.5696642142317));
#60506=CARTESIAN_POINT('Ctrl Pts',(2.80034190062008,9.61755692273634,12.5677807463362));
#60507=CARTESIAN_POINT('Ctrl Pts',(2.93865339111066,9.59025489483843,12.5656945718778));
#60508=CARTESIAN_POINT('Ctrl Pts',(3.00780913635596,9.57660388088948,12.5646514846486));
#60509=CARTESIAN_POINT('Ctrl Pts',(3.07688618068542,9.56248072941162,12.5635577069064));
#60510=CARTESIAN_POINT('Ctrl Pts',(3.14588026881465,9.54788887725495,12.5624101605141));
#60511=CARTESIAN_POINT('Ctrl Pts',(3.18037731287926,9.54059295117661,12.5618363873179));
#60512=CARTESIAN_POINT('Ctrl Pts',(3.2148536178259,9.53317984924622,12.5612491710932));
#60513=CARTESIAN_POINT('Ctrl Pts',(3.24930865362242,9.52565000838149,12.5606481127858));
#60514=CARTESIAN_POINT('Ctrl Pts',(3.26653617152068,9.52188508794913,12.5603475836321));
#60515=CARTESIAN_POINT('Ctrl Pts',(3.28375837212493,9.51809098274095,12.5600435939036));
#60516=CARTESIAN_POINT('Ctrl Pts',(3.30097518943068,9.51426774860628,12.5597360922117));
#60517=CARTESIAN_POINT('Ctrl Pts',(3.31819200673643,9.51044451447161,12.5594285905199));
#60518=CARTESIAN_POINT('Ctrl Pts',(3.3367571155512,9.50628678066224,12.5590928276944));
#60519=CARTESIAN_POINT('Ctrl Pts',(3.3526094255081,9.50271071554887,12.5588029992888));
#60520=CARTESIAN_POINT('Ctrl Pts',(3.64533816404849,9.43667510102825,12.5534510282646));
#60521=CARTESIAN_POINT('Ctrl Pts',(3.93428895180789,9.36270676548869,12.5471205564749));
#60522=CARTESIAN_POINT('Ctrl Pts',(4.21919428495158,9.28133608325902,12.5396851351043));
#60523=CARTESIAN_POINT('Ctrl Pts',(4.37443882435552,9.23699730607876,12.5356335838285));
#60524=CARTESIAN_POINT('Ctrl Pts',(4.52848250685322,9.19045977823743,12.5312541178136));
#60525=CARTESIAN_POINT('Ctrl Pts',(4.68128396609355,9.14180323426352,12.5265273067055));
#60526=CARTESIAN_POINT('Ctrl Pts',(4.9729361761219,9.04893246815381,12.5175052403395));
#60527=CARTESIAN_POINT('Ctrl Pts',(5.26006262434337,8.94834508993225,12.5072172317331));
#60528=CARTESIAN_POINT('Ctrl Pts',(5.54249832830085,8.84059374815403,12.4955147618435));
#60529=CARTESIAN_POINT('Ctrl Pts',(5.78171086995658,8.74933236734269,12.4856032048883));
#60530=CARTESIAN_POINT('Ctrl Pts',(6.01755870886431,8.65293089162241,12.4746771936492));
#60531=CARTESIAN_POINT('Ctrl Pts',(6.24994442165545,8.55169637580964,12.4626506151949));
#60532=CARTESIAN_POINT('Origin',(-6.52772161867356,9.09517583526925,13.2547520177953));
#60533=CARTESIAN_POINT('Ctrl Pts',(-7.10353236946292,7.16066185286935,14.3526205195542));
#60534=CARTESIAN_POINT('Ctrl Pts',(-7.10420293835514,7.21308870857396,14.3262172775605));
#60535=CARTESIAN_POINT('Ctrl Pts',(-7.09563107978587,7.3705695395524,14.2497542901758));
#60536=CARTESIAN_POINT('Ctrl Pts',(-7.02933623228066,7.63362087193247,14.1357461990317));
#60537=CARTESIAN_POINT('Ctrl Pts',(-6.87564852386692,7.92504962172612,14.0308126426424));
#60538=CARTESIAN_POINT('Ctrl Pts',(-6.66239699291616,8.17291221316709,13.9642188305442));
#60539=CARTESIAN_POINT('Ctrl Pts',(-6.44555610564831,8.33500242562356,13.9425618528397));
#60540=CARTESIAN_POINT('Ctrl Pts',(-6.30450358810212,8.40710732731462,13.9457940739706));
#60541=CARTESIAN_POINT('Ctrl Pts',(-6.25443531412204,8.42901391761335,13.9488692087856));
#60542=CARTESIAN_POINT('Ctrl Pts',(-6.81826428076322,6.90434192273487,13.8358832847937));
#60543=CARTESIAN_POINT('Ctrl Pts',(-6.81886755214442,6.95065173710113,13.8125514270221));
#60544=CARTESIAN_POINT('Ctrl Pts',(-6.81115710634597,7.09004574570647,13.7449862263706));
#60545=CARTESIAN_POINT('Ctrl Pts',(-6.75126038426607,7.32369230474132,13.6446049998666));
#60546=CARTESIAN_POINT('Ctrl Pts',(-6.61252933785919,7.58258619595588,13.5532653427725));
#60547=CARTESIAN_POINT('Ctrl Pts',(-6.42074067344956,7.80223546862304,13.4965368481301));
#60548=CARTESIAN_POINT('Ctrl Pts',(-6.22677981154663,7.94527355841214,13.4793227929944));
#60549=CARTESIAN_POINT('Ctrl Pts',(-6.10129479490154,8.00867147432692,13.483096339267));
#60550=CARTESIAN_POINT('Ctrl Pts',(-6.05684383053052,8.02791388513029,13.4860821707956));
#60551=CARTESIAN_POINT('Ctrl Pts',(-7.060874166321,6.6340016482441,13.304922676125));
#60552=CARTESIAN_POINT('Ctrl Pts',(-7.06166823277956,6.69385033520045,13.2747830501599));
#60553=CARTESIAN_POINT('Ctrl Pts',(-7.05151407295871,6.87300456587821,13.187783681333));
#60554=CARTESIAN_POINT('Ctrl Pts',(-6.97381583014319,7.17088697666304,13.058513067576));
#60555=CARTESIAN_POINT('Ctrl Pts',(-6.79329978326933,7.50214854137371,12.9389604953336));
#60556=CARTESIAN_POINT('Ctrl Pts',(-6.54058076329436,7.78676910420727,12.8623986671141));
#60557=CARTESIAN_POINT('Ctrl Pts',(-6.28027246344682,7.97577465832861,12.837429458236));
#60558=CARTESIAN_POINT('Ctrl Pts',(-6.10878315575702,8.06113488688539,12.841713067788));
#60559=CARTESIAN_POINT('Ctrl Pts',(-6.04762212113882,8.08722094161854,12.845572584902));
#60560=CARTESIAN_POINT('Ctrl Pts',(-7.66738794438976,6.53159212007938,13.1170811767575));
#60561=CARTESIAN_POINT('Ctrl Pts',(-7.66850215410177,6.6154980655897,13.0748492588303));
#60562=CARTESIAN_POINT('Ctrl Pts',(-7.65424811838746,6.86542480593276,12.9532002482573));
#60563=CARTESIAN_POINT('Ctrl Pts',(-7.54656095063027,7.27782973006081,12.7720225130049));
#60564=CARTESIAN_POINT('Ctrl Pts',(-7.29571415084507,7.73752000958537,12.6014925340904));
#60565=CARTESIAN_POINT('Ctrl Pts',(-6.94078600799892,8.1364481836985,12.488785652677));
#60566=CARTESIAN_POINT('Ctrl Pts',(-6.56967193451163,8.40541915029099,12.4490985003834));
#60567=CARTESIAN_POINT('Ctrl Pts',(-6.32164837097176,8.52859001388426,12.4535176928861));
#60568=CARTESIAN_POINT('Ctrl Pts',(-6.23272511332852,8.56640925874193,12.4586246319277));
#60569=CARTESIAN_POINT('',(-6.99999992462727,8.04448113171624,12.522061793522));
#60570=CARTESIAN_POINT('Ctrl Pts',(-6.99999977388181,8.04448088283872,12.522061406121));
#60571=CARTESIAN_POINT('Ctrl Pts',(-6.97337631313135,8.07076607346233,12.5155347659721));
#60572=CARTESIAN_POINT('Ctrl Pts',(-6.94625148402719,8.09633310306438,12.5095205719456));
#60573=CARTESIAN_POINT('Ctrl Pts',(-6.91864059243224,8.12119833195497,12.5040104271219));
#60574=CARTESIAN_POINT('Ctrl Pts',(-6.87585521537613,8.15972907588304,12.4954719986143));
#60575=CARTESIAN_POINT('Ctrl Pts',(-6.83190509173913,8.19657608428999,12.488142519529));
#60576=CARTESIAN_POINT('Ctrl Pts',(-6.78684501309333,8.23178719521259,12.4819974151937));
#60577=CARTESIAN_POINT('Ctrl Pts',(-6.74178493444752,8.26699830613518,12.4758523108585));
#60578=CARTESIAN_POINT('Ctrl Pts',(-6.69561423203128,8.30057401877221,12.4708914337041));
#60579=CARTESIAN_POINT('Ctrl Pts',(-6.64834300893827,8.33253226428265,12.4671176743163));
#60580=CARTESIAN_POINT('Ctrl Pts',(-6.60338098943086,8.36292934656748,12.4635282634208));
#60581=CARTESIAN_POINT('Ctrl Pts',(-6.55744285298859,8.39185759134211,12.4610091938602));
#60582=CARTESIAN_POINT('Ctrl Pts',(-6.5104998360318,8.41930782318824,12.4595867219062));
#60583=CARTESIAN_POINT('Ctrl Pts',(-6.5032227285201,8.42356315872726,12.4593662102729));
#60584=CARTESIAN_POINT('Ctrl Pts',(-6.49592142164987,8.4277829051022,12.4591721040651));
#60585=CARTESIAN_POINT('Ctrl Pts',(-6.48859575470359,8.43196694805737,12.4590045600572));
#60586=CARTESIAN_POINT('Ctrl Pts',(-6.44205415411054,8.45854910876866,12.4579401155015));
#60587=CARTESIAN_POINT('Ctrl Pts',(-6.3945306542809,8.48369338771844,12.4579456234358));
#60588=CARTESIAN_POINT('Ctrl Pts',(-6.34600963025918,8.50736035805974,12.4590572591614));
#60589=CARTESIAN_POINT('Ctrl Pts',(-6.31441415112375,8.5227716005612,12.4597811240031));
#60590=CARTESIAN_POINT('Ctrl Pts',(-6.2823953056962,8.53755565881508,12.4609745518824));
#60591=CARTESIAN_POINT('Ctrl Pts',(-6.2499459205233,8.55169191683731,12.4626538271208));
#60592=CARTESIAN_POINT('',(-6.9999915801407,6.97712494714797,13.9487134680504));
#60593=CARTESIAN_POINT('Ctrl Pts',(-6.99999158015451,6.9771362153215,13.9487146197636));
#60594=CARTESIAN_POINT('Ctrl Pts',(-6.99999158015451,6.98139583880415,13.9388762305162));
#60595=CARTESIAN_POINT('Ctrl Pts',(-7.,6.98228449209442,13.9352913921393));
#60596=CARTESIAN_POINT('Ctrl Pts',(-7.,6.9971931901372,13.9030475786216));
#60597=CARTESIAN_POINT('Ctrl Pts',(-7.00000000000326,7.03259754383002,13.8211717575672));
#60598=CARTESIAN_POINT('Ctrl Pts',(-7.00000000000326,7.11638182264416,13.6465448627553));
#60599=CARTESIAN_POINT('Ctrl Pts',(-7.,7.15192570282134,13.5765007476151));
#60600=CARTESIAN_POINT('Ctrl Pts',(-7.,7.26853858730711,13.3617723992316));
#60601=CARTESIAN_POINT('Ctrl Pts',(-7.,7.35673215220611,13.2193982896567));
#60602=CARTESIAN_POINT('Ctrl Pts',(-7.,7.66322934186235,12.8078043924259));
#60603=CARTESIAN_POINT('Ctrl Pts',(-7.,7.86763429655534,12.6356713199051));
#60604=CARTESIAN_POINT('Ctrl Pts',(-7.,8.04448084282976,12.5220613438382));
#60605=CARTESIAN_POINT('Ctrl Pts',(-6.9999915801407,6.97712494714797,13.9487134680504));
#60606=CARTESIAN_POINT('Ctrl Pts',(-6.99999179357842,7.02345511516882,13.9416137324713));
#60607=CARTESIAN_POINT('Ctrl Pts',(-6.99820050635823,7.06895925542468,13.9350275981178));
#60608=CARTESIAN_POINT('Ctrl Pts',(-6.99484214212171,7.11344412994376,13.9289647197009));
#60609=CARTESIAN_POINT('Ctrl Pts',(-6.99412245220856,7.12297713864213,13.9276654584731));
#60610=CARTESIAN_POINT('Ctrl Pts',(-6.99333067941413,7.13246348909142,13.9263902088819));
#60611=CARTESIAN_POINT('Ctrl Pts',(-6.99246885265765,7.14190152098239,13.925139034573));
#60612=CARTESIAN_POINT('Ctrl Pts',(-6.98828270432694,7.18774484291289,13.9190617096289));
#60613=CARTESIAN_POINT('Ctrl Pts',(-6.98244713497531,7.23244547821124,13.9135524609592));
#60614=CARTESIAN_POINT('Ctrl Pts',(-6.97524064834229,7.27587635862952,13.908587731437));
#60615=CARTESIAN_POINT('Ctrl Pts',(-6.96767039519366,7.3214995278626,13.9033723940317));
#60616=CARTESIAN_POINT('Ctrl Pts',(-6.95858694743669,7.3657214505831,13.8987580531846));
#60617=CARTESIAN_POINT('Ctrl Pts',(-6.9482703839507,7.40843320711306,13.8947152622816));
#60618=CARTESIAN_POINT('Ctrl Pts',(-6.94468364742794,7.42328270785089,13.8933097142223));
#60619=CARTESIAN_POINT('Ctrl Pts',(-6.9409475238705,7.43795000162698,13.8919732243342));
#60620=CARTESIAN_POINT('Ctrl Pts',(-6.93707278116213,7.45243154331358,13.8907044581386));
#60621=CARTESIAN_POINT('Ctrl Pts',(-6.93345734647906,7.46594394194718,13.8895206011308));
#60622=CARTESIAN_POINT('Ctrl Pts',(-6.92972121451281,7.47929463244384,13.8883956974777));
#60623=CARTESIAN_POINT('Ctrl Pts',(-6.92587277883775,7.49248113455884,13.8873286131981));
#60624=CARTESIAN_POINT('Ctrl Pts',(-6.91348381119123,7.53493140834987,13.8838934323268));
#60625=CARTESIAN_POINT('Ctrl Pts',(-6.89993442942445,7.57567800006318,13.8810573272698));
#60626=CARTESIAN_POINT('Ctrl Pts',(-6.88552314565712,7.61468928798206,13.8787588902026));
#60627=CARTESIAN_POINT('Ctrl Pts',(-6.87043421251612,7.65553497006394,13.8763523757105));
#60628=CARTESIAN_POINT('Ctrl Pts',(-6.8544001109962,7.69447831442104,13.8745353972937));
#60629=CARTESIAN_POINT('Ctrl Pts',(-6.83771752002407,7.73151542393473,13.8732375782579));
#60630=CARTESIAN_POINT('Ctrl Pts',(-6.83626070142977,7.73474971469382,13.8731242453285));
#60631=CARTESIAN_POINT('Ctrl Pts',(-6.83479891154535,7.73796948843846,13.8730148708164));
#60632=CARTESIAN_POINT('Ctrl Pts',(-6.83333233337493,7.74117475359548,13.8729094074551));
#60633=CARTESIAN_POINT('Ctrl Pts',(-6.82678505896167,7.75548408328111,13.8724385852504));
#60634=CARTESIAN_POINT('Ctrl Pts',(-6.82014241935267,7.76950420249532,13.8720457161995));
#60635=CARTESIAN_POINT('Ctrl Pts',(-6.81342017547794,7.78323627338698,13.8717265688566));
#60636=CARTESIAN_POINT('Ctrl Pts',(-6.81005905354057,7.79010230883282,13.8715669951852));
#60637=CARTESIAN_POINT('Ctrl Pts',(-6.80667802550112,7.7968963297535,13.8714258546653));
#60638=CARTESIAN_POINT('Ctrl Pts',(-6.80327897382311,7.80361856091292,13.8713026089469));
#60639=CARTESIAN_POINT('Ctrl Pts',(-6.8010541405342,7.80801856570131,13.8712219390415));
#60640=CARTESIAN_POINT('Ctrl Pts',(-6.79917315425435,7.81170206754556,13.8711605766567));
#60641=CARTESIAN_POINT('Ctrl Pts',(-6.79694806932509,7.81601686256903,13.8710945194426));
#60642=CARTESIAN_POINT('Ctrl Pts',(-6.79667926136544,7.81653812413135,13.8710865392056));
#60643=CARTESIAN_POINT('Ctrl Pts',(-6.79640538380907,7.81706856956299,13.8710785155005));
#60644=CARTESIAN_POINT('Ctrl Pts',(-6.79612518284729,7.81761054962054,13.8710704276006));
#60645=CARTESIAN_POINT('Ctrl Pts',(-6.79518125958311,7.81943633773277,13.8710431815956));
#60646=CARTESIAN_POINT('Ctrl Pts',(-6.79416569539586,7.82139310245855,13.8710151428786));
#60647=CARTESIAN_POINT('Ctrl Pts',(-6.79302961569968,7.8235701075631,13.8709860233455));
#60648=CARTESIAN_POINT('Ctrl Pts',(-6.76368963094169,7.87979265673828,13.8702339927812));
#60649=CARTESIAN_POINT('Ctrl Pts',(-6.73182093305379,7.93345140989508,13.8707651590374));
#60650=CARTESIAN_POINT('Ctrl Pts',(-6.69787436544692,7.98430705174562,13.8725913407545));
#60651=CARTESIAN_POINT('Ctrl Pts',(-6.67085582426605,8.02478375824305,13.8740448239607));
#60652=CARTESIAN_POINT('Ctrl Pts',(-6.64251966059964,8.06348488349544,13.8763192220685));
#60653=CARTESIAN_POINT('Ctrl Pts',(-6.6130719875628,8.10029601588777,13.8794277946745));
#60654=CARTESIAN_POINT('Ctrl Pts',(-6.57434521287239,8.14870651095385,13.8835158932748));
#60655=CARTESIAN_POINT('Ctrl Pts',(-6.53369822918461,8.19384839995991,13.8890457406106));
#60656=CARTESIAN_POINT('Ctrl Pts',(-6.49166404576566,8.23557412981306,13.8959769055419));
#60657=CARTESIAN_POINT('Ctrl Pts',(-6.45807128302675,8.26892038348224,13.9015161348096));
#60658=CARTESIAN_POINT('Ctrl Pts',(-6.42359132347886,8.30008482318858,13.9079509341316));
#60659=CARTESIAN_POINT('Ctrl Pts',(-6.38847438568453,8.32899839343566,13.9152673758578));
#60660=CARTESIAN_POINT('Ctrl Pts',(-6.3476522735808,8.36260932536996,13.9237724626651));
#60661=CARTESIAN_POINT('Ctrl Pts',(-6.30597044168472,8.39317911113965,13.9334683683526));
#60662=CARTESIAN_POINT('Ctrl Pts',(-6.26385540534517,8.42069809212293,13.9442719314227));
#60663=CARTESIAN_POINT('Ctrl Pts',(-6.22266933631966,7.49367505102186,13.1134072735229));
#60664=CARTESIAN_POINT('Ctrl Pts',(-6.22400486673781,7.81349730664259,13.3673816679581));
#60665=CARTESIAN_POINT('Ctrl Pts',(-6.22726445118346,8.61699336812186,14.0755188055406));
#60666=CARTESIAN_POINT('Ctrl Pts',(-6.23205297895451,9.75631511884638,15.3875857998101));
#60667=CARTESIAN_POINT('Ctrl Pts',(-6.23570680591364,10.7961444652413,17.0892590921569));
#60668=CARTESIAN_POINT('Ctrl Pts',(-6.23759597390816,11.541637417471,18.9411614085076));
#60669=CARTESIAN_POINT('Ctrl Pts',(-6.23804316716047,11.9701365581257,20.8893410093233));
#60670=CARTESIAN_POINT('Ctrl Pts',(-6.23649631643492,12.0627638071392,22.7260240074032));
#60671=CARTESIAN_POINT('Ctrl Pts',(-6.23490853076659,11.9504777429291,23.892461951891));
#60672=CARTESIAN_POINT('Ctrl Pts',(-6.23413323858226,11.8700330549955,24.3933787302679));
#60673=CARTESIAN_POINT('Ctrl Pts',(-6.71589075887148,7.42368503417367,13.2016810446589));
#60674=CARTESIAN_POINT('Ctrl Pts',(-6.71707947563242,7.74006436636922,13.453789394194));
#60675=CARTESIAN_POINT('Ctrl Pts',(-6.71993400051002,8.53485728885363,14.1564673243464));
#60676=CARTESIAN_POINT('Ctrl Pts',(-6.72416485221413,9.66125417255672,15.4573970130228));
#60677=CARTESIAN_POINT('Ctrl Pts',(-6.72736852339175,10.689155926356,17.143170277743));
#60678=CARTESIAN_POINT('Ctrl Pts',(-6.72902457707724,11.426258395907,18.9767998262514));
#60679=CARTESIAN_POINT('Ctrl Pts',(-6.72941957129847,11.8502298588172,20.9054834886988));
#60680=CARTESIAN_POINT('Ctrl Pts',(-6.72805203821864,11.9427120051071,22.7235306556374));
#60681=CARTESIAN_POINT('Ctrl Pts',(-6.72668376548171,11.8323442369596,23.8785262234885));
#60682=CARTESIAN_POINT('Ctrl Pts',(-6.72599062030542,11.7530859526059,24.3745538120327));
#60683=CARTESIAN_POINT('Ctrl Pts',(-7.02184862101457,7.17355760292472,13.5171491223171));
#60684=CARTESIAN_POINT('Ctrl Pts',(-7.02249157348648,7.478872844128,13.7610241429803));
#60685=CARTESIAN_POINT('Ctrl Pts',(-7.02397823406739,8.24599459896698,14.440704212245));
#60686=CARTESIAN_POINT('Ctrl Pts',(-7.0262282722894,9.33267229285362,15.6982356777953));
#60687=CARTESIAN_POINT('Ctrl Pts',(-7.02790162445773,10.3242143997312,17.3268265378416));
#60688=CARTESIAN_POINT('Ctrl Pts',(-7.0287661637212,11.0353397613724,19.0974453756984));
#60689=CARTESIAN_POINT('Ctrl Pts',(-7.028976081938,11.4446321919501,20.9601377844438));
#60690=CARTESIAN_POINT('Ctrl Pts',(-7.02824777989815,11.5344315703546,22.71520034539));
#60691=CARTESIAN_POINT('Ctrl Pts',(-7.02756283605818,11.4283603739875,23.8309174838911));
#60692=CARTESIAN_POINT('Ctrl Pts',(-7.02718415215858,11.3520777791479,24.3100040794306));
#60693=CARTESIAN_POINT('Ctrl Pts',(-6.99898915856098,6.85988137547321,13.9127665107488));
#60694=CARTESIAN_POINT('Ctrl Pts',(-6.99894180138027,7.1516676167299,14.1458797488553));
#60695=CARTESIAN_POINT('Ctrl Pts',(-6.99873531965576,7.88504568030388,14.7957455291437));
#60696=CARTESIAN_POINT('Ctrl Pts',(-6.99850468872881,8.92371894485393,15.9978491112633));
#60697=CARTESIAN_POINT('Ctrl Pts',(-6.99828080920108,9.87141264267925,17.5546291349416));
#60698=CARTESIAN_POINT('Ctrl Pts',(-6.99816434195365,10.5510797273584,19.2468680102348));
#60699=CARTESIAN_POINT('Ctrl Pts',(-6.99814257317328,10.9423828246477,21.0278308117662));
#60700=CARTESIAN_POINT('Ctrl Pts',(-6.99821546035646,11.0282138258093,22.7049155532659));
#60701=CARTESIAN_POINT('Ctrl Pts',(-6.99835922374124,10.9268166315182,23.7718253761471));
#60702=CARTESIAN_POINT('Ctrl Pts',(-6.99838072450059,10.8539129115264,24.2298152719421));
#60703=CARTESIAN_POINT('',(-7.00000355776417,10.9277699389974,24.1259406808918));
#60704=CARTESIAN_POINT('Ctrl Pts',(-7.00001601640884,6.97712293922472,13.9487170608442));
#60705=CARTESIAN_POINT('Ctrl Pts',(-7.00002088952752,7.14853164172674,14.0875671114257));
#60706=CARTESIAN_POINT('Ctrl Pts',(-7.000015982516,7.31421700914964,14.2303325311141));
#60707=CARTESIAN_POINT('Ctrl Pts',(-7.00000988103554,7.47407638767217,14.376420366171));
#60708=CARTESIAN_POINT('Ctrl Pts',(-7.00000652429656,7.56202327378949,14.4567908161979));
#60709=CARTESIAN_POINT('Ctrl Pts',(-7.00000279079959,7.64820743489774,14.5381675622895));
#60710=CARTESIAN_POINT('Ctrl Pts',(-6.99999999965548,7.73261611072525,14.6204569781481));
#60711=CARTESIAN_POINT('Ctrl Pts',(-6.99999455428923,7.89729272255631,14.7809990321527));
#60712=CARTESIAN_POINT('Ctrl Pts',(-6.99999266088549,8.05521000034952,14.9450123533677));
#60713=CARTESIAN_POINT('Ctrl Pts',(-6.99999257352085,8.20639703738741,15.1118865720018));
#60714=CARTESIAN_POINT('Ctrl Pts',(-6.99999248489117,8.35977324988939,15.281177115158));
#60715=CARTESIAN_POINT('Ctrl Pts',(-6.99999425322672,8.50622295743612,15.4534120257722));
#60716=CARTESIAN_POINT('Ctrl Pts',(-6.99999619758808,8.64580647529293,15.6279989379776));
#60717=CARTESIAN_POINT('Ctrl Pts',(-6.9999975442515,8.74248192916988,15.7489177200629));
#60718=CARTESIAN_POINT('Ctrl Pts',(-6.99999897835711,8.83586434207461,15.870965684437));
#60719=CARTESIAN_POINT('Ctrl Pts',(-6.99999998662364,8.92598174885412,15.9939582552016));
#60720=CARTESIAN_POINT('Ctrl Pts',(-7.0000014370777,9.05562123868325,16.1708907113886));
#60721=CARTESIAN_POINT('Ctrl Pts',(-7.00000201440511,9.17850354164596,16.3497755201176));
#60722=CARTESIAN_POINT('Ctrl Pts',(-7.0000021087437,9.29479363545964,16.5300313754151));
#60723=CARTESIAN_POINT('Ctrl Pts',(-7.00000220459648,9.41295025611371,16.7131804469875));
#60724=CARTESIAN_POINT('Ctrl Pts',(-7.00000180216161,9.52430140158153,16.8977449605128));
#60725=CARTESIAN_POINT('Ctrl Pts',(-7.00000129011683,9.62903794576636,17.0831664637562));
#60726=CARTESIAN_POINT('Ctrl Pts',(-7.00000086166955,9.71667498162649,17.2383156626862));
#60727=CARTESIAN_POINT('Ctrl Pts',(-7.00000035619204,9.79968127750393,17.3940658191389));
#60728=CARTESIAN_POINT('Ctrl Pts',(-6.99999998816694,9.87817756458936,17.5501163157672));
#60729=CARTESIAN_POINT('Ctrl Pts',(-6.99999970373616,9.93884396874961,17.6707210328739));
#60730=CARTESIAN_POINT('Ctrl Pts',(-6.99999950020192,9.99681674665053,17.7915056337493));
#60731=CARTESIAN_POINT('Ctrl Pts',(-6.99999936067802,10.0521635248232,17.9123401859273));
#60732=CARTESIAN_POINT('Ctrl Pts',(-6.99999924479307,10.0981331255442,18.0127022359021));
#60733=CARTESIAN_POINT('Ctrl Pts',(-6.99999917321886,10.142291206268,18.1130988977463));
#60734=CARTESIAN_POINT('Ctrl Pts',(-6.99999913936912,10.1846774087402,18.2134599710767));
#60735=CARTESIAN_POINT('Ctrl Pts',(-6.99999912244425,10.2058705099763,18.2636405077418));
#60736=CARTESIAN_POINT('Ctrl Pts',(-6.99999911499185,10.2266206416495,18.3138121472786));
#60737=CARTESIAN_POINT('Ctrl Pts',(-6.99999911640488,10.246932844701,18.3639665348978));
#60738=CARTESIAN_POINT('Ctrl Pts',(-6.9999991171114,10.2570889462268,18.3890437287075));
#60739=CARTESIAN_POINT('Ctrl Pts',(-6.99999912003648,10.2671355655972,18.4141166095378));
#60740=CARTESIAN_POINT('Ctrl Pts',(-6.99999912511644,10.2770733350148,18.4391841440791));
#60741=CARTESIAN_POINT('Ctrl Pts',(-6.99999912765642,10.2820422197236,18.4517179113498));
#60742=CARTESIAN_POINT('Ctrl Pts',(-6.99999913073525,10.2869838919442,18.4642503420482));
#60743=CARTESIAN_POINT('Ctrl Pts',(-6.99999913434566,10.291898430994,18.4767813084774));
#60744=CARTESIAN_POINT('Ctrl Pts',(-6.99999913750188,10.296194727389,18.48773589554));
#60745=CARTESIAN_POINT('Ctrl Pts',(-6.99999914057233,10.2999248874935,18.4972873011398));
#60746=CARTESIAN_POINT('Ctrl Pts',(-6.99999914483751,10.3045195539668,18.5091124088053));
#60747=CARTESIAN_POINT('Ctrl Pts',(-6.99999914545128,10.3051807324653,18.5108140572221));
#60748=CARTESIAN_POINT('Ctrl Pts',(-6.99999914609173,10.305859732172,18.5125628199288));
#60749=CARTESIAN_POINT('Ctrl Pts',(-6.9999991467648,10.3065607280344,18.514369687696));
#60750=CARTESIAN_POINT('Ctrl Pts',(-6.99999923697471,10.4005130113583,18.7565385241931));
#60751=CARTESIAN_POINT('Ctrl Pts',(-6.99999952144554,10.4851674501396,19.00016538121));
#60752=CARTESIAN_POINT('Ctrl Pts',(-6.99999999018483,10.5606734143179,19.2445368434734));
#60753=CARTESIAN_POINT('Ctrl Pts',(-7.0000004436457,10.6337182819468,19.4809430837961));
#60754=CARTESIAN_POINT('Ctrl Pts',(-7.00000106797418,10.698202212125,19.7180460706751));
#60755=CARTESIAN_POINT('Ctrl Pts',(-7.00000142593608,10.7543697313658,19.9551865164325));
#60756=CARTESIAN_POINT('Ctrl Pts',(-7.00000178766141,10.8111277673616,20.19482013633));
#60757=CARTESIAN_POINT('Ctrl Pts',(-7.00000187627638,10.8593936259894,20.4344920434748));
#60758=CARTESIAN_POINT('Ctrl Pts',(-7.00000131558951,10.8994259328862,20.6735748933678));
#60759=CARTESIAN_POINT('Ctrl Pts',(-7.0000010387301,10.9191933315174,20.7916306929476));
#60760=CARTESIAN_POINT('Ctrl Pts',(-7.00000060480743,10.9369532806506,20.9095436715295));
#60761=CARTESIAN_POINT('Ctrl Pts',(-6.99999997635849,10.9527374502756,21.0272429376326));
#60762=CARTESIAN_POINT('Ctrl Pts',(-6.99999887928608,10.980291601027,21.2327085020917));
#60763=CARTESIAN_POINT('Ctrl Pts',(-6.99999719588076,11.0018249275505,21.4375214622287));
#60764=CARTESIAN_POINT('Ctrl Pts',(-6.99999590265571,11.0175572494836,21.6413537925878));
#60765=CARTESIAN_POINT('Ctrl Pts',(-6.99999568173169,11.0202448310013,21.6761748448211));
#60766=CARTESIAN_POINT('Ctrl Pts',(-6.99999546003708,11.0229065683484,21.7128796154196));
#60767=CARTESIAN_POINT('Ctrl Pts',(-6.99999525389955,11.0254108669411,21.75013794005));
#60768=CARTESIAN_POINT('Ctrl Pts',(-6.99999512031371,11.0270337583356,21.7742829100596));
#60769=CARTESIAN_POINT('Ctrl Pts',(-6.99999499325482,11.0285915187921,21.7986602554154));
#60770=CARTESIAN_POINT('Ctrl Pts',(-6.99999487632675,11.0300601216929,21.8229070746112));
#60771=CARTESIAN_POINT('Ctrl Pts',(-6.9999945789659,11.0337949391971,21.8845693828506));
#60772=CARTESIAN_POINT('Ctrl Pts',(-6.99999434329384,11.0369990612,21.9460662528043));
#60773=CARTESIAN_POINT('Ctrl Pts',(-6.9999941942213,11.0396820511593,22.0073884345677));
#60774=CARTESIAN_POINT('Ctrl Pts',(-6.99999365475384,11.0493913227684,22.229302689719));
#60775=CARTESIAN_POINT('Ctrl Pts',(-6.9999942620196,11.0522757640116,22.4489301954425));
#60776=CARTESIAN_POINT('Ctrl Pts',(-6.99999708882545,11.0487792507388,22.6658974333243));
#60777=CARTESIAN_POINT('Ctrl Pts',(-6.99999738657601,11.0484109591607,22.6887508304715));
#60778=CARTESIAN_POINT('Ctrl Pts',(-6.99999770879879,11.0479718662955,22.7115747599508));
#60779=CARTESIAN_POINT('Ctrl Pts',(-6.99999805663954,11.0474624859708,22.7343688182385));
#60780=CARTESIAN_POINT('Ctrl Pts',(-6.9999986310883,11.0466212593786,22.7720125336482));
#60781=CARTESIAN_POINT('Ctrl Pts',(-6.9999992754144,11.0455883341832,22.809574777292));
#60782=CARTESIAN_POINT('Ctrl Pts',(-6.99999999465564,11.0443660188271,22.8470537692267));
#60783=CARTESIAN_POINT('Ctrl Pts',(-7.00000393353128,11.0376720921033,23.052304913658));
#60784=CARTESIAN_POINT('Ctrl Pts',(-7.00001006487307,11.025299318151,23.2550551439592));
#60785=CARTESIAN_POINT('Ctrl Pts',(-7.00001375756393,11.0076804835671,23.4549606777513));
#60786=CARTESIAN_POINT('Ctrl Pts',(-7.000017504741,10.9898016804802,23.6578158471807));
#60787=CARTESIAN_POINT('Ctrl Pts',(-7.00001874207249,10.9665208779502,23.8577418328988));
#60788=CARTESIAN_POINT('Ctrl Pts',(-7.00001328549311,10.938274975984,24.0544306054433));
#60789=CARTESIAN_POINT('Ctrl Pts',(-7.00001262288882,10.9348450147417,24.0783149504158));
#60790=CARTESIAN_POINT('Ctrl Pts',(-7.00001186234527,10.9313418208076,24.1021516203976));
#60791=CARTESIAN_POINT('Ctrl Pts',(-7.00001099700083,10.9277661612326,24.1259401133248));
#60792=CARTESIAN_POINT('Origin',(-5.99998362341993,10.9277594518961,24.125947303705));
#60793=CARTESIAN_POINT('Origin',(-5.999994993362,10.9277770074801,24.1259380195517));
#60794=CARTESIAN_POINT('Origin',(-6.,10.9277790634077,24.125942705097));
#60795=CARTESIAN_POINT('Ctrl Pts',(-5.9884183442854,11.3313022292381,25.0408390360803));
#60796=CARTESIAN_POINT('Ctrl Pts',(-5.98810619593714,11.2108096660665,25.0939098183863));
#60797=CARTESIAN_POINT('Ctrl Pts',(-5.98726411407663,10.7897530180886,25.2768810270768));
#60798=CARTESIAN_POINT('Ctrl Pts',(-5.98726411407568,10.2439464472041,25.5029615111316));
#60799=CARTESIAN_POINT('Ctrl Pts',(-5.98810619595882,9.81683424998038,25.6713133410833));
#60800=CARTESIAN_POINT('Ctrl Pts',(-5.98841834432643,9.69410642640033,25.7189877414102));
#60801=CARTESIAN_POINT('Ctrl Pts',(-6.58019637256003,11.3340652231778,25.047111700226));
#60802=CARTESIAN_POINT('Ctrl Pts',(-6.5798820750521,11.2136264141743,25.1003606676502));
#60803=CARTESIAN_POINT('Ctrl Pts',(-6.57903382472758,10.7926924751956,25.2838219693725));
#60804=CARTESIAN_POINT('Ctrl Pts',(-6.57903382472674,10.2467759245194,25.5099480085486));
#60805=CARTESIAN_POINT('Ctrl Pts',(-6.57988207507353,9.81940394754026,25.6778665220155));
#60806=CARTESIAN_POINT('Ctrl Pts',(-6.58019637260084,9.69658813799417,25.7253769164937));
#60807=CARTESIAN_POINT('Ctrl Pts',(-7.00079676143853,11.1662377150805,24.6661026672652));
#60808=CARTESIAN_POINT('Ctrl Pts',(-7.00061242393279,11.0471100806974,24.7189175646936));
#60809=CARTESIAN_POINT('Ctrl Pts',(-7.00011450599634,10.6307098582429,24.9007951477761));
#60810=CARTESIAN_POINT('Ctrl Pts',(-7.0001145059963,10.0904740685619,25.1245681387042));
#60811=CARTESIAN_POINT('Ctrl Pts',(-7.00061242394545,9.66742777151116,25.290400688646));
#60812=CARTESIAN_POINT('Ctrl Pts',(-7.00079676146261,9.54584603631305,25.3372908764602));
#60813=CARTESIAN_POINT('Ctrl Pts',(-6.99999917328613,10.927678046055,24.1245145225457));
#60814=CARTESIAN_POINT('Ctrl Pts',(-6.99999957798843,10.8103388551858,24.1765413802751));
#60815=CARTESIAN_POINT('Ctrl Pts',(-7.00000004346175,10.4001857821127,24.3557037853022));
#60816=CARTESIAN_POINT('Ctrl Pts',(-7.00000004346256,9.86804140738225,24.576125202425));
#60817=CARTESIAN_POINT('Ctrl Pts',(-6.99999957798869,9.45133243288797,24.7394602714692));
#60818=CARTESIAN_POINT('Ctrl Pts',(-6.99999917328596,9.33157254651437,24.7856430669351));
#60819=CARTESIAN_POINT('',(-7.00000356386834,9.33251602085003,24.7867164879855));
#60820=CARTESIAN_POINT('Origin',(-6.,9.33251101143585,24.7867243678371));
#60821=CARTESIAN_POINT('Origin',(-7.0002107682112,-4.74293616361314,-11.4504608650742));
#60822=CARTESIAN_POINT('Origin',(-5.999994980806,9.33250914740904,24.7867195890732));
#60823=CARTESIAN_POINT('Origin',(-5.99998370354292,9.33252808467289,24.7867138043456));
#60824=CARTESIAN_POINT('Ctrl Pts',(-6.23412989340402,8.85535213519231,25.6421122842036));
#60825=CARTESIAN_POINT('Ctrl Pts',(-6.23490519370591,8.44426394556272,25.3447917122089));
#60826=CARTESIAN_POINT('Ctrl Pts',(-6.23649298896613,7.54006566407591,24.5993912594835));
#60827=CARTESIAN_POINT('Ctrl Pts',(-6.23803984395223,6.30682932830241,23.2351599451));
#60828=CARTESIAN_POINT('Ctrl Pts',(-6.2375926509193,5.23225286032833,21.5545941421788));
#60829=CARTESIAN_POINT('Ctrl Pts',(-6.23570347947279,4.44990325945585,19.7179581728001));
#60830=CARTESIAN_POINT('Ctrl Pts',(-6.23204965637528,3.98190889009471,17.7794230915657));
#60831=CARTESIAN_POINT('Ctrl Pts',(-6.22726110625498,3.8597596825099,16.0460302370417));
#60832=CARTESIAN_POINT('Ctrl Pts',(-6.22400156292249,3.92718833567129,14.9771464147955));
#60833=CARTESIAN_POINT('Ctrl Pts',(-6.22266603698934,3.9737495101578,14.5714122610983));
#60834=CARTESIAN_POINT('Ctrl Pts',(-6.72598994962541,8.92473422419825,25.5461078251555));
#60835=CARTESIAN_POINT('Ctrl Pts',(-6.7266831066965,8.51794212602247,25.2514055028052));
#60836=CARTESIAN_POINT('Ctrl Pts',(-6.7280513688563,7.62319122749838,24.5127395435205));
#60837=CARTESIAN_POINT('Ctrl Pts',(-6.72941891797283,6.40302972279236,23.1617882479885));
#60838=CARTESIAN_POINT('Ctrl Pts',(-6.72902392012398,5.33903731288351,21.4982095508128));
#60839=CARTESIAN_POINT('Ctrl Pts',(-6.7273678628286,4.56367546252717,19.6804271754057));
#60840=CARTESIAN_POINT('Ctrl Pts',(-6.72416418641298,4.09848997856963,17.7615690069914));
#60841=CARTESIAN_POINT('Ctrl Pts',(-6.71993332126113,3.97507673802481,16.0451905115539));
#60842=CARTESIAN_POINT('Ctrl Pts',(-6.71707880685382,4.04021160935505,14.9863208404887));
#60843=CARTESIAN_POINT('Ctrl Pts',(-6.71589008825079,4.08565776872657,14.5843406421682));
#60844=CARTESIAN_POINT('Ctrl Pts',(-7.02718522642081,9.16264689799124,25.2169070753993));
#60845=CARTESIAN_POINT('Ctrl Pts',(-7.02756392064403,8.76993819821337,24.9320798125953));
#60846=CARTESIAN_POINT('Ctrl Pts',(-7.02824883165012,7.90599974588617,24.2181499613082));
#60847=CARTESIAN_POINT('Ctrl Pts',(-7.02897715373606,6.7284783391173,22.9136327893854));
#60848=CARTESIAN_POINT('Ctrl Pts',(-7.02876722992311,5.70076930069521,21.3070968357706));
#60849=CARTESIAN_POINT('Ctrl Pts',(-7.02790269246911,4.95159426737389,19.5522386119276));
#60850=CARTESIAN_POINT('Ctrl Pts',(-7.02622933538481,4.50113275642416,17.6995249184679));
#60851=CARTESIAN_POINT('Ctrl Pts',(-7.02397930905116,4.38032098780939,16.0419195542338));
#60852=CARTESIAN_POINT('Ctrl Pts',(-7.02249262973376,4.44215133384606,15.0188783064057));
#60853=CARTESIAN_POINT('Ctrl Pts',(-7.02184967226858,4.48559584516257,14.6305434540714));
#60854=CARTESIAN_POINT('Ctrl Pts',(-6.99838062538608,9.45820155481245,24.8079470509315));
#60855=CARTESIAN_POINT('Ctrl Pts',(-6.99835912980461,9.08279992667889,24.5356483167704));
#60856=CARTESIAN_POINT('Ctrl Pts',(-6.99821532184398,8.2566788241358,23.8529257033659));
#60857=CARTESIAN_POINT('Ctrl Pts',(-6.99814245121138,7.1314903406498,22.6063536230413));
#60858=CARTESIAN_POINT('Ctrl Pts',(-6.9981642146033,6.1488526955293,21.0703299396964));
#60859=CARTESIAN_POINT('Ctrl Pts',(-6.9982806895177,5.43285646000756,19.3931394441194));
#60860=CARTESIAN_POINT('Ctrl Pts',(-6.99850456865247,5.00216746505037,17.6222095472215));
#60861=CARTESIAN_POINT('Ctrl Pts',(-6.9987352349114,4.88660490348886,16.0377422203896));
#60862=CARTESIAN_POINT('Ctrl Pts',(-6.99894167917053,4.94565673237532,15.0596432877823));
#60863=CARTESIAN_POINT('Ctrl Pts',(-6.99898903104342,4.98714453063266,14.6884846342227));
#60864=CARTESIAN_POINT('',(-7.,4.92966193692261,14.7967990234135));
#60865=CARTESIAN_POINT('Ctrl Pts',(-7.00001101651645,9.33251828728899,24.7867134201296));
#60866=CARTESIAN_POINT('Ctrl Pts',(-7.00001786894295,9.17931983979782,24.6735516965421));
#60867=CARTESIAN_POINT('Ctrl Pts',(-7.00001802523628,9.03120918194217,24.5580124632972));
#60868=CARTESIAN_POINT('Ctrl Pts',(-7.00001556833393,8.88816179628229,24.4406082397738));
#60869=CARTESIAN_POINT('Ctrl Pts',(-7.00001306404844,8.74235563775587,24.3209397904152));
#60870=CARTESIAN_POINT('Ctrl Pts',(-7.0000078433619,8.60180983017618,24.1993336963811));
#60871=CARTESIAN_POINT('Ctrl Pts',(-7.00000354817398,8.4664648926225,24.0762902302008));
#60872=CARTESIAN_POINT('Ctrl Pts',(-7.00000225617386,8.42575289619948,24.0392785381084));
#60873=CARTESIAN_POINT('Ctrl Pts',(-7.00000104339817,8.38551126318123,24.0021365051628));
#60874=CARTESIAN_POINT('Ctrl Pts',(-6.99999999753967,8.34573781976912,23.964877022));
#60875=CARTESIAN_POINT('Ctrl Pts',(-6.99999887667098,8.30311177925403,23.9249452458545));
#60876=CARTESIAN_POINT('Ctrl Pts',(-6.99999794691815,8.26102348599585,23.8848785705131));
#60877=CARTESIAN_POINT('Ctrl Pts',(-6.99999718088437,8.21946771151489,23.8446921506738));
#60878=CARTESIAN_POINT('Ctrl Pts',(-6.99999462213106,8.08066055039311,23.7104589923891));
#60879=CARTESIAN_POINT('Ctrl Pts',(-6.99999387749955,7.94779642121724,23.5748934964743));
#60880=CARTESIAN_POINT('Ctrl Pts',(-6.99999403436534,7.82066688325193,23.4385283478739));
#60881=CARTESIAN_POINT('Ctrl Pts',(-6.99999406718762,7.79406655336375,23.409995577315));
#60882=CARTESIAN_POINT('Ctrl Pts',(-6.99999414005197,7.76771721764197,23.3814276290268));
#60883=CARTESIAN_POINT('Ctrl Pts',(-6.99999424550222,7.74161685943437,23.352829118262));
#60884=CARTESIAN_POINT('Ctrl Pts',(-6.99999432423845,7.72212858259807,23.3314755532857));
#60885=CARTESIAN_POINT('Ctrl Pts',(-6.99999441864875,7.70323903377222,23.3106151007504));
#60886=CARTESIAN_POINT('Ctrl Pts',(-6.9999945314086,7.68388235950719,23.2890695977729));
#60887=CARTESIAN_POINT('Ctrl Pts',(-6.99999463684072,7.66578358463525,23.2689242358912));
#60888=CARTESIAN_POINT('Ctrl Pts',(-6.99999475849199,7.64727647773833,23.2481798529943));
#60889=CARTESIAN_POINT('Ctrl Pts',(-6.99999490352853,7.62752043826751,23.2258462258222));
#60890=CARTESIAN_POINT('Ctrl Pts',(-6.99999520368191,7.58663527688044,23.1796267417684));
#60891=CARTESIAN_POINT('Ctrl Pts',(-6.99999556267868,7.54621521311681,23.1331494749869));
#60892=CARTESIAN_POINT('Ctrl Pts',(-6.99999595372411,7.50626134984804,23.0864242861152));
#60893=CARTESIAN_POINT('Ctrl Pts',(-6.99999673581497,7.42635362331049,22.992973908372));
#60894=CARTESIAN_POINT('Ctrl Pts',(-6.99999764539642,7.34831069875224,22.8985318422683));
#60895=CARTESIAN_POINT('Ctrl Pts',(-6.99999847634406,7.27213982922329,22.8031748296488));
#60896=CARTESIAN_POINT('Ctrl Pts',(-6.99999902467282,7.22187591795764,22.7402502962871));
#60897=CARTESIAN_POINT('Ctrl Pts',(-6.99999953898546,7.17242715196673,22.6769273058003));
#60898=CARTESIAN_POINT('Ctrl Pts',(-6.99999996276665,7.12379521756591,22.6132273646642));
#60899=CARTESIAN_POINT('Ctrl Pts',(-7.000001267365,6.97408319067755,22.4171289075978));
#60900=CARTESIAN_POINT('Ctrl Pts',(-7.00000171384827,6.83211409570069,22.2174616157779));
#60901=CARTESIAN_POINT('Ctrl Pts',(-7.00000170643154,6.69789322077232,22.0149182197186));
#60902=CARTESIAN_POINT('Ctrl Pts',(-7.00000169893551,6.56223720785845,21.8102091566455));
#60903=CARTESIAN_POINT('Ctrl Pts',(-7.00000122941501,6.43449595912778,21.6025621300187));
#60904=CARTESIAN_POINT('Ctrl Pts',(-7.00000072342875,6.31464981325747,21.3926452566123));
#60905=CARTESIAN_POINT('Ctrl Pts',(-7.00000046988977,6.25459745267091,21.2874603657385));
#60906=CARTESIAN_POINT('Ctrl Pts',(-7.00000020716712,6.19652700585555,21.1817048306048));
#60907=CARTESIAN_POINT('Ctrl Pts',(-6.9999999876651,6.14043371090483,21.0754583709577));
#60908=CARTESIAN_POINT('Ctrl Pts',(-6.99999993928858,6.12807119021431,21.0520424875293));
#60909=CARTESIAN_POINT('Ctrl Pts',(-6.99999989300536,6.11580469922885,21.0286027476278));
#60910=CARTESIAN_POINT('Ctrl Pts',(-6.99999984878286,6.10363403754539,21.0051400153112));
#60911=CARTESIAN_POINT('Ctrl Pts',(-6.99999965374465,6.0499567448507,20.901660353915));
#60912=CARTESIAN_POINT('Ctrl Pts',(-6.99999949863664,5.99814353340517,20.7977336628826));
#60913=CARTESIAN_POINT('Ctrl Pts',(-6.99999938184581,5.94817674612069,20.6934324333637));
#60914=CARTESIAN_POINT('Ctrl Pts',(-6.99999932345039,5.92319335247844,20.6412818186042));
#60915=CARTESIAN_POINT('Ctrl Pts',(-6.99999927466558,5.89867156487647,20.589037569223));
#60916=CARTESIAN_POINT('Ctrl Pts',(-6.99999923547373,5.87460909341309,20.5367084539057));
#60917=CARTESIAN_POINT('Ctrl Pts',(-6.9999992158778,5.86257785768141,20.510543896247));
#60918=CARTESIAN_POINT('Ctrl Pts',(-6.99999919868214,5.85066145098437,20.4843581221043));
#60919=CARTESIAN_POINT('Ctrl Pts',(-6.9999991838965,5.83885958468295,20.4581522189196));
#60920=CARTESIAN_POINT('Ctrl Pts',(-6.99999917283138,5.83002742864498,20.4385405219106));
#60921=CARTESIAN_POINT('Ctrl Pts',(-6.99999916268834,5.82084768949662,20.417992321048));
#60922=CARTESIAN_POINT('Ctrl Pts',(-6.99999915445987,5.81224564769479,20.3985848619336));
#60923=CARTESIAN_POINT('Ctrl Pts',(-6.99999915169314,5.80935331068039,20.3920593283864));
#60924=CARTESIAN_POINT('Ctrl Pts',(-6.99999914913284,5.80652587403082,20.3856629460377));
#60925=CARTESIAN_POINT('Ctrl Pts',(-6.99999914678746,5.80379731694203,20.3794752047448));
#60926=CARTESIAN_POINT('Ctrl Pts',(-6.99999907529424,5.72062370058133,20.1908565305928));
#60927=CARTESIAN_POINT('Ctrl Pts',(-6.99999912491859,5.64168481543872,19.9974674673488));
#60928=CARTESIAN_POINT('Ctrl Pts',(-6.99999933315959,5.56752048182436,19.7994484879038));
#60929=CARTESIAN_POINT('Ctrl Pts',(-6.99999947285733,5.5177675985959,19.6666081496818));
#60930=CARTESIAN_POINT('Ctrl Pts',(-6.99999968443233,5.47016400472382,19.5316850389696));
#60931=CARTESIAN_POINT('Ctrl Pts',(-6.9999999881677,5.42487991144661,19.3947326004997));
#60932=CARTESIAN_POINT('Ctrl Pts',(-7.00000042903665,5.35915048847276,19.1959474619658));
#60933=CARTESIAN_POINT('Ctrl Pts',(-7.00000106780692,5.2983069601726,18.9928846798482));
#60934=CARTESIAN_POINT('Ctrl Pts',(-7.00000153331199,5.24286429356814,18.7857670926481));
#60935=CARTESIAN_POINT('Ctrl Pts',(-7.00000199134801,5.18831120660947,18.5819727148307));
#60936=CARTESIAN_POINT('Ctrl Pts',(-7.0000022813202,5.13898707176438,18.3742525496783));
#60937=CARTESIAN_POINT('Ctrl Pts',(-7.00000202662856,5.0954046904489,18.1628637274833));
#60938=CARTESIAN_POINT('Ctrl Pts',(-7.00000181209397,5.05869391263252,17.9848044326435));
#60939=CARTESIAN_POINT('Ctrl Pts',(-7.00000121063182,5.02605739395554,17.8041428574034));
#60940=CARTESIAN_POINT('Ctrl Pts',(-6.99999998662441,4.99781410946024,17.6210585612637));
#60941=CARTESIAN_POINT('Ctrl Pts',(-6.99999852881493,4.96417597344145,17.4030026741207));
#60942=CARTESIAN_POINT('Ctrl Pts',(-6.9999961728693,4.93677017808673,17.1815088206562));
#60943=CARTESIAN_POINT('Ctrl Pts',(-6.99999449845864,4.91605392436374,16.9569202229915));
#60944=CARTESIAN_POINT('Ctrl Pts',(-6.99999284827044,4.8956373574151,16.7355805830434));
#60945=CARTESIAN_POINT('Ctrl Pts',(-6.99999186158996,4.88171821086046,16.5112350383155));
#60946=CARTESIAN_POINT('Ctrl Pts',(-6.99999320068044,4.87474433973957,16.2842614502171));
#60947=CARTESIAN_POINT('Ctrl Pts',(-6.99999413396,4.86988389785898,16.1260721297867));
#60948=CARTESIAN_POINT('Ctrl Pts',(-6.99999620011843,4.86839726354882,15.9666072810556));
#60949=CARTESIAN_POINT('Ctrl Pts',(-6.99999999965507,4.87043896665418,15.8060095551962));
#60950=CARTESIAN_POINT('Ctrl Pts',(-7.0000050688351,4.87316292001774,15.5917469063387));
#60951=CARTESIAN_POINT('Ctrl Pts',(-7.00001329848799,4.88216722682931,15.3754653522329));
#60952=CARTESIAN_POINT('Ctrl Pts',(-7.00001657716596,4.89779630351165,15.1576281480176));
#60953=CARTESIAN_POINT('Ctrl Pts',(-7.00001838079985,4.90639401651905,15.0377937008366));
#60954=CARTESIAN_POINT('Ctrl Pts',(-7.00001867122039,4.91699660060305,14.9174893752695));
#60955=CARTESIAN_POINT('Ctrl Pts',(-7.0000159872059,4.92966193666588,14.796799023232));
#60956=CARTESIAN_POINT('Ctrl Pts',(-6.26386075990253,3.90573694599532,15.8144217439117));
#60957=CARTESIAN_POINT('Ctrl Pts',(-6.27437424078817,3.90868760274242,15.8076587396846));
#60958=CARTESIAN_POINT('Ctrl Pts',(-6.28486073450179,3.91182238565663,15.8008093299079));
#60959=CARTESIAN_POINT('Ctrl Pts',(-6.29531386314359,3.91514200828217,15.7938746164386));
#60960=CARTESIAN_POINT('Ctrl Pts',(-6.33637970203193,3.92818337537731,15.766631114916));
#60961=CARTESIAN_POINT('Ctrl Pts',(-6.37693083405109,3.94408145526261,15.7380701969033));
#60962=CARTESIAN_POINT('Ctrl Pts',(-6.41657832582218,3.96284753712821,15.7082659326139));
#60963=CARTESIAN_POINT('Ctrl Pts',(-6.45584412580718,3.98143295537587,15.6787485980233));
#60964=CARTESIAN_POINT('Ctrl Pts',(-6.49422354029561,4.00283147356113,15.6480118989296));
#60965=CARTESIAN_POINT('Ctrl Pts',(-6.53133639222252,4.02700421041334,15.6161374338063));
#60966=CARTESIAN_POINT('Ctrl Pts',(-6.53913743592629,4.03208526904487,15.6094374880314));
#60967=CARTESIAN_POINT('Ctrl Pts',(-6.54688251210572,4.03728872113799,15.6026873013788));
#60968=CARTESIAN_POINT('Ctrl Pts',(-6.55456808012088,4.04261391242737,15.5958876755575));
#60969=CARTESIAN_POINT('Ctrl Pts',(-6.59048110957155,4.06749740200537,15.5641144660964));
#60970=CARTESIAN_POINT('Ctrl Pts',(-6.62509401715786,4.09504226037126,15.5312624561904));
#60971=CARTESIAN_POINT('Ctrl Pts',(-6.65805353180285,4.12515734110993,15.4974380911881));
#60972=CARTESIAN_POINT('Ctrl Pts',(-6.66665268310277,4.1330143784016,15.4886133000645));
#60973=CARTESIAN_POINT('Ctrl Pts',(-6.67513927108329,4.14104609822003,15.4797223433999));
#60974=CARTESIAN_POINT('Ctrl Pts',(-6.6835069874228,4.14925028383301,15.4707671487047));
#60975=CARTESIAN_POINT('Ctrl Pts',(-6.70372707170477,4.16907520592987,15.4491274582383));
#60976=CARTESIAN_POINT('Ctrl Pts',(-6.72325280714651,4.18990753989218,15.427113219735));
#60977=CARTESIAN_POINT('Ctrl Pts',(-6.74199680599635,4.2117111890082,15.404754774594));
#60978=CARTESIAN_POINT('Ctrl Pts',(-6.75136880542126,4.22261301356621,15.3935755520236));
#60979=CARTESIAN_POINT('Ctrl Pts',(-6.76054545271633,4.23375761324951,15.3823102742471));
#60980=CARTESIAN_POINT('Ctrl Pts',(-6.76951613170011,4.24514000632777,15.3709629941128));
#60981=CARTESIAN_POINT('Ctrl Pts',(-6.774001471192,4.2508312028669,15.3652893540456));
#60982=CARTESIAN_POINT('Ctrl Pts',(-6.77843532773899,4.25658185105849,15.3595952131745));
#60983=CARTESIAN_POINT('Ctrl Pts',(-6.78281636744521,4.26239126853153,15.3538811340133));
#60984=CARTESIAN_POINT('Ctrl Pts',(-6.78500688729832,4.26529597726805,15.3510240944326));
#60985=CARTESIAN_POINT('Ctrl Pts',(-6.78718420291574,4.2682153777334,15.3481620702732));
#60986=CARTESIAN_POINT('Ctrl Pts',(-6.78934814805164,4.27114938188087,15.3452951314681));
#60987=CARTESIAN_POINT('Ctrl Pts',(-6.79114832908272,4.27359017325018,15.3429101316044));
#60988=CARTESIAN_POINT('Ctrl Pts',(-6.79330664708345,4.27654724408184,15.3400288633611));
#60989=CARTESIAN_POINT('Ctrl Pts',(-6.79490577325515,4.27875757383909,15.3378814778922));
#60990=CARTESIAN_POINT('Ctrl Pts',(-6.79522891003434,4.2792042170442,15.3374475538928));
#60991=CARTESIAN_POINT('Ctrl Pts',(-6.79552935127015,4.27962025354817,15.3370435698547));
#60992=CARTESIAN_POINT('Ctrl Pts',(-6.79579970571376,4.27999511491821,15.336679641855));
#60993=CARTESIAN_POINT('Ctrl Pts',(-6.8103038065088,4.30010585185524,15.3171554634471));
#60994=CARTESIAN_POINT('Ctrl Pts',(-6.82466112344216,4.32154660532228,15.2967066172978));
#60995=CARTESIAN_POINT('Ctrl Pts',(-6.83868683916184,4.34442059427056,15.2753634668361));
#60996=CARTESIAN_POINT('Ctrl Pts',(-6.8523579833504,4.36671632643349,15.2545598734058));
#60997=CARTESIAN_POINT('Ctrl Pts',(-6.86571378715539,4.39037451869574,15.2329067157737));
#60998=CARTESIAN_POINT('Ctrl Pts',(-6.87854492101801,4.41546138438675,15.2104366111897));
#60999=CARTESIAN_POINT('Ctrl Pts',(-6.89092336821551,4.43966317712243,15.1887592593599));
#61000=CARTESIAN_POINT('Ctrl Pts',(-6.9028129530209,4.46519521373549,15.1663217176226));
#61001=CARTESIAN_POINT('Ctrl Pts',(-6.91399605182675,4.49207938040125,15.1431558653217));
#61002=CARTESIAN_POINT('Ctrl Pts',(-6.92152697963795,4.51018372893101,15.1275555058515));
#61003=CARTESIAN_POINT('Ctrl Pts',(-6.928736887252,4.52890048186552,15.1116249176021));
#61004=CARTESIAN_POINT('Ctrl Pts',(-6.93555357905215,4.54822416775344,15.0953740358282));
#61005=CARTESIAN_POINT('Ctrl Pts',(-6.94510274554621,4.5752937638614,15.0726089790698));
#61006=CARTESIAN_POINT('Ctrl Pts',(-6.95387447251374,4.60353495328979,15.0491954413136));
#61007=CARTESIAN_POINT('Ctrl Pts',(-6.96168682153978,4.63298567227641,15.0252248664936));
#61008=CARTESIAN_POINT('Ctrl Pts',(-6.96890749341195,4.6602059075082,15.0030697304666));
#61009=CARTESIAN_POINT('Ctrl Pts',(-6.97530773605332,4.68845969100606,14.9804388867761));
#61010=CARTESIAN_POINT('Ctrl Pts',(-6.98071683853119,4.71773610714928,14.957402693869));
#61011=CARTESIAN_POINT('Ctrl Pts',(-6.98600813822278,4.74637492335643,14.9348681974487));
#61012=CARTESIAN_POINT('Ctrl Pts',(-6.99035024736982,4.77599276568247,14.911945979747));
#61013=CARTESIAN_POINT('Ctrl Pts',(-6.99356765821133,4.80653286408542,14.8886977956708));
#61014=CARTESIAN_POINT('Ctrl Pts',(-6.99669733437195,4.83624017304388,14.8660835598566));
#61015=CARTESIAN_POINT('Ctrl Pts',(-6.99876194175778,4.86682028043261,14.8431610402342));
#61016=CARTESIAN_POINT('Ctrl Pts',(-6.99959682204669,4.89817205285958,14.8199808716854));
#61017=CARTESIAN_POINT('Ctrl Pts',(-6.99987412951937,4.90858561860223,14.8122815235968));
#61018=CARTESIAN_POINT('Ctrl Pts',(-7.0000157989355,4.91908390180451,14.8045536889217));
#61019=CARTESIAN_POINT('Ctrl Pts',(-7.0000159872059,4.92966193655724,14.7967990233117));
#61020=CARTESIAN_POINT('Ctrl Pts',(-6.24907873965842,3.90163420221723,15.8312168444344));
#61021=CARTESIAN_POINT('Ctrl Pts',(-6.29175678648451,3.91267140088817,15.8162585233033));
#61022=CARTESIAN_POINT('Ctrl Pts',(-6.42266965978749,3.95530760846479,15.7676241602702));
#61023=CARTESIAN_POINT('Ctrl Pts',(-6.62983849714768,4.0702747377564,15.6756774243267));
#61024=CARTESIAN_POINT('Ctrl Pts',(-6.84319911297757,4.2747492473435,15.553294548616));
#61025=CARTESIAN_POINT('Ctrl Pts',(-7.00357104976123,4.53497041307359,15.4263581296174));
#61026=CARTESIAN_POINT('Ctrl Pts',(-7.09151802900392,4.81587189318471,15.3108183618548));
#61027=CARTESIAN_POINT('Ctrl Pts',(-7.10724350840679,5.00645768800968,15.2433526903401));
#61028=CARTESIAN_POINT('Ctrl Pts',(-7.10592746249851,5.09162974565076,15.2153112980894));
#61029=CARTESIAN_POINT('Ctrl Pts',(-6.05068860243976,3.86152988210803,15.2178949522498));
#61030=CARTESIAN_POINT('Ctrl Pts',(-6.08843043831061,3.87101767241173,15.2046346505576));
#61031=CARTESIAN_POINT('Ctrl Pts',(-6.20441284673364,3.90776438456602,15.1614401205735));
#61032=CARTESIAN_POINT('Ctrl Pts',(-6.38893740513147,4.00756197392119,15.0793702464572));
#61033=CARTESIAN_POINT('Ctrl Pts',(-6.58005579450863,4.18649249103738,14.9697285938614));
#61034=CARTESIAN_POINT('Ctrl Pts',(-6.72429241821602,4.41551556330386,14.8559648014311));
#61035=CARTESIAN_POINT('Ctrl Pts',(-6.80352362709971,4.66352886406962,14.7527862461739));
#61036=CARTESIAN_POINT('Ctrl Pts',(-6.81764215739556,4.83172244359836,14.6930400233625));
#61037=CARTESIAN_POINT('Ctrl Pts',(-6.81646301824315,4.90672397733544,14.6683643944402));
#61038=CARTESIAN_POINT('Ctrl Pts',(-6.03817570823002,3.3653742336236,14.8043699886451));
#61039=CARTESIAN_POINT('Ctrl Pts',(-6.09017057840755,3.37836166406013,14.7864796423558));
#61040=CARTESIAN_POINT('Ctrl Pts',(-6.24902820060427,3.42842032220146,14.7286780918748));
#61041=CARTESIAN_POINT('Ctrl Pts',(-6.49746651777635,3.56211616729947,14.6212903640043));
#61042=CARTESIAN_POINT('Ctrl Pts',(-6.75008955648423,3.79671603666322,14.4808560682429));
#61043=CARTESIAN_POINT('Ctrl Pts',(-6.938221838207,4.09228824662061,14.3368904112171));
#61044=CARTESIAN_POINT('Ctrl Pts',(-7.04099372055609,4.40971738199054,14.2065130934989));
#61045=CARTESIAN_POINT('Ctrl Pts',(-7.05951570838809,4.62558997385974,14.1301183926698));
#61046=CARTESIAN_POINT('Ctrl Pts',(-7.05795834765348,4.7225588847146,14.0981910611585));
#61047=CARTESIAN_POINT('Ctrl Pts',(-6.22023196797387,2.74899963093355,14.8711973556313));
#61048=CARTESIAN_POINT('Ctrl Pts',(-6.29602853838421,2.76816901593314,14.8454805002066));
#61049=CARTESIAN_POINT('Ctrl Pts',(-6.52656687096162,2.84173846370411,14.7629046578067));
#61050=CARTESIAN_POINT('Ctrl Pts',(-6.88224706785488,3.03547585470201,14.6121278007695));
#61051=CARTESIAN_POINT('Ctrl Pts',(-7.2385216941781,3.36931140292561,14.4181924261346));
#61052=CARTESIAN_POINT('Ctrl Pts',(-7.50089116590327,3.78417613333916,14.2210755321012));
#61053=CARTESIAN_POINT('Ctrl Pts',(-7.64353817399801,4.22638305526497,14.0423330763607));
#61054=CARTESIAN_POINT('Ctrl Pts',(-7.66949567306553,4.52776300479599,13.9361805986748));
#61055=CARTESIAN_POINT('Ctrl Pts',(-7.66730078022939,4.66398161311348,13.8912880999727));
#61056=CARTESIAN_POINT('',(-7.00000002017424,3.16613029753958,14.5427413090324));
#61057=CARTESIAN_POINT('Ctrl Pts',(-7.,4.92966193692261,14.7967990234135));
#61058=CARTESIAN_POINT('Ctrl Pts',(-7.,4.82595068015789,14.7556187999394));
#61059=CARTESIAN_POINT('Ctrl Pts',(-7.,4.73230467693603,14.7209082500355));
#61060=CARTESIAN_POINT('Ctrl Pts',(-7.,4.65045299426906,14.6929800881805));
#61061=CARTESIAN_POINT('Ctrl Pts',(-7.,4.60952715293557,14.679016007253));
#61062=CARTESIAN_POINT('Ctrl Pts',(-7.,4.57156438471307,14.6666986894123));
#61063=CARTESIAN_POINT('Ctrl Pts',(-7.,4.536804100054,14.6558533229263));
#61064=CARTESIAN_POINT('Ctrl Pts',(-7.,4.51942395772447,14.6504306396834));
#61065=CARTESIAN_POINT('Ctrl Pts',(-7.,4.5028443894743,14.6453743550468));
#61066=CARTESIAN_POINT('Ctrl Pts',(-7.,4.48709423463723,14.6406556616635));
#61067=CARTESIAN_POINT('Ctrl Pts',(-7.,4.47921915721869,14.6382963149719));
#61068=CARTESIAN_POINT('Ctrl Pts',(-7.,4.47155143315342,14.6360213660936));
#61069=CARTESIAN_POINT('Ctrl Pts',(-7.,4.46409448566477,14.6338269308933));
#61070=CARTESIAN_POINT('Ctrl Pts',(-7.,4.46036601192044,14.6327297132932));
#61071=CARTESIAN_POINT('Ctrl Pts',(-7.,4.45669023232026,14.6316526241125));
#61072=CARTESIAN_POINT('Ctrl Pts',(-7.,4.45306756465829,14.6305951801213));
#61073=CARTESIAN_POINT('Ctrl Pts',(-7.,4.44944489699631,14.6295377361301));
#61074=CARTESIAN_POINT('Ctrl Pts',(-7.,4.44753558080656,14.6289809309358));
#61075=CARTESIAN_POINT('Ctrl Pts',(-7.,4.44235931122075,14.6274812983564));
#61076=CARTESIAN_POINT('Ctrl Pts',(-7.,4.35953899784779,14.603487177086));
#61077=CARTESIAN_POINT('Ctrl Pts',(-7.,4.27926853216976,14.5830032990511));
#61078=CARTESIAN_POINT('Ctrl Pts',(-7.,4.20217774711042,14.5661085517943));
#61079=CARTESIAN_POINT('Ctrl Pts',(-7.,4.12508696205109,14.5492138045375));
#61080=CARTESIAN_POINT('Ctrl Pts',(-7.,4.0527845638725,14.5361291043884));
#61081=CARTESIAN_POINT('Ctrl Pts',(-7.,3.98126344323272,14.5256474164678));
#61082=CARTESIAN_POINT('Ctrl Pts',(-7.,3.83822120195318,14.5046840406266));
#61083=CARTESIAN_POINT('Ctrl Pts',(-7.,3.69572435361907,14.4945099507662));
#61084=CARTESIAN_POINT('Ctrl Pts',(-7.,3.55810486077357,14.4974003670815));
#61085=CARTESIAN_POINT('Ctrl Pts',(-7.,3.42048536792807,14.5002907833969));
#61086=CARTESIAN_POINT('Ctrl Pts',(-7.,3.28796856453053,14.5162141391388));
#61087=CARTESIAN_POINT('Ctrl Pts',(-7.,3.16613072517763,14.542741284242));
#61088=CARTESIAN_POINT('Ctrl Pts',(-6.2499459998768,2.76546773691422,14.8593866472137));
#61089=CARTESIAN_POINT('Ctrl Pts',(-6.29701743055659,2.77824199061018,14.8431647544954));
#61090=CARTESIAN_POINT('Ctrl Pts',(-6.34322178177099,2.792709947018,14.8266893964536));
#61091=CARTESIAN_POINT('Ctrl Pts',(-6.38860511461875,2.80882516992212,14.8099544424063));
#61092=CARTESIAN_POINT('Ctrl Pts',(-6.40556261896127,2.81484663078076,14.8037014187053));
#61093=CARTESIAN_POINT('Ctrl Pts',(-6.4224053522873,2.82109856990858,14.7974120498922));
#61094=CARTESIAN_POINT('Ctrl Pts',(-6.43913510817571,2.82758028715883,14.7910856860475));
#61095=CARTESIAN_POINT('Ctrl Pts',(-6.46648688592921,2.83817736286468,14.7807426004089));
#61096=CARTESIAN_POINT('Ctrl Pts',(-6.49353686265284,2.84938831338855,14.7703006731512));
#61097=CARTESIAN_POINT('Ctrl Pts',(-6.52029720529596,2.86121064762762,14.7597553008202));
#61098=CARTESIAN_POINT('Ctrl Pts',(-6.59365016089588,2.89361692770002,14.7308493096417));
#61099=CARTESIAN_POINT('Ctrl Pts',(-6.66481622967055,2.93059441007357,14.7011737610307));
#61100=CARTESIAN_POINT('Ctrl Pts',(-6.73336338682278,2.97189481715064,14.6708725711793));
#61101=CARTESIAN_POINT('Ctrl Pts',(-6.7460546543055,2.9795414437233,14.6652624113795));
#61102=CARTESIAN_POINT('Ctrl Pts',(-6.75865601417981,2.987336308447,14.6596308188776));
#61103=CARTESIAN_POINT('Ctrl Pts',(-6.77116453647933,2.99527789980353,14.6539787286651));
#61104=CARTESIAN_POINT('Ctrl Pts',(-6.80197425854347,3.01483882127632,14.6400570739439));
#61105=CARTESIAN_POINT('Ctrl Pts',(-6.83222110171795,3.03529283448632,14.6260105120857));
#61106=CARTESIAN_POINT('Ctrl Pts',(-6.86190703099567,3.05665271147598,14.6118299629835));
#61107=CARTESIAN_POINT('Ctrl Pts',(-6.90200296541259,3.08550288554055,14.5926767014676));
#61108=CARTESIAN_POINT('Ctrl Pts',(-6.9410772764051,3.11600461962484,14.5732789530564));
#61109=CARTESIAN_POINT('Ctrl Pts',(-6.97913132965225,3.14820836614017,14.5536087616453));
#61110=CARTESIAN_POINT('Ctrl Pts',(-6.98612216659513,3.15412445448368,14.5499951886076));
#61111=CARTESIAN_POINT('Ctrl Pts',(-6.99307845882553,3.16009806955511,14.5463724203771));
#61112=CARTESIAN_POINT('Ctrl Pts',(-7.00000005853886,3.16612963662624,14.5427402846217));
#61113=CARTESIAN_POINT('Ctrl Pts',(7.10691982128491,-7.16634812687415,14.3573277946041));
#61114=CARTESIAN_POINT('Ctrl Pts',(7.10723242798241,-7.19552103167944,14.3426529330767));
#61115=CARTESIAN_POINT('Ctrl Pts',(7.1039242705972,-7.3187564684501,14.2819048781017));
#61116=CARTESIAN_POINT('Ctrl Pts',(7.06369615611098,-7.53922760006879,14.1823067263407));
#61117=CARTESIAN_POINT('Ctrl Pts',(6.94787920664715,-7.8127689334572,14.0761819460459));
#61118=CARTESIAN_POINT('Ctrl Pts',(6.77787455319756,-8.05682754693778,13.9995481841559));
#61119=CARTESIAN_POINT('Ctrl Pts',(6.56638861545542,-8.25893233176591,13.9558001011829));
#61120=CARTESIAN_POINT('Ctrl Pts',(6.38249370354767,-8.37571921190027,13.9481326205135));
#61121=CARTESIAN_POINT('Ctrl Pts',(6.27483013576736,-8.42598304509719,13.9530906703659));
#61122=CARTESIAN_POINT('Ctrl Pts',(6.25029140148474,-8.43656339435967,13.9546787322473));
#61123=CARTESIAN_POINT('Ctrl Pts',(6.81469559418484,-6.90842566153106,13.8380339234899));
#61124=CARTESIAN_POINT('Ctrl Pts',(6.81497660549222,-6.93407149048773,13.8251286161839));
#61125=CARTESIAN_POINT('Ctrl Pts',(6.81201885386562,-7.04253689015183,13.7717073504501));
#61126=CARTESIAN_POINT('Ctrl Pts',(6.77586367536613,-7.23730205240579,13.6842786040574));
#61127=CARTESIAN_POINT('Ctrl Pts',(6.6717314805588,-7.47924373358209,13.5919128736868));
#61128=CARTESIAN_POINT('Ctrl Pts',(6.5192820021909,-7.69478794234902,13.5262200739852));
#61129=CARTESIAN_POINT('Ctrl Pts',(6.33046962900436,-7.87269576845227,13.4898403370137));
#61130=CARTESIAN_POINT('Ctrl Pts',(6.16723164439068,-7.97503474134159,13.4846001443658));
#61131=CARTESIAN_POINT('Ctrl Pts',(6.07210359157714,-8.01895822338946,13.4895950828663));
#61132=CARTESIAN_POINT('Ctrl Pts',(6.05044504509845,-8.02819857653725,13.4911219087981));
#61133=CARTESIAN_POINT('Ctrl Pts',(7.05841184590234,-6.63607078428829,13.3013650836311));
#61134=CARTESIAN_POINT('Ctrl Pts',(7.0587777866451,-6.66928177922984,13.2846602023184));
#61135=CARTESIAN_POINT('Ctrl Pts',(7.05485772682236,-6.80931320231469,13.2156289903415));
#61136=CARTESIAN_POINT('Ctrl Pts',(7.00774539855559,-7.05851473581658,13.1029646382612));
#61137=CARTESIAN_POINT('Ctrl Pts',(6.87223084342461,-7.36801504029715,12.9826820888225));
#61138=CARTESIAN_POINT('Ctrl Pts',(6.67211859264277,-7.64608395178626,12.8952410504026));
#61139=CARTESIAN_POINT('Ctrl Pts',(6.42070776244213,-7.8789865058943,12.8449652134551));
#61140=CARTESIAN_POINT('Ctrl Pts',(6.19931043638224,-8.01568553558642,12.8364055904847));
#61141=CARTESIAN_POINT('Ctrl Pts',(6.06838347156874,-8.07522561979308,12.8426925700324));
#61142=CARTESIAN_POINT('Ctrl Pts',(6.03847420372112,-8.08779776067679,12.8446797960011));
#61143=CARTESIAN_POINT('Ctrl Pts',(7.67172816874031,-6.5351689148283,13.1136040700797));
#61144=CARTESIAN_POINT('Ctrl Pts',(7.67223759814686,-6.58187397818695,13.0901237528483));
#61145=CARTESIAN_POINT('Ctrl Pts',(7.66669930574663,-6.77826320004743,12.9931998819998));
#61146=CARTESIAN_POINT('Ctrl Pts',(7.60107815888014,-7.12488980375239,12.835118593979));
#61147=CARTESIAN_POINT('Ctrl Pts',(7.4125330539824,-7.55499723180348,12.6642970064452));
#61148=CARTESIAN_POINT('Ctrl Pts',(7.13207063067744,-7.94395590627747,12.5372620297768));
#61149=CARTESIAN_POINT('Ctrl Pts',(6.77551369413477,-8.27351015060811,12.4613099458292));
#61150=CARTESIAN_POINT('Ctrl Pts',(6.45683536720761,-8.46992594992077,12.4459497372264));
#61151=CARTESIAN_POINT('Ctrl Pts',(6.26620834906591,-8.55638102622129,12.4539020742517));
#61152=CARTESIAN_POINT('Ctrl Pts',(6.22254868972825,-8.57468274401025,12.4565571066556));
#61153=CARTESIAN_POINT('',(6.26385989014072,-8.4207183952526,13.9442649556632));
#61154=CARTESIAN_POINT('',(6.24999925108292,-8.5516700679197,12.4626498445719));
#61155=CARTESIAN_POINT('Origin',(6.527902330383,-9.095144289412,13.2547395928924));
#61156=CARTESIAN_POINT('',(6.99999925693877,-8.04450726878133,12.5220453001149));
#61157=CARTESIAN_POINT('Ctrl Pts',(6.99999932345931,-8.04450779086442,12.5220461127869));
#61158=CARTESIAN_POINT('Ctrl Pts',(6.93523191518207,-8.10843582533326,12.5061772190589));
#61159=CARTESIAN_POINT('Ctrl Pts',(6.86743938004946,-8.1682348981219,12.493290097609));
#61160=CARTESIAN_POINT('Ctrl Pts',(6.79657680503947,-8.22416384023962,12.483332862315));
#61161=CARTESIAN_POINT('Ctrl Pts',(6.78822731619943,-8.23075375145836,12.4821596361805));
#61162=CARTESIAN_POINT('Ctrl Pts',(6.77983520416841,-8.23728990558737,12.4810270335501));
#61163=CARTESIAN_POINT('Ctrl Pts',(6.77140039427982,-8.24377270394801,12.4799349282528));
#61164=CARTESIAN_POINT('Ctrl Pts',(6.69137888490863,-8.30527537165709,12.469574064708));
#61165=CARTESIAN_POINT('Ctrl Pts',(6.60751263574372,-8.36197566386238,12.4628589954802));
#61166=CARTESIAN_POINT('Ctrl Pts',(6.52054032183533,-8.41339421877647,12.459915588264));
#61167=CARTESIAN_POINT('Ctrl Pts',(6.44077171921804,-8.4605538962621,12.4572159765137));
#61168=CARTESIAN_POINT('Ctrl Pts',(6.35839158720097,-8.50327266058605,12.4576922431241));
#61169=CARTESIAN_POINT('Ctrl Pts',(6.27311920727313,-8.5414595618975,12.4615310781794));
#61170=CARTESIAN_POINT('Ctrl Pts',(6.26544704768595,-8.54489532856954,12.4618764673336));
#61171=CARTESIAN_POINT('Ctrl Pts',(6.25775147218604,-8.54829438959152,12.4622490480023));
#61172=CARTESIAN_POINT('Ctrl Pts',(6.25003227450165,-8.55165666657415,12.4626489390251));
#61173=CARTESIAN_POINT('',(6.99999053791474,-6.97711506405584,13.9486981655111));
#61174=CARTESIAN_POINT('Ctrl Pts',(6.999992895158,-6.97711506288399,13.9486981661339));
#61175=CARTESIAN_POINT('Ctrl Pts',(7.,-7.01455702470623,13.862138053422));
#61176=CARTESIAN_POINT('Ctrl Pts',(7.,-7.0801064098619,13.7187009838892));
#61177=CARTESIAN_POINT('Ctrl Pts',(7.,-7.1457012109594,13.5893393878538));
#61178=CARTESIAN_POINT('Ctrl Pts',(7.,-7.18319507671516,13.5188655305678));
#61179=CARTESIAN_POINT('Ctrl Pts',(7.,-7.19198611824022,13.5025948308775));
#61180=CARTESIAN_POINT('Ctrl Pts',(7.,-7.28161416552635,13.3396546434541));
#61181=CARTESIAN_POINT('Ctrl Pts',(7.,-7.36734370955451,13.2056023658641));
#61182=CARTESIAN_POINT('Ctrl Pts',(7.,-7.63342635361862,12.8482671475625));
#61183=CARTESIAN_POINT('Ctrl Pts',(7.,-7.82958249364545,12.660118225788));
#61184=CARTESIAN_POINT('Ctrl Pts',(6.999998447357,-8.04450634432302,12.5220438611068));
#61185=CARTESIAN_POINT('Ctrl Pts',(6.99997871935865,-6.97711506623554,13.9486981642574));
#61186=CARTESIAN_POINT('Ctrl Pts',(6.99998461169886,-7.00647256572936,13.944192975335));
#61187=CARTESIAN_POINT('Ctrl Pts',(6.99926918215788,-7.03549390394242,13.9398952854494));
#61188=CARTESIAN_POINT('Ctrl Pts',(6.9978867243848,-7.06412133653092,13.9358116282601));
#61189=CARTESIAN_POINT('Ctrl Pts',(6.99565943477728,-7.11024323937347,13.9292324130424));
#61190=CARTESIAN_POINT('Ctrl Pts',(6.99170320771225,-7.15534155737423,13.9232085050283));
#61191=CARTESIAN_POINT('Ctrl Pts',(6.98629128447007,-7.19927391203044,13.9177213839171));
#61192=CARTESIAN_POINT('Ctrl Pts',(6.98059873556339,-7.24548430088387,13.9119497378896));
#61193=CARTESIAN_POINT('Ctrl Pts',(6.9732952011298,-7.29040458299394,13.9067721201308));
#61194=CARTESIAN_POINT('Ctrl Pts',(6.96465598626061,-7.33390797762943,13.9021650165857));
#61195=CARTESIAN_POINT('Ctrl Pts',(6.96131166253051,-7.35074856293986,13.9003815621924));
#61196=CARTESIAN_POINT('Ctrl Pts',(6.95776677933511,-7.3673772269038,13.8986835707991));
#61197=CARTESIAN_POINT('Ctrl Pts',(6.95403590762787,-7.38378810741358,13.8970695411509));
#61198=CARTESIAN_POINT('Ctrl Pts',(6.94867965578311,-7.40734850184747,13.8947523482911));
#61199=CARTESIAN_POINT('Ctrl Pts',(6.94294025497593,-7.4304599269881,13.8926081951853));
#61200=CARTESIAN_POINT('Ctrl Pts',(6.93686495180243,-7.45311123350962,13.8906295633292));
#61201=CARTESIAN_POINT('Ctrl Pts',(6.92508574188899,-7.49702912315409,13.8867932576653));
#61202=CARTESIAN_POINT('Ctrl Pts',(6.91204633189904,-7.53921528441703,13.8835791656713));
#61203=CARTESIAN_POINT('Ctrl Pts',(6.89805485559285,-7.57961678769472,13.8809316931373));
#61204=CARTESIAN_POINT('Ctrl Pts',(6.8849547097132,-7.61744450330617,13.8784528784899));
#61205=CARTESIAN_POINT('Ctrl Pts',(6.87101910746412,-7.65370821014627,13.8764708448023));
#61206=CARTESIAN_POINT('Ctrl Pts',(6.85646977033409,-7.68839143484718,13.8749381971813));
#61207=CARTESIAN_POINT('Ctrl Pts',(6.84887976069648,-7.70648476840533,13.874138654899));
#61208=CARTESIAN_POINT('Ctrl Pts',(6.84112232443655,-7.72414843240078,13.8734613457473));
#61209=CARTESIAN_POINT('Ctrl Pts',(6.83322939388326,-7.74138491679247,13.8728974458017));
#61210=CARTESIAN_POINT('Ctrl Pts',(6.82669899579392,-7.7556459195947,13.8724308901792));
#61211=CARTESIAN_POINT('Ctrl Pts',(6.82007579813622,-7.76961452281618,13.8720419720816));
#61212=CARTESIAN_POINT('Ctrl Pts',(6.81337672309828,-7.78329277122056,13.8717257571408));
#61213=CARTESIAN_POINT('Ctrl Pts',(6.81002718557931,-7.79013189542275,13.8715676496704));
#61214=CARTESIAN_POINT('Ctrl Pts',(6.80665867083591,-7.79689842709432,13.871427722253));
#61215=CARTESIAN_POINT('Ctrl Pts',(6.80327319043602,-7.80359269140715,13.8713053571058));
#61216=CARTESIAN_POINT('Ctrl Pts',(6.80113746306185,-7.80781576224322,13.8712281631589));
#61217=CARTESIAN_POINT('Ctrl Pts',(6.79934549967287,-7.81132577461448,13.8711696878805));
#61218=CARTESIAN_POINT('Ctrl Pts',(6.79723646122255,-7.81541914235799,13.8711065106));
#61219=CARTESIAN_POINT('Ctrl Pts',(6.79600232562242,-7.8178144381175,13.8710695414633));
#61220=CARTESIAN_POINT('Ctrl Pts',(6.79465906404181,-7.82040915241095,13.8710312483486));
#61221=CARTESIAN_POINT('Ctrl Pts',(6.79306783305638,-7.82345899582193,13.8709903453484));
#61222=CARTESIAN_POINT('Ctrl Pts',(6.76770433410507,-7.87207211413368,13.8703383701076));
#61223=CARTESIAN_POINT('Ctrl Pts',(6.74051264580759,-7.91869839077715,13.8706400530389));
#61224=CARTESIAN_POINT('Ctrl Pts',(6.71177143962633,-7.9631738516196,13.8719116731427));
#61225=CARTESIAN_POINT('Ctrl Pts',(6.67920446635632,-8.01356947994824,13.8733525597104));
#61226=CARTESIAN_POINT('Ctrl Pts',(6.64464924538837,-8.06120381413504,13.8760382416814));
#61227=CARTESIAN_POINT('Ctrl Pts',(6.60855631925091,-8.10592857893428,13.8799422685215));
#61228=CARTESIAN_POINT('Ctrl Pts',(6.58247964648337,-8.13824164360055,13.8827628774685));
#61229=CARTESIAN_POINT('Ctrl Pts',(6.55559909698159,-8.16903621853364,13.8862198555525));
#61230=CARTESIAN_POINT('Ctrl Pts',(6.52806938950912,-8.19826223787322,13.8903070009252));
#61231=CARTESIAN_POINT('Ctrl Pts',(6.48890293382725,-8.23984203280442,13.896121773867));
#61232=CARTESIAN_POINT('Ctrl Pts',(6.44842494734317,-8.27824683059856,13.9032112200784));
#61233=CARTESIAN_POINT('Ctrl Pts',(6.40711341512205,-8.31342797164745,13.9115007136302));
#61234=CARTESIAN_POINT('Ctrl Pts',(6.37671580707502,-8.33931475140976,13.9176002398968));
#61235=CARTESIAN_POINT('Ctrl Pts',(6.34586575073266,-8.36345636015453,13.9243498879396));
#61236=CARTESIAN_POINT('Ctrl Pts',(6.31473704059775,-8.38583898722829,13.9317234455883));
#61237=CARTESIAN_POINT('Ctrl Pts',(6.29786789628842,-8.39796848968737,13.9357192940353));
#61238=CARTESIAN_POINT('Ctrl Pts',(6.28091670191048,-8.40958155320845,13.9398983834985));
#61239=CARTESIAN_POINT('Ctrl Pts',(6.26391275766735,-8.42068213410475,13.9442527024039));
#61240=CARTESIAN_POINT('Ctrl Pts',(6.99933866940308,-10.874321861748,24.2330493766441));
#61241=CARTESIAN_POINT('Ctrl Pts',(6.99933866940308,-10.8803485967835,24.1955798273128));
#61242=CARTESIAN_POINT('Ctrl Pts',(6.99933866940308,-10.9752955965243,23.5851351122749));
#61243=CARTESIAN_POINT('Ctrl Pts',(6.99933866940308,-11.0599204354475,22.3847684638779));
#61244=CARTESIAN_POINT('Ctrl Pts',(6.99933866940308,-10.904731832472,20.6450473295634));
#61245=CARTESIAN_POINT('Ctrl Pts',(6.99933866940308,-10.4757466585894,18.9490871086045));
#61246=CARTESIAN_POINT('Ctrl Pts',(6.99933866940308,-9.78232713548459,17.3424622371035));
#61247=CARTESIAN_POINT('Ctrl Pts',(6.99933866940308,-8.84436745984052,15.8669670641752));
#61248=CARTESIAN_POINT('Ctrl Pts',(6.99933866940308,-7.8388982304481,14.7344891895317));
#61249=CARTESIAN_POINT('Ctrl Pts',(6.99933866940308,-7.1385959671508,14.1224323391862));
#61250=CARTESIAN_POINT('Ctrl Pts',(6.99933866940308,-6.8652637212831,13.9057057530616));
#61251=CARTESIAN_POINT('Ctrl Pts',(7.01707119673726,-11.3554689991295,24.3104931498652));
#61252=CARTESIAN_POINT('Ctrl Pts',(7.01707119673726,-11.3617630889567,24.2713590868946));
#61253=CARTESIAN_POINT('Ctrl Pts',(7.01707119673726,-11.4609222058883,23.6338095273083));
#61254=CARTESIAN_POINT('Ctrl Pts',(7.01707119673726,-11.5493039149732,22.3805007967095));
#61255=CARTESIAN_POINT('Ctrl Pts',(7.01707119673726,-11.3871776978523,20.5627917354021));
#61256=CARTESIAN_POINT('Ctrl Pts',(7.01707119673726,-10.9391538957696,18.7917526334238));
#61257=CARTESIAN_POINT('Ctrl Pts',(7.01707119673726,-10.2148922939487,17.1135088397462));
#61258=CARTESIAN_POINT('Ctrl Pts',(7.01707119673726,-9.23504398166122,15.5722064363879));
#61259=CARTESIAN_POINT('Ctrl Pts',(7.01707119673726,-8.18492837750478,14.3894430108701));
#61260=CARTESIAN_POINT('Ctrl Pts',(7.01707119673726,-7.45357513988494,13.7502283468605));
#61261=CARTESIAN_POINT('Ctrl Pts',(7.01707119673726,-7.16803669166219,13.5238268590662));
#61262=CARTESIAN_POINT('Ctrl Pts',(6.72645657496606,-11.7431402439294,24.3728913678652));
#61263=CARTESIAN_POINT('Ctrl Pts',(6.72645657496606,-11.7496497476197,24.3324161682093));
#61264=CARTESIAN_POINT('Ctrl Pts',(6.72645657496606,-11.8522026636346,23.6730276159059));
#61265=CARTESIAN_POINT('Ctrl Pts',(6.72645657496606,-11.9436113688706,22.377062239736));
#61266=CARTESIAN_POINT('Ctrl Pts',(6.72645657496606,-11.7758953574806,20.4965165233067));
#61267=CARTESIAN_POINT('Ctrl Pts',(6.72645657496606,-11.3125316975443,18.664984651021));
#61268=CARTESIAN_POINT('Ctrl Pts',(6.72645657496606,-10.5634199280358,16.9290358549664));
#61269=CARTESIAN_POINT('Ctrl Pts',(6.72645657496606,-9.54982098387161,15.3347110620732));
#61270=CARTESIAN_POINT('Ctrl Pts',(6.72645657496606,-8.46373277521302,14.1114314189815));
#61271=CARTESIAN_POINT('Ctrl Pts',(6.72645657496606,-7.70736105793842,13.4503350838351));
#61272=CARTESIAN_POINT('Ctrl Pts',(6.72645657496606,-7.41198779351563,13.2161383066535));
#61273=CARTESIAN_POINT('Ctrl Pts',(6.2530336072437,-11.8653885094301,24.3925680243669));
#61274=CARTESIAN_POINT('Ctrl Pts',(6.2530336072437,-11.871965941738,24.3516699106168));
#61275=CARTESIAN_POINT('Ctrl Pts',(6.2530336072437,-11.9755890584896,23.6853946494987));
#61276=CARTESIAN_POINT('Ctrl Pts',(6.2530336072437,-12.0679522968085,22.3759779250414));
#61277=CARTESIAN_POINT('Ctrl Pts',(6.2530336072437,-11.8984735994768,20.4756172953318));
#61278=CARTESIAN_POINT('Ctrl Pts',(6.2530336072437,-11.4302726681641,18.6250096304905));
#61279=CARTESIAN_POINT('Ctrl Pts',(6.2530336072437,-10.6733246458032,16.8708641367243));
#61280=CARTESIAN_POINT('Ctrl Pts',(6.2530336072437,-9.64908277606497,15.2598192614479));
#61281=CARTESIAN_POINT('Ctrl Pts',(6.2530336072437,-8.55165096489382,14.023763232717));
#61282=CARTESIAN_POINT('Ctrl Pts',(6.2530336072437,-7.78738991926524,13.3557667305361));
#61283=CARTESIAN_POINT('Ctrl Pts',(6.2530336072437,-7.48891534351923,13.1191117864997));
#61284=CARTESIAN_POINT('',(6.99999999999999,-10.9277801898196,24.1259420764689));
#61285=CARTESIAN_POINT('Ctrl Pts',(6.99999999999999,-10.9277802009504,24.1259420781412));
#61286=CARTESIAN_POINT('Ctrl Pts',(6.99999999999999,-10.9521697295792,23.9636071725245));
#61287=CARTESIAN_POINT('Ctrl Pts',(7.00000000006069,-10.9728907817461,23.8012468908599));
#61288=CARTESIAN_POINT('Ctrl Pts',(6.9999999986734,-10.9899916559804,23.6387646053103));
#61289=CARTESIAN_POINT('Ctrl Pts',(6.99999999728326,-11.007127638005,23.4759487465215));
#61290=CARTESIAN_POINT('Ctrl Pts',(6.99999999422988,-11.0206285810772,23.3130099248014));
#61291=CARTESIAN_POINT('Ctrl Pts',(6.99999999314799,-11.0304911277933,23.1498445645567));
#61292=CARTESIAN_POINT('Ctrl Pts',(6.99999999206991,-11.0403189654241,22.9872534292619));
#61293=CARTESIAN_POINT('Ctrl Pts',(6.99999999472212,-11.0465339705917,22.8244368952001));
#61294=CARTESIAN_POINT('Ctrl Pts',(6.99999999803537,-11.0490812192129,22.6612929825452));
#61295=CARTESIAN_POINT('Ctrl Pts',(6.9999999990723,-11.0498784125077,22.6102350558974));
#61296=CARTESIAN_POINT('Ctrl Pts',(6.99999999999999,-11.050315984112,22.5591450947523));
#61297=CARTESIAN_POINT('Ctrl Pts',(6.99999999999999,-11.0503912041555,22.5080200916307));
#61298=CARTESIAN_POINT('Ctrl Pts',(6.99999999999999,-11.0504514191662,22.4670935982913));
#61299=CARTESIAN_POINT('Ctrl Pts',(6.99999999938395,-11.050284473563,22.4261442171503));
#61300=CARTESIAN_POINT('Ctrl Pts',(6.99999999847198,-11.0498891036841,22.3851771719374));
#61301=CARTESIAN_POINT('Ctrl Pts',(6.99999999416106,-11.0480201762815,22.1915245001614));
#61302=CARTESIAN_POINT('Ctrl Pts',(6.99999998574661,-11.0410429983283,21.9974766397485));
#61303=CARTESIAN_POINT('Ctrl Pts',(6.99999998500516,-11.0289287826382,21.8035275616802));
#61304=CARTESIAN_POINT('Ctrl Pts',(6.99999998426214,-11.0167889585745,21.6091684925233));
#61305=CARTESIAN_POINT('Ctrl Pts',(6.9999999898422,-10.9994903474747,21.4149090420219));
#61306=CARTESIAN_POINT('Ctrl Pts',(6.99999999472998,-10.9770562251435,21.2212489722765));
#61307=CARTESIAN_POINT('Ctrl Pts',(6.99999999759807,-10.9638921791236,21.107611806859));
#61308=CARTESIAN_POINT('Ctrl Pts',(6.99999999999999,-10.9489608647286,20.9941810381186));
#61309=CARTESIAN_POINT('Ctrl Pts',(6.99999999999999,-10.932275327311,20.8810571714478));
#61310=CARTESIAN_POINT('Ctrl Pts',(6.99999999999999,-10.9207674511519,20.8030365829761));
#61311=CARTESIAN_POINT('Ctrl Pts',(6.99999999890217,-10.9084190204695,20.7251635518545));
#61312=CARTESIAN_POINT('Ctrl Pts',(6.99999999758209,-10.8952326698626,20.6474486195686));
#61313=CARTESIAN_POINT('Ctrl Pts',(6.99999999346273,-10.8540842340522,20.4049366465432));
#61314=CARTESIAN_POINT('Ctrl Pts',(6.99999998925867,-10.8047802507612,20.1639637182118));
#61315=CARTESIAN_POINT('Ctrl Pts',(6.99999999152157,-10.7474287547034,19.9248987552727));
#61316=CARTESIAN_POINT('Ctrl Pts',(6.99999999354312,-10.6961940769102,19.7113312428321));
#61317=CARTESIAN_POINT('Ctrl Pts',(6.99999999999999,-10.638536191055,19.4992861507973));
#61318=CARTESIAN_POINT('Ctrl Pts',(6.99999999999999,-10.5744977406333,19.2890339660142));
#61319=CARTESIAN_POINT('Ctrl Pts',(6.99999999999999,-10.5402382199967,19.176552495647));
#61320=CARTESIAN_POINT('Ctrl Pts',(6.99999999803026,-10.5041671068588,19.064577502989));
#61321=CARTESIAN_POINT('Ctrl Pts',(6.9999999963631,-10.4662992290647,18.953187918004));
#61322=CARTESIAN_POINT('Ctrl Pts',(6.99999999271524,-10.383442022048,18.7094607687616));
#61323=CARTESIAN_POINT('Ctrl Pts',(6.9999999920498,-10.2919792980796,18.4685373660799));
#61324=CARTESIAN_POINT('Ctrl Pts',(6.99999999506633,-10.192229900311,18.2311614364419));
#61325=CARTESIAN_POINT('Ctrl Pts',(6.99999999705715,-10.126398300433,18.0745004683543));
#61326=CARTESIAN_POINT('Ctrl Pts',(6.99999999999999,-10.0569584112504,17.9193843975432));
#61327=CARTESIAN_POINT('Ctrl Pts',(6.99999999999999,-9.98401350683041,17.7660225963322));
#61328=CARTESIAN_POINT('Ctrl Pts',(6.99999999999999,-9.91676134047503,17.6246293975939));
#61329=CARTESIAN_POINT('Ctrl Pts',(6.99999999722473,-9.84651938466177,17.4847350710404));
#61330=CARTESIAN_POINT('Ctrl Pts',(6.99999999446462,-9.77332652212723,17.3464252545198));
#61331=CARTESIAN_POINT('Ctrl Pts',(6.99999999008266,-9.65712508822082,17.126843748257));
#61332=CARTESIAN_POINT('Ctrl Pts',(6.9999999878424,-9.53348786437254,16.9112542269386));
#61333=CARTESIAN_POINT('Ctrl Pts',(6.9999999926269,-9.40257758585834,16.7000150351235));
#61334=CARTESIAN_POINT('Ctrl Pts',(6.99999999531398,-9.32905545431275,16.5813783946359));
#61335=CARTESIAN_POINT('Ctrl Pts',(6.99999999999999,-9.25323851341331,16.464114496737));
#61336=CARTESIAN_POINT('Ctrl Pts',(6.99999999999999,-9.17515027025553,16.3482917014736));
#61337=CARTESIAN_POINT('Ctrl Pts',(6.99999999999999,-9.06614443700028,16.1866110207835));
#61338=CARTESIAN_POINT('Ctrl Pts',(6.99999999014829,-8.95275813323968,16.0276937647234));
#61339=CARTESIAN_POINT('Ctrl Pts',(6.99999998525269,-8.83523425972555,15.8719395760796));
#61340=CARTESIAN_POINT('Ctrl Pts',(6.9999999800339,-8.70995173852396,15.7059028649202));
#61341=CARTESIAN_POINT('Ctrl Pts',(6.99999998144993,-8.57996719499021,15.5434613062878));
#61342=CARTESIAN_POINT('Ctrl Pts',(6.99999998835927,-8.44567949375304,15.3850002973565));
#61343=CARTESIAN_POINT('Ctrl Pts',(6.99999999308627,-8.35380681241871,15.2765894924701));
#61344=CARTESIAN_POINT('Ctrl Pts',(6.99999999999999,-8.25992084841546,15.1700411226945));
#61345=CARTESIAN_POINT('Ctrl Pts',(6.99999999999999,-8.16415901451128,15.0654684229204));
#61346=CARTESIAN_POINT('Ctrl Pts',(6.99999999999999,-8.0515313796965,14.9424781316783));
#61347=CARTESIAN_POINT('Ctrl Pts',(6.99999999283346,-7.93626854432952,14.8222826805839));
#61348=CARTESIAN_POINT('Ctrl Pts',(6.99999999157248,-7.81832399166569,14.704766066323));
#61349=CARTESIAN_POINT('Ctrl Pts',(6.99999999107886,-7.77215394478804,14.6587635382978));
#61350=CARTESIAN_POINT('Ctrl Pts',(6.99999999110859,-7.72557250945403,14.6131718504097));
#61351=CARTESIAN_POINT('Ctrl Pts',(6.99999999149962,-7.67857521415048,14.5679854218538));
#61352=CARTESIAN_POINT('Ctrl Pts',(6.99999999249427,-7.55902957501349,14.4530460312539));
#61353=CARTESIAN_POINT('Ctrl Pts',(6.99999999550996,-7.43679567896384,14.3407261100692));
#61354=CARTESIAN_POINT('Ctrl Pts',(6.9999999971702,-7.31180057699937,14.2309835488546));
#61355=CARTESIAN_POINT('Ctrl Pts',(6.99999999862359,-7.2023786773616,14.1349138682792));
#61356=CARTESIAN_POINT('Ctrl Pts',(6.99999999923208,-7.09084007712802,14.0408196924531));
#61357=CARTESIAN_POINT('Ctrl Pts',(6.99999999922763,-6.97711506346271,13.9486981662434));
#61358=CARTESIAN_POINT('',(6.27159471697349,-11.879498130607,24.2690139179281));
#61359=CARTESIAN_POINT('Origin',(5.999999877384,-10.9277801432444,24.1259420367214));
#61360=CARTESIAN_POINT('Ctrl Pts',(6.27159470457059,-11.8794980693497,24.2690136413476));
#61361=CARTESIAN_POINT('Ctrl Pts',(6.27193966902461,-11.9138782752637,24.0395180963159));
#61362=CARTESIAN_POINT('Ctrl Pts',(6.27225782570503,-11.9412741979417,23.8113318898144));
#61363=CARTESIAN_POINT('Ctrl Pts',(6.2725491703234,-11.9620370299863,23.5849163366204));
#61364=CARTESIAN_POINT('Ctrl Pts',(6.27284515823024,-11.9831307684991,23.3548922982783));
#61365=CARTESIAN_POINT('Ctrl Pts',(6.27311347263771,-11.9973783339202,23.1266957546801));
#61366=CARTESIAN_POINT('Ctrl Pts',(6.27335410998336,-12.0051465975195,22.9007562103819));
#61367=CARTESIAN_POINT('Ctrl Pts',(6.27354178919894,-12.0112052648252,22.7245401857032));
#61368=CARTESIAN_POINT('Ctrl Pts',(6.27371263292358,-12.0133226538049,22.5496959438336));
#61369=CARTESIAN_POINT('Ctrl Pts',(6.27386663982658,-12.0116720606791,22.3764053057318));
#61370=CARTESIAN_POINT('Ctrl Pts',(6.27406868985895,-12.0095065577829,22.1490558924583));
#61371=CARTESIAN_POINT('Ctrl Pts',(6.27424175991821,-12.0008567741586,21.924382128493));
#61372=CARTESIAN_POINT('Ctrl Pts',(6.27438584775141,-11.9862080268575,21.702730216841));
#61373=CARTESIAN_POINT('Ctrl Pts',(6.27447251988024,-11.9773964701482,21.5694015199156));
#61374=CARTESIAN_POINT('Ctrl Pts',(6.27454870539273,-11.9664139927013,21.4371652340053));
#61375=CARTESIAN_POINT('Ctrl Pts',(6.27461440393747,-11.9533633920536,21.3060881202131));
#61376=CARTESIAN_POINT('Ctrl Pts',(6.27472591298159,-11.9312128252649,21.0836131214071));
#61377=CARTESIAN_POINT('Ctrl Pts',(6.27480721144035,-11.9031053991405,20.8644800898332));
#61378=CARTESIAN_POINT('Ctrl Pts',(6.27485829825228,-11.8695299765572,20.6489750513824));
#61379=CARTESIAN_POINT('Ctrl Pts',(6.27487121253493,-11.861042414286,20.5944973324769));
#61380=CARTESIAN_POINT('Ctrl Pts',(6.27488219619905,-11.852205343758,20.5402512077538));
#61381=CARTESIAN_POINT('Ctrl Pts',(6.27489124923553,-11.8430264894263,20.4862408043289));
#61382=CARTESIAN_POINT('Ctrl Pts',(6.2749281265656,-11.8056366433318,20.266230703004));
#61383=CARTESIAN_POINT('Ctrl Pts',(6.27493296851791,-11.7625774362594,20.0501357110777));
#61384=CARTESIAN_POINT('Ctrl Pts',(6.27490577502609,-11.7143927225912,19.8381799883121));
#61385=CARTESIAN_POINT('Ctrl Pts',(6.27488257562516,-11.6732852216319,19.6573556269408));
#61386=CARTESIAN_POINT('Ctrl Pts',(6.27483606022284,-11.6284468537051,19.4795430164125));
#61387=CARTESIAN_POINT('Ctrl Pts',(6.27476622928505,-11.580201581638,19.3048547409607));
#61388=CARTESIAN_POINT('Ctrl Pts',(6.27472435130897,-11.5512686414021,19.2000932748732));
#61389=CARTESIAN_POINT('Ctrl Pts',(6.27467408806462,-11.5211101803306,19.0964550027122));
#61390=CARTESIAN_POINT('Ctrl Pts',(6.27461544106535,-11.4897939376987,18.9939601886112));
#61391=CARTESIAN_POINT('Ctrl Pts',(6.27458611756572,-11.4741358163827,18.9427127815608));
#61392=CARTESIAN_POINT('Ctrl Pts',(6.27455469549538,-11.4581882408752,18.8917512417613));
#61393=CARTESIAN_POINT('Ctrl Pts',(6.27452117829932,-11.4419595134016,18.8410777748231));
#61394=CARTESIAN_POINT('Ctrl Pts',(6.27450441970129,-11.4338451496648,18.815741041354));
#61395=CARTESIAN_POINT('Ctrl Pts',(6.27448713714406,-11.42566049734,18.7904763262773));
#61396=CARTESIAN_POINT('Ctrl Pts',(6.27446933062821,-11.417406587565,18.7652838965214));
#61397=CARTESIAN_POINT('Ctrl Pts',(6.27445391884753,-11.410262716844,18.7434795073012));
#61398=CARTESIAN_POINT('Ctrl Pts',(6.27443872924805,-11.4033391852076,18.7225464152243));
#61399=CARTESIAN_POINT('Ctrl Pts',(6.27442216557726,-11.3959300847421,18.7003629482844));
#61400=CARTESIAN_POINT('Ctrl Pts',(6.27441959185747,-11.3947788333836,18.6969160053567));
#61401=CARTESIAN_POINT('Ctrl Pts',(6.27441698496212,-11.3936157619352,18.6934389053631));
#61402=CARTESIAN_POINT('Ctrl Pts',(6.27441433890278,-11.3924381130524,18.6899237251114));
#61403=CARTESIAN_POINT('Ctrl Pts',(6.27440279536136,-11.3873005719312,18.674588608375));
#61404=CARTESIAN_POINT('Ctrl Pts',(6.27439106194386,-11.3821286345952,18.659254378921));
#61405=CARTESIAN_POINT('Ctrl Pts',(6.27437913865126,-11.3769222139522,18.6439212020826));
#61406=CARTESIAN_POINT('Ctrl Pts',(6.27420010485628,-11.298745381651,18.4136864061409));
#61407=CARTESIAN_POINT('Ctrl Pts',(6.27397826087162,-11.2127926337038,18.1836848208436));
#61408=CARTESIAN_POINT('Ctrl Pts',(6.27371361097497,-11.1188661132799,17.954486037609));
#61409=CARTESIAN_POINT('Ctrl Pts',(6.27345238303172,-11.0261540734958,17.7282508208268));
#61410=CARTESIAN_POINT('Ctrl Pts',(6.27314944898001,-10.9256730981749,17.5027977428166));
#61411=CARTESIAN_POINT('Ctrl Pts',(6.27280481477215,-10.8172468333938,17.2787232728831));
#61412=CARTESIAN_POINT('Ctrl Pts',(6.27260797344829,-10.7553180723634,17.1507408663181));
#61413=CARTESIAN_POINT('Ctrl Pts',(6.27239752857088,-10.6907976264797,17.0232090921316));
#61414=CARTESIAN_POINT('Ctrl Pts',(6.27217348154728,-10.6236547832016,16.8962464403836));
#61415=CARTESIAN_POINT('Ctrl Pts',(6.27177013422557,-10.5027788814663,16.6676781482547));
#61416=CARTESIAN_POINT('Ctrl Pts',(6.27132270209057,-10.3734022583509,16.4409510714598));
#61417=CARTESIAN_POINT('Ctrl Pts',(6.27083119534451,-10.2354141323912,16.2167885889214));
#61418=CARTESIAN_POINT('Ctrl Pts',(6.27036732298328,-10.1051842254242,16.005229376537));
#61419=CARTESIAN_POINT('Ctrl Pts',(6.26986419337307,-9.9672840646058,15.7959548398425));
#61420=CARTESIAN_POINT('Ctrl Pts',(6.26932181699206,-9.82164027902969,15.5896211743922));
#61421=CARTESIAN_POINT('Ctrl Pts',(6.26905884654146,-9.7510250876935,15.4895805773476));
#61422=CARTESIAN_POINT('Ctrl Pts',(6.26878665006723,-9.67858983338576,15.3902320272094));
#61423=CARTESIAN_POINT('Ctrl Pts',(6.26850522898499,-9.60432785523052,15.2916544052724));
#61424=CARTESIAN_POINT('Ctrl Pts',(6.26791730417586,-9.44918503869204,15.0857130838198));
#61425=CARTESIAN_POINT('Ctrl Pts',(6.26728911874199,-9.28606733530127,14.8831340243101));
#61426=CARTESIAN_POINT('Ctrl Pts',(6.2666206878755,-9.11502762540494,14.6845502371122));
#61427=CARTESIAN_POINT('Ctrl Pts',(6.26595956710941,-8.94585844171389,14.4881382039364));
#61428=CARTESIAN_POINT('Ctrl Pts',(6.26525907633653,-8.76893953451425,14.2956345095279));
#61429=CARTESIAN_POINT('Ctrl Pts',(6.26451923361523,-8.58435346620896,14.1076918850216));
#61430=CARTESIAN_POINT('Ctrl Pts',(6.26430323028774,-8.5304620054781,14.0528204493752));
#61431=CARTESIAN_POINT('Ctrl Pts',(6.26408387263419,-8.47591720627682,13.9983380635825));
#61432=CARTESIAN_POINT('Ctrl Pts',(6.26386116116393,-8.42072164431578,13.9442616342516));
#61433=CARTESIAN_POINT('Ctrl Pts',(6.99999999998952,-9.33248386897495,24.7867299440625));
#61434=CARTESIAN_POINT('Ctrl Pts',(6.99999999998952,-9.33249195735398,24.786726802229));
#61435=CARTESIAN_POINT('Ctrl Pts',(6.99999999998952,-9.6023398658611,24.6819075264287));
#61436=CARTESIAN_POINT('Ctrl Pts',(6.99999999998952,-10.1365881548782,24.4674868371929));
#61437=CARTESIAN_POINT('Ctrl Pts',(6.99999999998952,-10.6659288230028,24.2412740854125));
#61438=CARTESIAN_POINT('Ctrl Pts',(6.99999999998952,-10.9277807259463,24.1259369152881));
#61439=CARTESIAN_POINT('Ctrl Pts',(7.00000270572501,-9.54650236979056,25.3377021349181));
#61440=CARTESIAN_POINT('Ctrl Pts',(7.00000270572501,-9.54651058116988,25.3376989453067));
#61441=CARTESIAN_POINT('Ctrl Pts',(7.00000270572501,-9.82046207618911,25.2312856794191));
#61442=CARTESIAN_POINT('Ctrl Pts',(7.00000270572501,-10.3628264314778,25.0136075514825));
#61443=CARTESIAN_POINT('Ctrl Pts',(7.00000270572501,-10.9002087461763,24.7839582708241));
#61444=CARTESIAN_POINT('Ctrl Pts',(7.00000270572501,-11.1660426386622,24.6668671647262));
#61445=CARTESIAN_POINT('Ctrl Pts',(6.57967198017911,-9.69699923069142,25.725143336737));
#61446=CARTESIAN_POINT('Ctrl Pts',(6.57967198017911,-9.69700752856398,25.7251401135283));
#61447=CARTESIAN_POINT('Ctrl Pts',(6.57967198017911,-9.97384464742507,25.617605960879));
#61448=CARTESIAN_POINT('Ctrl Pts',(6.57967198017911,-10.5219161845321,25.3976372164886));
#61449=CARTESIAN_POINT('Ctrl Pts',(6.57967198017911,-11.0649533494474,25.1655713839582));
#61450=CARTESIAN_POINT('Ctrl Pts',(6.57967198017911,-11.3335873593288,25.0472469178692));
#61451=CARTESIAN_POINT('Ctrl Pts',(5.98852436209622,-9.69454278461808,25.7188194279643));
#61452=CARTESIAN_POINT('Ctrl Pts',(5.98852436209622,-9.69455108107887,25.718816205304));
#61453=CARTESIAN_POINT('Ctrl Pts',(5.98852436209622,-9.97134110008892,25.6113003480331));
#61454=CARTESIAN_POINT('Ctrl Pts',(5.98852436209622,-10.519319483198,25.3913689916389));
#61455=CARTESIAN_POINT('Ctrl Pts',(5.98852436209622,-11.0622643482839,25.1593426026514));
#61456=CARTESIAN_POINT('Ctrl Pts',(5.98852436209622,-11.3308526539734,25.0410382677614));
#61457=CARTESIAN_POINT('',(6.99999999994033,-9.33250873275173,24.7867180660544));
#61458=CARTESIAN_POINT('',(5.98852583803188,-9.69456766153457,25.7188097331067));
#61459=CARTESIAN_POINT('Origin',(5.999999999061,-9.33250979146063,24.7867247845918));
#61460=CARTESIAN_POINT('',(5.98852581752181,-11.3308503373093,25.0410389569969));
#61461=CARTESIAN_POINT('Origin',(5.98846855648545,4.75314843273632,-11.4751154999728));
#61462=CARTESIAN_POINT('Origin',(6.,-10.9277801936245,24.1259421517584));
#61463=CARTESIAN_POINT('Origin',(6.99999997873566,4.74946019458188,-11.4664777699154));
#61464=CARTESIAN_POINT('Origin',(5.999999877384,-10.9277801432444,24.1259420367214));
#61465=CARTESIAN_POINT('Origin',(5.99999763271771,-10.927779210435,24.1259401188868));
#61466=CARTESIAN_POINT('Ctrl Pts',(-6.09474589299296,-11.2721661211721,
25.0678864406018));
#61467=CARTESIAN_POINT('Ctrl Pts',(-6.05665088594491,-11.2844331672992,
25.0619829591023));
#61468=CARTESIAN_POINT('Ctrl Pts',(-5.71262397471385,-11.3942435667727,
25.0092456877338));
#61469=CARTESIAN_POINT('Ctrl Pts',(-5.02648233484312,-11.5958351263256,
24.9142565089414));
#61470=CARTESIAN_POINT('Ctrl Pts',(-3.98603640523322,-11.8499663881965,
24.7972465440184));
#61471=CARTESIAN_POINT('Ctrl Pts',(-2.81241127776029,-12.0696726758818,
24.6980993235061));
#61472=CARTESIAN_POINT('Ctrl Pts',(-1.52058000263906,-12.2260603896697,
24.6290271692427));
#61473=CARTESIAN_POINT('Ctrl Pts',(-0.18943338566882,-12.2892377815174,
24.6021117442546));
#61474=CARTESIAN_POINT('Ctrl Pts',(1.08611700923628,-12.2543717429925,24.6168486008321));
#61475=CARTESIAN_POINT('Ctrl Pts',(2.24134999476999,-12.1455614154255,24.6644539540119));
#61476=CARTESIAN_POINT('Ctrl Pts',(3.27313427271148,-11.9878599489094,24.7348915555515));
#61477=CARTESIAN_POINT('Ctrl Pts',(4.20017951060728,-11.7988850751499,24.8206976463489));
#61478=CARTESIAN_POINT('Ctrl Pts',(5.05727095054733,-11.5852913554165,24.9192987376905));
#61479=CARTESIAN_POINT('Ctrl Pts',(5.68075726226311,-11.403640393652,25.004824199225));
#61480=CARTESIAN_POINT('Ctrl Pts',(6.02267051912257,-11.2953816471556,25.0567121658076));
#61481=CARTESIAN_POINT('Ctrl Pts',(6.09461115805388,-11.2722173874739,25.0678609837662));
#61482=CARTESIAN_POINT('Ctrl Pts',(-6.21870783125079,-11.6030071289173,
24.9346094928434));
#61483=CARTESIAN_POINT('Ctrl Pts',(-6.17988419054913,-11.6154566213683,
24.9284813863121));
#61484=CARTESIAN_POINT('Ctrl Pts',(-5.82927340985939,-11.7268865197749,
24.8737036247638));
#61485=CARTESIAN_POINT('Ctrl Pts',(-5.12991816585638,-11.9312122509951,
24.7744497244118));
#61486=CARTESIAN_POINT('Ctrl Pts',(-4.06889120378561,-12.1883443489005,
24.6509624758045));
#61487=CARTESIAN_POINT('Ctrl Pts',(-2.8713420059513,-12.4102486289105,24.5452756161874));
#61488=CARTESIAN_POINT('Ctrl Pts',(-1.55249930391971,-12.5678336068868,
24.4708055953072));
#61489=CARTESIAN_POINT('Ctrl Pts',(-0.193370339803287,-12.631221050945,
24.4412527778677));
#61490=CARTESIAN_POINT('Ctrl Pts',(1.10886668231814,-12.5962715383566,24.4574968110138));
#61491=CARTESIAN_POINT('Ctrl Pts',(2.28838800899833,-12.4867526600937,24.5090736087206));
#61492=CARTESIAN_POINT('Ctrl Pts',(3.34149766488906,-12.3276452266319,24.5845653347974));
#61493=CARTESIAN_POINT('Ctrl Pts',(4.28728535808482,-12.1366714881359,24.6757451511196));
#61494=CARTESIAN_POINT('Ctrl Pts',(5.16128278679853,-11.9205124015365,24.7796819536751));
#61495=CARTESIAN_POINT('Ctrl Pts',(5.79679487909143,-11.7364122164643,24.8690883834396));
#61496=CARTESIAN_POINT('Ctrl Pts',(6.14525360451488,-11.6265672049225,24.9230077699474));
#61497=CARTESIAN_POINT('Ctrl Pts',(6.21857044990854,-11.6030581495952,24.934580419999));
#61498=CARTESIAN_POINT('Ctrl Pts',(-6.32920995303496,-11.8134825706664,
24.6410481436331));
#61499=CARTESIAN_POINT('Ctrl Pts',(-6.28968289989913,-11.8260512681113,
24.6347407922777));
#61500=CARTESIAN_POINT('Ctrl Pts',(-5.93272838617964,-11.9385158037939,
24.5783421587689));
#61501=CARTESIAN_POINT('Ctrl Pts',(-5.22085586767563,-12.1441818047848,
24.4758249486542));
#61502=CARTESIAN_POINT('Ctrl Pts',(-4.14083998302221,-12.4019390210003,
24.3475960658914));
#61503=CARTESIAN_POINT('Ctrl Pts',(-2.92182894542457,-12.6234699451084,
24.2372880454582));
#61504=CARTESIAN_POINT('Ctrl Pts',(-1.57943400594235,-12.7800180096094,
24.1591267156643));
#61505=CARTESIAN_POINT('Ctrl Pts',(-0.19663864163009,-12.8424707279084,
24.1278317350971));
#61506=CARTESIAN_POINT('Ctrl Pts',(1.12797187797457,-12.8080965926766,24.1450661652523));
#61507=CARTESIAN_POINT('Ctrl Pts',(2.32846266169234,-12.6995389486587,24.1993284835348));
#61508=CARTESIAN_POINT('Ctrl Pts',(3.4004058329485,-12.5410674609128,24.2783326775672));
#61509=CARTESIAN_POINT('Ctrl Pts',(4.36314548455404,-12.3501685854821,24.3733486865178));
#61510=CARTESIAN_POINT('Ctrl Pts',(5.25278011477892,-12.1333806487397,24.4812087583929));
#61511=CARTESIAN_POINT('Ctrl Pts',(5.89967149746468,-11.948107139288,24.573578404262));
#61512=CARTESIAN_POINT('Ctrl Pts',(6.25442391879544,-11.8372665858876,24.6291055563114));
#61513=CARTESIAN_POINT('Ctrl Pts',(6.32906931217782,-11.8135319788164,24.6410164748022));
#61514=CARTESIAN_POINT('Ctrl Pts',(-6.39488492041273,-11.8436591114854,
24.2701454690196));
#61515=CARTESIAN_POINT('Ctrl Pts',(-6.35487922842965,-11.8562498384674,
24.2637551803992));
#61516=CARTESIAN_POINT('Ctrl Pts',(-5.99362080848964,-11.9688695480746,
24.2066158363988));
#61517=CARTESIAN_POINT('Ctrl Pts',(-5.27347888337443,-12.1740990310879,
24.1027642521193));
#61518=CARTESIAN_POINT('Ctrl Pts',(-4.18145499098206,-12.4299236517987,
23.972877644657));
#61519=CARTESIAN_POINT('Ctrl Pts',(-2.94953624141899,-12.6486106768879,
23.8611813945531));
#61520=CARTESIAN_POINT('Ctrl Pts',(-1.5937350037576,-12.8021773211153,23.7820856217206));
#61521=CARTESIAN_POINT('Ctrl Pts',(-0.198310009722217,-12.8628133789537,
23.7504395921336));
#61522=CARTESIAN_POINT('Ctrl Pts',(1.13800675393286,-12.8295115867388,23.7678657201884));
#61523=CARTESIAN_POINT('Ctrl Pts',(2.35019416885011,-12.7233156388094,23.8227634215804));
#61524=CARTESIAN_POINT('Ctrl Pts',(3.43313248483788,-12.5673456810811,23.9027391680116));
#61525=CARTESIAN_POINT('Ctrl Pts',(4.40622212620569,-12.3785782658713,23.9989627708025));
#61526=CARTESIAN_POINT('Ctrl Pts',(5.30578762347871,-12.1632801814373,24.1082181549124));
#61527=CARTESIAN_POINT('Ctrl Pts',(5.9601831227946,-11.9784445497445,24.2017910192575));
#61528=CARTESIAN_POINT('Ctrl Pts',(6.31919194555327,-11.8674827026873,24.2580454484966));
#61529=CARTESIAN_POINT('Ctrl Pts',(6.39474133018431,-11.8437059948412,24.270112962504));
#61530=CARTESIAN_POINT('',(-5.98852245733355,-11.3308498383553,25.041039515272));
#61531=CARTESIAN_POINT('Ctrl Pts',(-5.98852261948756,-11.3308502493362,
25.0410393033413));
#61532=CARTESIAN_POINT('Ctrl Pts',(-5.87203729212264,-11.3676893585621,
25.0233524151582));
#61533=CARTESIAN_POINT('Ctrl Pts',(-5.74885694585024,-11.4056370269848,
25.0052380517102));
#61534=CARTESIAN_POINT('Ctrl Pts',(-5.61897930285015,-11.4443295356622,
24.9868774560996));
#61535=CARTESIAN_POINT('Ctrl Pts',(-5.51139836494418,-11.4763795196109,
24.9716689101892));
#61536=CARTESIAN_POINT('Ctrl Pts',(-5.39922222271884,-11.5089397853205,
24.95629165793));
#61537=CARTESIAN_POINT('Ctrl Pts',(-5.28245262905368,-11.5417771151824,
24.9408537610589));
#61538=CARTESIAN_POINT('Ctrl Pts',(-5.21028892635494,-11.5620706114189,
24.9313131283897));
#61539=CARTESIAN_POINT('Ctrl Pts',(-5.13637046322292,-11.5824668107469,
24.9217505880393));
#61540=CARTESIAN_POINT('Ctrl Pts',(-5.06069736322921,-11.6028989291272,
24.9121955101112));
#61541=CARTESIAN_POINT('Ctrl Pts',(-5.00123303445601,-11.618954597588,24.9046870785098));
#61542=CARTESIAN_POINT('Ctrl Pts',(-4.94068526356721,-11.6350323657382,
24.8971832504966));
#61543=CARTESIAN_POINT('Ctrl Pts',(-4.87905391860342,-11.6510985731773,
24.8896996784921));
#61544=CARTESIAN_POINT('Ctrl Pts',(-4.80902284567548,-11.6693544419322,
24.8811961714355));
#61545=CARTESIAN_POINT('Ctrl Pts',(-4.73759279368948,-11.6875951379917,
24.8727189371375));
#61546=CARTESIAN_POINT('Ctrl Pts',(-4.66476376183948,-11.7057675159946,
24.8642922961047));
#61547=CARTESIAN_POINT('Ctrl Pts',(-4.62834924591448,-11.7148537049961,
24.8600789755884));
#61548=CARTESIAN_POINT('Ctrl Pts',(-4.59158498506663,-11.7239228122847,
24.8558782984125));
#61549=CARTESIAN_POINT('Ctrl Pts',(-4.55447097936004,-11.7329678424902,
24.8516934278991));
#61550=CARTESIAN_POINT('Ctrl Pts',(-4.53591397650673,-11.737490357593,24.8496009926424));
#61551=CARTESIAN_POINT('Ctrl Pts',(-4.51726953744016,-11.74200685328,24.8475125087285));
#61552=CARTESIAN_POINT('Ctrl Pts',(-4.49853766217382,-11.7465164463142,
24.8454283731866));
#61553=CARTESIAN_POINT('Ctrl Pts',(-4.48917172454064,-11.7487712428313,
24.8443863054157));
#61554=CARTESIAN_POINT('Ctrl Pts',(-4.47978392785757,-11.7510243136755,
24.8433453247165));
#61555=CARTESIAN_POINT('Ctrl Pts',(-4.47037427212638,-11.7532755472464,
24.842305481108));
#61556=CARTESIAN_POINT('Ctrl Pts',(-4.46096461639519,-11.7555267808173,
24.8412656374995));
#61557=CARTESIAN_POINT('Ctrl Pts',(-4.45028767571464,-11.7580722650254,
24.8400902439203));
#61558=CARTESIAN_POINT('Ctrl Pts',(-4.44207972779027,-11.7600236241699,
24.839189411637));
#61559=CARTESIAN_POINT('Ctrl Pts',(-4.3082138427399,-11.7918489258584,24.8244974676823));
#61560=CARTESIAN_POINT('Ctrl Pts',(-4.17003358662756,-11.8233757417418,
24.8100018159802));
#61561=CARTESIAN_POINT('Ctrl Pts',(-4.02753109711927,-11.8542860450678,
24.7958403638104));
#61562=CARTESIAN_POINT('Ctrl Pts',(-3.89043362431304,-11.8840239428708,
24.782216045313));
#61563=CARTESIAN_POINT('Ctrl Pts',(-3.74933536252293,-11.9131909388871,
24.768901016943));
#61564=CARTESIAN_POINT('Ctrl Pts',(-3.60424405611465,-11.9414881581407,
24.7560277004985));
#61565=CARTESIAN_POINT('Ctrl Pts',(-3.45629266440207,-11.9703431810486,
24.7429006212057));
#61566=CARTESIAN_POINT('Ctrl Pts',(-3.30418521703504,-11.9982928718332,
24.7302333253027));
#61567=CARTESIAN_POINT('Ctrl Pts',(-3.14792171413729,-12.0250014601485,
24.7181717967167));
#61568=CARTESIAN_POINT('Ctrl Pts',(-3.06978996268842,-12.0383557543061,
24.7121410324237));
#61569=CARTESIAN_POINT('Ctrl Pts',(-2.99061919724623,-12.0513995223159,
24.706261772375));
#61570=CARTESIAN_POINT('Ctrl Pts',(-2.91040941695071,-12.0640894680238,
24.7005525165982));
#61571=CARTESIAN_POINT('Ctrl Pts',(-2.8944008951393,-12.0666221675512,24.6994130452607));
#61572=CARTESIAN_POINT('Ctrl Pts',(-2.87835098870976,-12.0691407759745,
24.698280343509));
#61573=CARTESIAN_POINT('Ctrl Pts',(-2.86225969246319,-12.0716449382825,
24.6971545622365));
#61574=CARTESIAN_POINT('Ctrl Pts',(-2.83803873028227,-12.0754142567779,
24.6954600122631));
#61575=CARTESIAN_POINT('Ctrl Pts',(-2.81372399115987,-12.0791508453967,
24.6937811417577));
#61576=CARTESIAN_POINT('Ctrl Pts',(-2.7893154852027,-12.0828535279687,24.6921184602829));
#61577=CARTESIAN_POINT('Ctrl Pts',(-2.76900328635972,-12.0859348154834,
24.6907348148935));
#61578=CARTESIAN_POINT('Ctrl Pts',(-2.74862614907856,-12.0889926192221,
24.6893623822283));
#61579=CARTESIAN_POINT('Ctrl Pts',(-2.72818407336812,-12.0920262541816,
24.6880014584464));
#61580=CARTESIAN_POINT('Ctrl Pts',(-2.7179630355129,-12.0935430716613,24.6873209965555));
#61581=CARTESIAN_POINT('Ctrl Pts',(-2.70772576305032,-12.0950538469408,
24.686643411874));
#61582=CARTESIAN_POINT('Ctrl Pts',(-2.69747225598158,-12.0965584941556,
24.6859687414516));
#61583=CARTESIAN_POINT('Ctrl Pts',(-2.68721874891285,-12.0980631413704,
24.6852940710292));
#61584=CARTESIAN_POINT('Ctrl Pts',(-2.6755394896848,-12.0997661554961,24.6845306665604));
#61585=CARTESIAN_POINT('Ctrl Pts',(-2.66666303095805,-12.1010539656649,
24.6839535099897));
#61586=CARTESIAN_POINT('Ctrl Pts',(-2.48101466815436,-12.1279881132578,
24.6718824605159));
#61587=CARTESIAN_POINT('Ctrl Pts',(-2.29046761447812,-12.152891870862,24.6607744723008));
#61588=CARTESIAN_POINT('Ctrl Pts',(-2.09501603487607,-12.1752942100462,
24.6508269772436));
#61589=CARTESIAN_POINT('Ctrl Pts',(-1.9914217661717,-12.187168015056,24.6455545538742));
#61590=CARTESIAN_POINT('Ctrl Pts',(-1.88645003482912,-12.198338371781,24.6406083864231));
#61591=CARTESIAN_POINT('Ctrl Pts',(-1.78010252029589,-12.2087299989047,
24.6360195566438));
#61592=CARTESIAN_POINT('Ctrl Pts',(-1.69952665156399,-12.2166033788018,
24.6325427575146));
#61593=CARTESIAN_POINT('Ctrl Pts',(-1.61816109532668,-12.224030864184,24.6292705220193));
#61594=CARTESIAN_POINT('Ctrl Pts',(-1.53600439826816,-12.2309813192398,
24.6262153348566));
#61595=CARTESIAN_POINT('Ctrl Pts',(-1.46165279623633,-12.2372714634003,
24.6234503982393));
#61596=CARTESIAN_POINT('Ctrl Pts',(-1.38665322243647,-12.2431708891406,
24.6208632424687));
#61597=CARTESIAN_POINT('Ctrl Pts',(-1.31100694342468,-12.2486562098158,
24.6184622894281));
#61598=CARTESIAN_POINT('Ctrl Pts',(-1.23139016223158,-12.2544294425732,
24.61593531579));
#61599=CARTESIAN_POINT('Ctrl Pts',(-1.15105628669057,-12.2597439305082,
24.6136146255172));
#61600=CARTESIAN_POINT('Ctrl Pts',(-1.07000531525417,-12.2645727179209,
24.6115095904989));
#61601=CARTESIAN_POINT('Ctrl Pts',(-1.02947982953596,-12.2669871116273,
24.6104570729898));
#61602=CARTESIAN_POINT('Ctrl Pts',(-0.988775069842594,-12.2692800782001,
24.6094584653373));
#61603=CARTESIAN_POINT('Ctrl Pts',(-0.947891036077653,-12.2714482656201,
24.6085148998782));
#61604=CARTESIAN_POINT('Ctrl Pts',(-0.927449019195181,-12.2725323593301,
24.6080431171487));
#61605=CARTESIAN_POINT('Ctrl Pts',(-0.906962183795259,-12.273585258121,
24.6075850947084));
#61606=CARTESIAN_POINT('Ctrl Pts',(-0.886430529875502,-12.2746065445393,
24.6071409713632));
#61607=CARTESIAN_POINT('Ctrl Pts',(-0.876164702915622,-12.2751171877484,
24.6069189096906));
#61608=CARTESIAN_POINT('Ctrl Pts',(-0.865887671325822,-12.2756199278561,
24.6067003227752));
#61609=CARTESIAN_POINT('Ctrl Pts',(-0.855599435106474,-12.2761147128055,
24.6064852277811));
#61610=CARTESIAN_POINT('Ctrl Pts',(-0.845311198887126,-12.2766094977549,
24.6062701327869));
#61611=CARTESIAN_POINT('Ctrl Pts',(-0.833325131026369,-12.277174653871,
24.6060244894571));
#61612=CARTESIAN_POINT('Ctrl Pts',(-0.824701112560467,-12.2775751501454,
24.6058504356311));
#61613=CARTESIAN_POINT('Ctrl Pts',(-0.603040005567242,-12.2878690111678,
24.6013767713046));
#61614=CARTESIAN_POINT('Ctrl Pts',(-0.379291206361343,-12.2940987664784,
24.5986974694608));
#61615=CARTESIAN_POINT('Ctrl Pts',(-0.153450032143192,-12.2960189027172,
24.5978640448336));
#61616=CARTESIAN_POINT('Ctrl Pts',(-0.0981184220889285,-12.296489340537,
24.5976598538723));
#61617=CARTESIAN_POINT('Ctrl Pts',(-0.0426612493675976,-12.2967008729678,
24.5975665207692));
#61618=CARTESIAN_POINT('Ctrl Pts',(0.0129209291749937,-12.2966522430943,
24.5975851009201));
#61619=CARTESIAN_POINT('Ctrl Pts',(0.154143964989606,-12.2965286844546,
24.5976323093129));
#61620=CARTESIAN_POINT('Ctrl Pts',(0.296176681680763,-12.2947211521966,
24.5984041962327));
#61621=CARTESIAN_POINT('Ctrl Pts',(0.439019093386752,-12.2911972488102,
24.5999241571628));
#61622=CARTESIAN_POINT('Ctrl Pts',(0.510440299239747,-12.289435297117,24.6006841376278));
#61623=CARTESIAN_POINT('Ctrl Pts',(0.582063928371205,-12.2872442541996,
24.6016311402581));
#61624=CARTESIAN_POINT('Ctrl Pts',(0.653889980745084,-12.284621348819,24.6027674927322));
#61625=CARTESIAN_POINT('Ctrl Pts',(0.689803006932021,-12.2833098961286,
24.6033356689693));
#61626=CARTESIAN_POINT('Ctrl Pts',(0.72576663891555,-12.2818904780535,24.6039511831153));
#61627=CARTESIAN_POINT('Ctrl Pts',(0.761780876621343,-12.2803627883741,
24.6046143100682));
#61628=CARTESIAN_POINT('Ctrl Pts',(0.77978799547424,-12.2795989435345,24.6049458735447));
#61629=CARTESIAN_POINT('Ctrl Pts',(0.797807765757056,-12.2788080308129,
24.6052893402592));
#61630=CARTESIAN_POINT('Ctrl Pts',(0.815840187458312,-12.2779900166903,
24.6056447425024));
#61631=CARTESIAN_POINT('Ctrl Pts',(0.833872609159567,-12.2771720025676,
24.6060001447456));
#61632=CARTESIAN_POINT('Ctrl Pts',(0.853533015103848,-12.2762488605904,
24.6064014130275));
#61633=CARTESIAN_POINT('Ctrl Pts',(0.869975406804535,-12.2754546381132,
24.6067467875715));
#61634=CARTESIAN_POINT('Ctrl Pts',(0.954838144713319,-12.2713554842222,
24.6085293402528));
#61635=CARTESIAN_POINT('Ctrl Pts',(1.03908076610755,-12.2666952328111,24.6105599527878));
#61636=CARTESIAN_POINT('Ctrl Pts',(1.12269744174171,-12.2615009244909,24.6128288068564));
#61637=CARTESIAN_POINT('Ctrl Pts',(1.34022666710179,-12.2479879038332,24.6187312427553));
#61638=CARTESIAN_POINT('Ctrl Pts',(1.55351828284116,-12.2308639657858,24.6262450190716));
#61639=CARTESIAN_POINT('Ctrl Pts',(1.76257209799047,-12.2106134075563,24.6351868042739));
#61640=CARTESIAN_POINT('Ctrl Pts',(1.93920899338593,-12.193503001161,24.6427420319854));
#61641=CARTESIAN_POINT('Ctrl Pts',(2.1128209108483,-12.1741595331882,24.6513170009043));
#61642=CARTESIAN_POINT('Ctrl Pts',(2.28341906446789,-12.1528496006427,24.6608086010793));
#61643=CARTESIAN_POINT('Ctrl Pts',(2.31450099185576,-12.1489670628663,24.6625379118671));
#61644=CARTESIAN_POINT('Ctrl Pts',(2.34548290429981,-12.1450191894154,24.6642976673795));
#61645=CARTESIAN_POINT('Ctrl Pts',(2.37636489708942,-12.1410075682698,24.6660872274319));
#61646=CARTESIAN_POINT('Ctrl Pts',(2.47701179056917,-12.1279333729328,24.6719195472952));
#61647=CARTESIAN_POINT('Ctrl Pts',(2.57747204661453,-12.1140718251945,24.6781174316816));
#61648=CARTESIAN_POINT('Ctrl Pts',(2.67697489282744,-12.0995577541734,24.6846234144293));
#61649=CARTESIAN_POINT('Ctrl Pts',(2.77861440864647,-12.0847320159428,24.6912691030861));
#61650=CARTESIAN_POINT('Ctrl Pts',(2.8792548073093,-12.0692255340046,24.6982362519364));
#61651=CARTESIAN_POINT('Ctrl Pts',(2.9780848394563,-12.0532304524573,24.7054405178432));
#61652=CARTESIAN_POINT('Ctrl Pts',(3.0123039965395,-12.0476922754868,24.707934940858));
#61653=CARTESIAN_POINT('Ctrl Pts',(3.04630621857371,-12.0420959332209,24.7104575923126));
#61654=CARTESIAN_POINT('Ctrl Pts',(3.08005815461792,-12.0364506606366,24.7130043583632));
#61655=CARTESIAN_POINT('Ctrl Pts',(3.15872540585718,-12.0232929538869,24.7189402277749));
#61656=CARTESIAN_POINT('Ctrl Pts',(3.23624816580929,-12.0098356819973,24.7250222887154));
#61657=CARTESIAN_POINT('Ctrl Pts',(3.31262495126853,-11.9961231064857,24.7312311044611));
#61658=CARTESIAN_POINT('Ctrl Pts',(3.45631259761645,-11.9703256382004,24.7429117495125));
#61659=CARTESIAN_POINT('Ctrl Pts',(3.59594394370824,-11.9436260683294,24.7550405618913));
#61660=CARTESIAN_POINT('Ctrl Pts',(3.73152323809938,-11.9163084789191,24.7674937459439));
#61661=CARTESIAN_POINT('Ctrl Pts',(3.83534629158847,-11.895389388292,24.7770300663666));
#61662=CARTESIAN_POINT('Ctrl Pts',(3.93679211525432,-11.8741075813535,24.7867566625271));
#61663=CARTESIAN_POINT('Ctrl Pts',(4.03586070844626,-11.8525830145618,24.7966201217043));
#61664=CARTESIAN_POINT('Ctrl Pts',(4.06062785674425,-11.8472018728639,24.7990859864985));
#61665=CARTESIAN_POINT('Ctrl Pts',(4.08626076073108,-11.8415877062263,24.8016601504212));
#61666=CARTESIAN_POINT('Ctrl Pts',(4.11422298318758,-11.835398101637,24.8045003838752));
#61667=CARTESIAN_POINT('Ctrl Pts',(4.14218520564409,-11.8292084970477,24.8073406173293));
#61668=CARTESIAN_POINT('Ctrl Pts',(4.16996881025387,-11.8229965347247,24.8101932086679));
#61669=CARTESIAN_POINT('Ctrl Pts',(4.1975737970365,-11.8167648448493,24.8130569697881));
#61670=CARTESIAN_POINT('Ctrl Pts',(4.20543951623015,-11.8149891974618,24.8138729651366));
#61671=CARTESIAN_POINT('Ctrl Pts',(4.21329073408853,-11.8132119477631,24.8146898676183));
#61672=CARTESIAN_POINT('Ctrl Pts',(4.22112745001383,-11.8114331549952,24.8155076504106));
#61673=CARTESIAN_POINT('Ctrl Pts',(4.26829713190448,-11.8007264903911,24.8204299360386));
#61674=CARTESIAN_POINT('Ctrl Pts',(4.3149414118535,-11.7899639527628,24.8253841062339));
#61675=CARTESIAN_POINT('Ctrl Pts',(4.36106030408131,-11.77915846756,24.8303645098757));
#61676=CARTESIAN_POINT('Ctrl Pts',(4.5190215100943,-11.742148743524,24.8474228243255));
#61677=CARTESIAN_POINT('Ctrl Pts',(4.67082010192686,-11.7046406077475,24.8647871087404));
#61678=CARTESIAN_POINT('Ctrl Pts',(4.81645382359858,-11.6671135529552,24.8822424723097));
#61679=CARTESIAN_POINT('Ctrl Pts',(4.86915567872832,-11.6535332819685,24.8885592101608));
#61680=CARTESIAN_POINT('Ctrl Pts',(4.9210503274101,-11.6399500662591,24.8948880037593));
#61681=CARTESIAN_POINT('Ctrl Pts',(4.97213805285758,-11.6263850694136,24.9012191073043));
#61682=CARTESIAN_POINT('Ctrl Pts',(5.00446500995171,-11.6178014993453,24.9052252616372));
#61683=CARTESIAN_POINT('Ctrl Pts',(5.03646882664084,-11.6092260567639,24.9092319631941));
#61684=CARTESIAN_POINT('Ctrl Pts',(5.06814946717143,-11.6006633548531,24.9132370544178));
#61685=CARTESIAN_POINT('Ctrl Pts',(5.21038741293057,-11.562219020725,24.9312188861827));
#61686=CARTESIAN_POINT('Ctrl Pts',(5.34611056112384,-11.5240356189547,24.9491675989117));
#61687=CARTESIAN_POINT('Ctrl Pts',(5.47531845837768,-11.4865046012324,24.9669050009867));
#61688=CARTESIAN_POINT('Ctrl Pts',(5.60704277519038,-11.4482426391245,24.984987852113));
#61689=CARTESIAN_POINT('Ctrl Pts',(5.73199578464032,-11.4106585980952,25.0028509325174));
#61690=CARTESIAN_POINT('Ctrl Pts',(5.85017903341744,-11.3741144711569,25.0203156695206));
#61691=CARTESIAN_POINT('Ctrl Pts',(5.86231997951077,-11.3703602988882,25.0221098191373));
#61692=CARTESIAN_POINT('Ctrl Pts',(5.87438948168156,-11.3666170571579,25.0238997747802));
#61693=CARTESIAN_POINT('Ctrl Pts',(5.88638754150042,-11.3628851084615,25.0256853498019));
#61694=CARTESIAN_POINT('Ctrl Pts',(5.9210293540039,-11.3521099107238,25.0308408129391));
#61695=CARTESIAN_POINT('Ctrl Pts',(5.95507558688705,-11.3414288775921,25.0359597592798));
#61696=CARTESIAN_POINT('Ctrl Pts',(5.98852582557976,-11.3308501354331,25.0410382779965));
#61697=CARTESIAN_POINT('',(-6.27159361731041,-11.8794975616087,24.2690120888651));
#61698=CARTESIAN_POINT('Origin',(-5.9999949808,-10.9277770011797,24.1259380084106));
#61699=CARTESIAN_POINT('Ctrl Pts',(-6.27159386307184,-11.8794985003198,
24.2690123724987));
#61700=CARTESIAN_POINT('Ctrl Pts',(-6.19708064714059,-11.9025009409338,
24.2574475533713));
#61701=CARTESIAN_POINT('Ctrl Pts',(-6.11543894003613,-11.9272858575891,
24.2450493547133));
#61702=CARTESIAN_POINT('Ctrl Pts',(-6.02658470930716,-11.9536191428594,
24.2319368725984));
#61703=CARTESIAN_POINT('Ctrl Pts',(-5.93855995222029,-11.9797066011628,
24.2189467983666));
#61704=CARTESIAN_POINT('Ctrl Pts',(-5.84345655035932,-12.0073137872402,
24.2052557335694));
#61705=CARTESIAN_POINT('Ctrl Pts',(-5.7411838234057,-12.0361672792979,24.1909996691092));
#61706=CARTESIAN_POINT('Ctrl Pts',(-5.64049533840775,-12.0645738202079,
24.1769644363028));
#61707=CARTESIAN_POINT('Ctrl Pts',(-5.53285775062703,-12.0941884570633,
24.1623816092192));
#61708=CARTESIAN_POINT('Ctrl Pts',(-5.41817817581817,-12.1247040018455,
24.1474001817781));
#61709=CARTESIAN_POINT('Ctrl Pts',(-5.37925167383706,-12.1350621097858,
24.1423149295356));
#61710=CARTESIAN_POINT('Ctrl Pts',(-5.33951376816848,-12.1455236128537,
24.1371839145072));
#61711=CARTESIAN_POINT('Ctrl Pts',(-5.2989607104461,-12.1560752216459,24.1320134677298));
#61712=CARTESIAN_POINT('Ctrl Pts',(-5.21821245862246,-12.1770853257353,
24.1217182011858));
#61713=CARTESIAN_POINT('Ctrl Pts',(-5.13423231221224,-12.1984533510321,
24.1112662369327));
#61714=CARTESIAN_POINT('Ctrl Pts',(-5.0469909259153,-12.2200666319346,24.1007138157334));
#61715=CARTESIAN_POINT('Ctrl Pts',(-4.92201084106593,-12.2510293412144,
24.085596649984));
#61716=CARTESIAN_POINT('Ctrl Pts',(-4.79033765404794,-12.2824975295437,
24.0702722548015));
#61717=CARTESIAN_POINT('Ctrl Pts',(-4.65188544733252,-12.3141001739185,
24.0549257642203));
#61718=CARTESIAN_POINT('Ctrl Pts',(-4.5134332406171,-12.3457028182933,24.039579273639));
#61719=CARTESIAN_POINT('Ctrl Pts',(-4.36820181664654,-12.3774401803882,
24.0242105653309));
#61720=CARTESIAN_POINT('Ctrl Pts',(-4.21610826590916,-12.4088909807736,
24.0090296785428));
#61721=CARTESIAN_POINT('Ctrl Pts',(-4.07082504414953,-12.4389335012141,
23.9945285499213));
#61722=CARTESIAN_POINT('Ctrl Pts',(-3.91927991557136,-12.4687142331352,
23.9801988310894));
#61723=CARTESIAN_POINT('Ctrl Pts',(-3.76141769099652,-12.4978253761718,
23.966247356158));
#61724=CARTESIAN_POINT('Ctrl Pts',(-3.73054470085429,-12.5035186193426,
23.9635188772633));
#61725=CARTESIAN_POINT('Ctrl Pts',(-3.69943013468555,-12.5091861150751,
23.9608049377641));
#61726=CARTESIAN_POINT('Ctrl Pts',(-3.66807363502218,-12.514824609958,23.9581071920514));
#61727=CARTESIAN_POINT('Ctrl Pts',(-3.58017498710756,-12.5306304582447,
23.9505448619729));
#61728=CARTESIAN_POINT('Ctrl Pts',(-3.49037513941867,-12.5462087327828,
23.9431096159783));
#61729=CARTESIAN_POINT('Ctrl Pts',(-3.39866711822361,-12.5614848718521,
23.9358394498037));
#61730=CARTESIAN_POINT('Ctrl Pts',(-3.35281310762608,-12.5691229413868,
23.9322043667164));
#61731=CARTESIAN_POINT('Ctrl Pts',(-3.30648204469947,-12.5766854194222,
23.9286105469247));
#61732=CARTESIAN_POINT('Ctrl Pts',(-3.25967322796412,-12.5841625638991,
23.9250630077419));
#61733=CARTESIAN_POINT('Ctrl Pts',(-3.23626881959645,-12.5879011361376,
23.9232892381504));
#61734=CARTESIAN_POINT('Ctrl Pts',(-3.21274497218075,-12.5916183713035,
23.9215270382812));
#61735=CARTESIAN_POINT('Ctrl Pts',(-3.18910160199944,-12.595313027064,23.9197770418822));
#61736=CARTESIAN_POINT('Ctrl Pts',(-3.17727991690878,-12.5971603549442,
23.9189020436828));
#61737=CARTESIAN_POINT('Ctrl Pts',(-3.16542835109203,-12.5990020377369,
23.918030096324));
#61738=CARTESIAN_POINT('Ctrl Pts',(-3.15354689471706,-12.6008379184752,
23.9171612799832));
#61739=CARTESIAN_POINT('Ctrl Pts',(-3.1416654383421,-12.6026737992134,23.9162924636424));
#61740=CARTESIAN_POINT('Ctrl Pts',(-3.1281400511785,-12.6047504351401,23.9153102018295));
#61741=CARTESIAN_POINT('Ctrl Pts',(-3.11781284420954,-12.6063279965277,
23.9145643044261));
#61742=CARTESIAN_POINT('Ctrl Pts',(-3.07661938484431,-12.6126206186387,
23.9115890474692));
#61743=CARTESIAN_POINT('Ctrl Pts',(-3.03568519935775,-12.6187487292425,
23.9086931412116));
#61744=CARTESIAN_POINT('Ctrl Pts',(-2.99501202309511,-12.6247166820769,
23.9058744407652));
#61745=CARTESIAN_POINT('Ctrl Pts',(-2.79739625318866,-12.6537127355573,
23.8921794282279));
#61746=CARTESIAN_POINT('Ctrl Pts',(-2.60594586740788,-12.6789296984963,
23.8803064010344));
#61747=CARTESIAN_POINT('Ctrl Pts',(-2.42085391603547,-12.7008778071539,
23.870005028324));
#61748=CARTESIAN_POINT('Ctrl Pts',(-2.23092606413269,-12.723399354416,23.8594345114753));
#61749=CARTESIAN_POINT('Ctrl Pts',(-2.04769292395376,-12.7424793193334,
23.8505186523863));
#61750=CARTESIAN_POINT('Ctrl Pts',(-1.87131426315632,-12.7586451232207,
23.8429958321136));
#61751=CARTESIAN_POINT('Ctrl Pts',(-1.78116939726151,-12.7669072577495,
23.8391510153905));
#61752=CARTESIAN_POINT('Ctrl Pts',(-1.69281424560786,-12.7744077750593,
23.8356702336904));
#61753=CARTESIAN_POINT('Ctrl Pts',(-1.60626582519892,-12.7812143692985,
23.8325196677634));
#61754=CARTESIAN_POINT('Ctrl Pts',(-1.43907203963571,-12.7943633124251,
23.8264334209953));
#61755=CARTESIAN_POINT('Ctrl Pts',(-1.27862277410174,-12.8049251375061,
23.8215784341343));
#61756=CARTESIAN_POINT('Ctrl Pts',(-1.1250175870215,-12.8133803812603,23.8177150430602));
#61757=CARTESIAN_POINT('Ctrl Pts',(-0.969940669440592,-12.8219166368629,
23.8138146358503));
#61758=CARTESIAN_POINT('Ctrl Pts',(-0.821839215358774,-12.8283058798147,
23.8109248045128));
#61759=CARTESIAN_POINT('Ctrl Pts',(-0.680783296076854,-12.8330036704535,
23.8088159024075));
#61760=CARTESIAN_POINT('Ctrl Pts',(-0.53838902393423,-12.837746034206,23.8066869908252));
#61761=CARTESIAN_POINT('Ctrl Pts',(-0.403174234552946,-12.8407648333977,
23.8053537869326));
#61762=CARTESIAN_POINT('Ctrl Pts',(-0.275184076784705,-12.8424872179352,
23.8045989542072));
#61763=CARTESIAN_POINT('Ctrl Pts',(-0.236233659390891,-12.8430113800881,
23.804369240843));
#61764=CARTESIAN_POINT('Ctrl Pts',(-0.197952170246763,-12.8434151814382,
23.8041932297371));
#61765=CARTESIAN_POINT('Ctrl Pts',(-0.160340475176224,-12.8437098785878,
23.8040651618987));
#61766=CARTESIAN_POINT('Ctrl Pts',(-0.154018237855442,-12.8437594149172,
23.8040436346779));
#61767=CARTESIAN_POINT('Ctrl Pts',(-0.147714925196181,-12.8438058676637,
23.8040234624916));
#61768=CARTESIAN_POINT('Ctrl Pts',(-0.141430540525102,-12.8438492902627,
23.8040046172673));
#61769=CARTESIAN_POINT('Ctrl Pts',(-0.103048091275479,-12.8441144977235,
23.8038895183507));
#61770=CARTESIAN_POINT('Ctrl Pts',(-0.0662562838150946,-12.8442643991019,
23.8038251218336));
#61771=CARTESIAN_POINT('Ctrl Pts',(-0.0289819554348571,-12.844317014175,
23.8038019501873));
#61772=CARTESIAN_POINT('Ctrl Pts',(-0.0185596180577554,-12.8443317259637,
23.8037954711245));
#61773=CARTESIAN_POINT('Ctrl Pts',(-0.00809955461635552,-12.844338555091,
23.8037923587938));
#61774=CARTESIAN_POINT('Ctrl Pts',(0.00244355647455851,-12.844337252009,
23.803792740049));
#61775=CARTESIAN_POINT('Ctrl Pts',(0.127128013150683,-12.8443218415601,
23.8037972488312));
#61776=CARTESIAN_POINT('Ctrl Pts',(0.258986464546909,-12.8431696756197,
23.8042924754873));
#61777=CARTESIAN_POINT('Ctrl Pts',(0.397985692314567,-12.8404650149112,
23.8054910559536));
#61778=CARTESIAN_POINT('Ctrl Pts',(0.535666794351003,-12.8377860024234,
23.8066782703155));
#61779=CARTESIAN_POINT('Ctrl Pts',(0.680354207936333,-12.833583687344,23.8085556447809));
#61780=CARTESIAN_POINT('Ctrl Pts',(0.831993697184611,-12.8274126453801,
23.8113495723966));
#61781=CARTESIAN_POINT('Ctrl Pts',(0.94225644354008,-12.8229254498733,23.8133811417033));
#61782=CARTESIAN_POINT('Ctrl Pts',(1.05619452308235,-12.8173964738687,23.8158977309064));
#61783=CARTESIAN_POINT('Ctrl Pts',(1.17377814699504,-12.8106410003335,23.8189926615624));
#61784=CARTESIAN_POINT('Ctrl Pts',(1.33433786019959,-12.8014164428886,23.8232187702838));
#61785=CARTESIAN_POINT('Ctrl Pts',(1.50169675089625,-12.7899057935866,23.8285229658335));
#61786=CARTESIAN_POINT('Ctrl Pts',(1.6757438097164,-12.7756233796364,23.8351480557093));
#61787=CARTESIAN_POINT('Ctrl Pts',(1.84376169748946,-12.7618357233527,23.8415436455848));
#61788=CARTESIAN_POINT('Ctrl Pts',(2.01801263886451,-12.7454647212648,23.8491703749819));
#61789=CARTESIAN_POINT('Ctrl Pts',(2.19836007197658,-12.7260475718018,23.8582571266038));
#61790=CARTESIAN_POINT('Ctrl Pts',(2.26107777821509,-12.7192950549792,23.8614171395247));
#61791=CARTESIAN_POINT('Ctrl Pts',(2.32453242794122,-12.7121739290865,23.8647538068919));
#61792=CARTESIAN_POINT('Ctrl Pts',(2.38871710222971,-12.7046640542677,23.8682770054759));
#61793=CARTESIAN_POINT('Ctrl Pts',(2.47498633891838,-12.6945701934602,23.8730124607214));
#61794=CARTESIAN_POINT('Ctrl Pts',(2.5625744551735,-12.6837740476544,23.8780848912508));
#61795=CARTESIAN_POINT('Ctrl Pts',(2.65146478041537,-12.6722277327554,23.8835179409207));
#61796=CARTESIAN_POINT('Ctrl Pts',(2.72897733062453,-12.6621593219255,23.8882555716379));
#61797=CARTESIAN_POINT('Ctrl Pts',(2.80748007424341,-12.6515204683365,23.8932674718265));
#61798=CARTESIAN_POINT('Ctrl Pts',(2.88696072282057,-12.6402790211584,23.8985693908055));
#61799=CARTESIAN_POINT('Ctrl Pts',(2.92670104710914,-12.6346582975693,23.9012203502951));
#61800=CARTESIAN_POINT('Ctrl Pts',(2.96668584644875,-12.6288869179267,23.9039438136002));
#61801=CARTESIAN_POINT('Ctrl Pts',(3.00691346377708,-12.6229608302188,23.9067417754196));
#61802=CARTESIAN_POINT('Ctrl Pts',(3.02702727244124,-12.6199977863648,23.9081407563294));
#61803=CARTESIAN_POINT('Ctrl Pts',(3.04720178554791,-12.6169960650334,23.9095583618172));
#61804=CARTESIAN_POINT('Ctrl Pts',(3.06743679137486,-12.6139551575869,23.9109948405961));
#61805=CARTESIAN_POINT('Ctrl Pts',(3.07755429428834,-12.6124347038637,23.9117130799855));
#61806=CARTESIAN_POINT('Ctrl Pts',(3.08768692037775,-12.6109044535828,23.9124360376945));
#61807=CARTESIAN_POINT('Ctrl Pts',(3.09783464270007,-12.6093643430508,23.9131637448486));
#61808=CARTESIAN_POINT('Ctrl Pts',(3.10798236502239,-12.6078242325187,23.9138914520027));
#61809=CARTESIAN_POINT('Ctrl Pts',(3.11649244848053,-12.6065275650744,23.9145041924201));
#61810=CARTESIAN_POINT('Ctrl Pts',(3.12832307126662,-12.6047143669116,23.915361145775));
#61811=CARTESIAN_POINT('Ctrl Pts',(3.24396552605183,-12.5869906434566,23.9237377284268));
#61812=CARTESIAN_POINT('Ctrl Pts',(3.35681651989267,-12.5687093250851,23.9324152959104));
#61813=CARTESIAN_POINT('Ctrl Pts',(3.46688415179261,-12.5500070581239,23.9413237929068));
#61814=CARTESIAN_POINT('Ctrl Pts',(3.63912326404861,-12.5207408533099,23.9552642365022));
#61815=CARTESIAN_POINT('Ctrl Pts',(3.80454615891661,-12.4904466297004,23.9697687507377));
#61816=CARTESIAN_POINT('Ctrl Pts',(3.96320907665928,-12.4596127305724,23.9845897060615));
#61817=CARTESIAN_POINT('Ctrl Pts',(4.12187199440194,-12.4287788314444,23.9994106613853));
#61818=CARTESIAN_POINT('Ctrl Pts',(4.27377520622497,-12.3974049903084,24.0145481991502));
#61819=CARTESIAN_POINT('Ctrl Pts',(4.41898721777619,-12.3659267693461,24.0297822509075));
#61820=CARTESIAN_POINT('Ctrl Pts',(4.56351696175518,-12.3345964464066,24.0449447266334));
#61821=CARTESIAN_POINT('Ctrl Pts',(4.70141874662422,-12.3031625796294,24.0602030464379));
#61822=CARTESIAN_POINT('Ctrl Pts',(4.83277339477483,-12.2720089508995,24.0753670005252));
#61823=CARTESIAN_POINT('Ctrl Pts',(4.90532264871698,-12.254802308015,24.0837422926929));
#61824=CARTESIAN_POINT('Ctrl Pts',(4.975874747427,-12.2376802960697,24.0920892107805));
#61825=CARTESIAN_POINT('Ctrl Pts',(5.04444361185108,-12.2207014895619,24.1003786510992));
#61826=CARTESIAN_POINT('Ctrl Pts',(5.13538803840724,-12.198182116747,24.1113731221698));
#61827=CARTESIAN_POINT('Ctrl Pts',(5.22284371582237,-12.1759150854809,24.1222662743539));
#61828=CARTESIAN_POINT('Ctrl Pts',(5.3068432141015,-12.1540259495273,24.1329956083273));
#61829=CARTESIAN_POINT('Ctrl Pts',(5.42689803314422,-12.122741283431,24.1483303219271));
#61830=CARTESIAN_POINT('Ctrl Pts',(5.53989334717833,-12.0922305098064,24.1633297223276));
#61831=CARTESIAN_POINT('Ctrl Pts',(5.64592620334713,-12.0628176246999,24.1778361176492));
#61832=CARTESIAN_POINT('Ctrl Pts',(5.75378553571296,-12.0328980859346,24.192592393873));
#61833=CARTESIAN_POINT('Ctrl Pts',(5.85444062957484,-12.0041144877992,24.2068385125593));
#61834=CARTESIAN_POINT('Ctrl Pts',(5.94798628536258,-11.976758368691,24.2204298262157));
#61835=CARTESIAN_POINT('Ctrl Pts',(6.02496352185606,-11.9542474521508,24.2316139026625));
#61836=CARTESIAN_POINT('Ctrl Pts',(6.09712657776811,-11.9327021773434,24.2423549858525));
#61837=CARTESIAN_POINT('Ctrl Pts',(6.16452362202879,-11.9122612713575,24.2525831370081));
#61838=CARTESIAN_POINT('Ctrl Pts',(6.20165855736736,-11.9009985857253,24.2582187214163));
#61839=CARTESIAN_POINT('Ctrl Pts',(6.23734650792921,-11.8900707994031,24.2636987908079));
#61840=CARTESIAN_POINT('Ctrl Pts',(6.27159479316527,-11.8794983798055,24.2690136880117));
#61841=CARTESIAN_POINT('Ctrl Pts',(-6.390311350328,-11.8061935254293,24.5118466387929));
#61842=CARTESIAN_POINT('Ctrl Pts',(-4.260207566885,-12.4817978211448,24.1870549186574));
#61843=CARTESIAN_POINT('Ctrl Pts',(0.0001663377189254,-13.1582627349181,
23.8622596453287));
#61844=CARTESIAN_POINT('Ctrl Pts',(4.260540242323,-12.4817449966618,24.187080281601));
#61845=CARTESIAN_POINT('Ctrl Pts',(6.390810363485,-11.8060352474225,24.5119227297642));
#61846=CARTESIAN_POINT('Ctrl Pts',(-6.390311350328,-11.9720500990187,23.5458954363187));
#61847=CARTESIAN_POINT('Ctrl Pts',(-4.260207566885,-12.6077625183053,23.2652555130157));
#61848=CARTESIAN_POINT('Ctrl Pts',(0.0001663377189254,-13.2461470236974,
22.9846373688158));
#61849=CARTESIAN_POINT('Ctrl Pts',(4.260540242323,-12.6077126674846,23.2652774262116));
#61850=CARTESIAN_POINT('Ctrl Pts',(6.390810363485,-11.9719011667457,23.5459611835739));
#61851=CARTESIAN_POINT('Ctrl Pts',(-6.390311350328,-12.0713617692531,21.4528915452424));
#61852=CARTESIAN_POINT('Ctrl Pts',(-4.260207566885,-12.659242522167,21.2792390801719));
#61853=CARTESIAN_POINT('Ctrl Pts',(0.0001663377189254,-13.2456907932709,
21.1056336066131));
#61854=CARTESIAN_POINT('Ctrl Pts',(4.260540242323,-12.6591967269967,21.279252636856));
#61855=CARTESIAN_POINT('Ctrl Pts',(6.390810363485,-12.0712240427635,21.4529322278795));
#61856=CARTESIAN_POINT('Ctrl Pts',(-6.390311350328,-11.3879808552225,18.3168609136282));
#61857=CARTESIAN_POINT('Ctrl Pts',(-4.260207566885,-12.0191856806185,18.3050659001811));
#61858=CARTESIAN_POINT('Ctrl Pts',(0.0001663377189254,-12.6510858023129,
18.2929947474269));
#61859=CARTESIAN_POINT('Ctrl Pts',(4.260540242323,-12.0191363361555,18.3050668428024));
#61860=CARTESIAN_POINT('Ctrl Pts',(6.390810363485,-11.3878329789516,18.3168636769094));
#61861=CARTESIAN_POINT('Ctrl Pts',(-6.390311350328,-9.96973039617433,15.6641171406436));
#61862=CARTESIAN_POINT('Ctrl Pts',(-4.260207566885,-10.7489883683133,15.7526875000242));
#61863=CARTESIAN_POINT('Ctrl Pts',(0.0001663377189254,-11.5273045000232,
15.8421713762416));
#61864=CARTESIAN_POINT('Ctrl Pts',(4.260540242323,-10.748927590366,15.7526805123096));
#61865=CARTESIAN_POINT('Ctrl Pts',(6.390810363485,-9.9695478345618,15.6640963907245));
#61866=CARTESIAN_POINT('Ctrl Pts',(-6.390311350328,-8.71308977409159,14.2543209333947));
#61867=CARTESIAN_POINT('Ctrl Pts',(-4.260207566885,-9.62712791089626,14.3567599107344));
#61868=CARTESIAN_POINT('Ctrl Pts',(0.0001663377189254,-10.542551067134,
14.4578276726223));
#61869=CARTESIAN_POINT('Ctrl Pts',(4.260540242323,-9.62705642639862,14.3567520184532));
#61870=CARTESIAN_POINT('Ctrl Pts',(6.390810363485,-8.71287563671292,14.2542969343644));
#61871=CARTESIAN_POINT('Ctrl Pts',(-6.390311350328,-8.1393678365502,13.7249554217385));
#61872=CARTESIAN_POINT('Ctrl Pts',(-4.260207566885,-9.11425616282747,13.8221631313431));
#61873=CARTESIAN_POINT('Ctrl Pts',(0.0001663377189254,-10.0902570778465,
13.9182879348291));
#61874=CARTESIAN_POINT('Ctrl Pts',(4.260540242323,-9.11417994787105,13.8221556250518));
#61875=CARTESIAN_POINT('Ctrl Pts',(6.390810363485,-8.13913944341977,13.7249326482792));
#61876=CARTESIAN_POINT('',(-6.26386060047837,-8.42071136785102,13.944258352743));
#61877=CARTESIAN_POINT('Ctrl Pts',(-6.27159552384391,-11.8794980574192,
24.2690121660514));
#61878=CARTESIAN_POINT('Ctrl Pts',(-6.27195777356616,-11.915653437869,24.0278185457168));
#61879=CARTESIAN_POINT('Ctrl Pts',(-6.27229031321601,-11.9441024432717,
23.7878332652866));
#61880=CARTESIAN_POINT('Ctrl Pts',(-6.27259314303954,-11.9652318790949,
23.5495554059373));
#61881=CARTESIAN_POINT('Ctrl Pts',(-6.27289863569945,-11.9865471097967,
23.3091823270881));
#61882=CARTESIAN_POINT('Ctrl Pts',(-6.27317389374832,-12.0004135038023,
23.0705467396266));
#61883=CARTESIAN_POINT('Ctrl Pts',(-6.27341891743877,-12.0072245116416,
22.8341074875309));
#61884=CARTESIAN_POINT('Ctrl Pts',(-6.27366754257446,-12.0141356300935,
22.5941929673217));
#61885=CARTESIAN_POINT('Ctrl Pts',(-6.27388503802917,-12.0137824618086,
22.3565397769456));
#61886=CARTESIAN_POINT('Ctrl Pts',(-6.27407140406683,-12.0065719197372,
22.1215733736428));
#61887=CARTESIAN_POINT('Ctrl Pts',(-6.2742180445919,-12.0008983662902,21.9366920659419));
#61888=CARTESIAN_POINT('Ctrl Pts',(-6.27434541228839,-11.9909792002045,
21.7534731040869));
#61889=CARTESIAN_POINT('Ctrl Pts',(-6.27445350728488,-11.9770107165648,
21.5721011929025));
#61890=CARTESIAN_POINT('Ctrl Pts',(-6.274502629551,-11.9706629336613,21.4896792531497));
#61891=CARTESIAN_POINT('Ctrl Pts',(-6.27454777177045,-11.9634789140546,
21.4076384849629));
#61892=CARTESIAN_POINT('Ctrl Pts',(-6.27458893395529,-11.9554822034544,
21.3259945718025));
#61893=CARTESIAN_POINT('Ctrl Pts',(-6.274707125726,-11.9325207064088,21.0915648713221));
#61894=CARTESIAN_POINT('Ctrl Pts',(-6.27479250271421,-11.9028603482648,
20.8604109425169));
#61895=CARTESIAN_POINT('Ctrl Pts',(-6.27484506491992,-11.8670439537005,
20.6328687479079));
#61896=CARTESIAN_POINT('Ctrl Pts',(-6.27489762712562,-11.8312275591362,
20.4053265532988));
#61897=CARTESIAN_POINT('Ctrl Pts',(-6.27491737454883,-11.7892550892312,
20.1813959027504));
#61898=CARTESIAN_POINT('Ctrl Pts',(-6.27490430718954,-11.7416481920867,
19.9613626470728));
#61899=CARTESIAN_POINT('Ctrl Pts',(-6.27489476683278,-11.7068908418988,
19.8007184257666));
#61900=CARTESIAN_POINT('Ctrl Pts',(-6.2748675368223,-11.6690630215386,19.6418631629783));
#61901=CARTESIAN_POINT('Ctrl Pts',(-6.27482283433795,-11.6284198495329,
19.4852105192767));
#61902=CARTESIAN_POINT('Ctrl Pts',(-6.2747779149856,-11.5875795027186,19.3277978966284));
#61903=CARTESIAN_POINT('Ctrl Pts',(-6.27471535321751,-11.5438966073892,
19.1726096136311));
#61904=CARTESIAN_POINT('Ctrl Pts',(-6.27463536938977,-11.4976754978955,
19.0200386342048));
#61905=CARTESIAN_POINT('Ctrl Pts',(-6.27457690215347,-11.4638884110919,
18.9085110447105));
#61906=CARTESIAN_POINT('Ctrl Pts',(-6.27450912554786,-11.4287460092372,
18.7983814464739));
#61907=CARTESIAN_POINT('Ctrl Pts',(-6.27443212564381,-11.3923814819426,
18.6897930754465));
#61908=CARTESIAN_POINT('Ctrl Pts',(-6.2743563538205,-11.3565969368728,18.5829365934247));
#61909=CARTESIAN_POINT('Ctrl Pts',(-6.27427024653004,-11.3190562665239,
18.4758584939686));
#61910=CARTESIAN_POINT('Ctrl Pts',(-6.27417380377242,-11.279707466543,18.3686262100674));
#61911=CARTESIAN_POINT('Ctrl Pts',(-6.27399075391238,-11.2050228296955,
18.1650976606481));
#61912=CARTESIAN_POINT('Ctrl Pts',(-6.27377047091144,-11.1238233577958,
17.9610107904066));
#61913=CARTESIAN_POINT('Ctrl Pts',(-6.2735129547696,-11.0358409761326,17.7568349441134));
#61914=CARTESIAN_POINT('Ctrl Pts',(-6.27325823077298,-10.9488125524818,
17.5548728954104));
#61915=CARTESIAN_POINT('Ctrl Pts',(-6.27296707666657,-10.8551474376645,
17.3528237006521));
#61916=CARTESIAN_POINT('Ctrl Pts',(-6.27263949245036,-10.7546000178705,
17.1511902357532));
#61917=CARTESIAN_POINT('Ctrl Pts',(-6.27231699539509,-10.6556140313846,
16.9526880019566));
#61918=CARTESIAN_POINT('Ctrl Pts',(-6.27195919091438,-10.5499577801541,
16.754588644364));
#61919=CARTESIAN_POINT('Ctrl Pts',(-6.27156607900826,-10.4374113233089,
16.5574202692555));
#61920=CARTESIAN_POINT('Ctrl Pts',(-6.27136274846917,-10.3791985564473,
16.4554382346859));
#61921=CARTESIAN_POINT('Ctrl Pts',(-6.27114997212718,-10.319142693358,16.3537060639873));
#61922=CARTESIAN_POINT('Ctrl Pts',(-6.27092774998227,-10.2572149239311,
16.2523020893105));
#61923=CARTESIAN_POINT('Ctrl Pts',(-6.270506080497,-10.139706155087,16.0598866942392));
#61924=CARTESIAN_POINT('Ctrl Pts',(-6.27005040092663,-10.0154565177156,
15.8686500111997));
#61925=CARTESIAN_POINT('Ctrl Pts',(-6.26956071122401,-9.88428092908672,
15.6791641145428));
#61926=CARTESIAN_POINT('Ctrl Pts',(-6.269385046217,-9.83722467984934,15.6111903728333));
#61927=CARTESIAN_POINT('Ctrl Pts',(-6.26920500460963,-9.78927731157033,
15.5434423912217));
#61928=CARTESIAN_POINT('Ctrl Pts',(-6.26902058639972,-9.74043078973703,
15.4759481428237));
#61929=CARTESIAN_POINT('Ctrl Pts',(-6.26850853728607,-9.60480525567523,
15.2885459872248));
#61930=CARTESIAN_POINT('Ctrl Pts',(-6.26796274757707,-9.46224556682946,
15.103096995557));
#61931=CARTESIAN_POINT('Ctrl Pts',(-6.26738321722616,-9.31269176801434,
14.9201584331212));
#61932=CARTESIAN_POINT('Ctrl Pts',(-6.26681230202503,-9.16536119767451,
14.7399393885074));
#61933=CARTESIAN_POINT('Ctrl Pts',(-6.26620864188511,-9.01124286675024,
14.5621566742659));
#61934=CARTESIAN_POINT('Ctrl Pts',(-6.26557223676186,-8.85030877350661,
14.3873838069623));
#61935=CARTESIAN_POINT('Ctrl Pts',(-6.26502582981991,-8.71213341549658,
14.2373267058013));
#61936=CARTESIAN_POINT('Ctrl Pts',(-6.26445528440148,-8.56893413725298,
14.0894889713098));
#61937=CARTESIAN_POINT('Ctrl Pts',(-6.26386060047837,-8.42071136785102,
13.944258352743));
#61938=CARTESIAN_POINT('Ctrl Pts',(6.26385989014072,-8.4207183952526,13.9442649556632));
#61939=CARTESIAN_POINT('Ctrl Pts',(5.97439127923632,-8.54554836940733,13.9556074956481));
#61940=CARTESIAN_POINT('Ctrl Pts',(5.68299007296676,-8.66170806319399,13.9653100424049));
#61941=CARTESIAN_POINT('Ctrl Pts',(5.39014689160465,-8.76905158074534,13.973629824907));
#61942=CARTESIAN_POINT('Ctrl Pts',(5.11540307099319,-8.86976066330876,13.9814353979125));
#61943=CARTESIAN_POINT('Ctrl Pts',(4.83939001142658,-8.96270901393859,13.9880240320898));
#61944=CARTESIAN_POINT('Ctrl Pts',(4.56251287045879,-9.04781787373074,13.9936194822245));
#61945=CARTESIAN_POINT('Ctrl Pts',(4.30529839834099,-9.12688265447598,13.9988175666444));
#61946=CARTESIAN_POINT('Ctrl Pts',(4.04733821401237,-9.19918161327066,14.0031586462239));
#61947=CARTESIAN_POINT('Ctrl Pts',(3.78895714201621,-9.26469470268314,14.0068301382572));
#61948=CARTESIAN_POINT('Ctrl Pts',(3.5726868546934,-9.31953050997035,14.009903252827));
#61949=CARTESIAN_POINT('Ctrl Pts',(3.35612169198377,-9.3696126353749,14.0125073906));
#61950=CARTESIAN_POINT('Ctrl Pts',(3.13945213736916,-9.41495729916426,14.0147564904394));
#61951=CARTESIAN_POINT('Ctrl Pts',(2.89877806005409,-9.46532563604517,14.0172547649644));
#61952=CARTESIAN_POINT('Ctrl Pts',(2.65798320741555,-9.50986231004713,14.0193332725718));
#61953=CARTESIAN_POINT('Ctrl Pts',(2.41731281525442,-9.54854310212053,14.021048344074));
#61954=CARTESIAN_POINT('Ctrl Pts',(2.18015968341001,-9.58665859651125,14.0227383507859));
#61955=CARTESIAN_POINT('Ctrl Pts',(1.94312740078789,-9.61908808142941,14.0240754870134));
#61956=CARTESIAN_POINT('Ctrl Pts',(1.70645060761349,-9.64585877898722,14.0251184015268));
#61957=CARTESIAN_POINT('Ctrl Pts',(1.47135448327552,-9.6724506858542,14.0261543508348));
#61958=CARTESIAN_POINT('Ctrl Pts',(1.23660911590013,-9.69345906616529,14.0269000092261));
#61959=CARTESIAN_POINT('Ctrl Pts',(1.00244447583806,-9.7089616077502,14.0274173350616));
#61960=CARTESIAN_POINT('Ctrl Pts',(0.769963846594297,-9.72435266176066,
14.0279309405135));
#61961=CARTESIAN_POINT('Ctrl Pts',(0.538055622018907,-9.73431674912164,
14.0282194987896));
#61962=CARTESIAN_POINT('Ctrl Pts',(0.30694484651642,-9.73898112574318,14.0283478661244));
#61963=CARTESIAN_POINT('Ctrl Pts',(0.204466564770979,-9.74104938630157,
14.0284047862913));
#61964=CARTESIAN_POINT('Ctrl Pts',(0.102145075869552,-9.74207630888253,
14.0284302647289));
#61965=CARTESIAN_POINT('Ctrl Pts',(-9.86274122834492E-13,-9.74207626567393,
14.028430215033));
#61966=CARTESIAN_POINT('Ctrl Pts',(-0.000185913574553349,-9.74207626559528,
14.0284302149425));
#61967=CARTESIAN_POINT('Ctrl Pts',(-0.000371826563709544,-9.74207626211513,
14.0284302147675));
#61968=CARTESIAN_POINT('Ctrl Pts',(-0.000557738968337773,-9.74207625523356,
14.0284302145081));
#61969=CARTESIAN_POINT('Ctrl Pts',(-0.230883208579248,-9.74206772970903,
14.028429893058));
#61970=CARTESIAN_POINT('Ctrl Pts',(-0.462099352355539,-9.73683400689415,
14.0282994240873));
#61971=CARTESIAN_POINT('Ctrl Pts',(-0.693981990386209,-9.72622568352782,
14.0279722040158));
#61972=CARTESIAN_POINT('Ctrl Pts',(-0.927845006148299,-9.71552676050494,
14.0276421893438));
#61973=CARTESIAN_POINT('Ctrl Pts',(-1.16238594907491,-9.699361051742,14.0271120352145));
#61974=CARTESIAN_POINT('Ctrl Pts',(-1.39737484628166,-9.67762830339212,
14.0263176856921));
#61975=CARTESIAN_POINT('Ctrl Pts',(-1.63392438984921,-9.65575121999055,
14.0255180606067));
#61976=CARTESIAN_POINT('Ctrl Pts',(-1.87092785750831,-9.62823296750948,
14.024450705365));
#61977=CARTESIAN_POINT('Ctrl Pts',(-2.1081506638769,-9.59502420670042,14.023054791648));
#61978=CARTESIAN_POINT('Ctrl Pts',(-2.34834588913176,-9.56139933772146,
14.0216413870314));
#61979=CARTESIAN_POINT('Ctrl Pts',(-2.5887659841926,-9.52194050765764,14.0198911192562));
#61980=CARTESIAN_POINT('Ctrl Pts',(-2.82916743460895,-9.4766498428339,14.017745715887));
#61981=CARTESIAN_POINT('Ctrl Pts',(-2.93286958992579,-9.45711277452661,
14.0168202516146));
#61982=CARTESIAN_POINT('Ctrl Pts',(-3.03656827583359,-9.43649117750807,
14.0158213229269));
#61983=CARTESIAN_POINT('Ctrl Pts',(-3.14024394547988,-9.41478818616068,
14.0147445403436));
#61984=CARTESIAN_POINT('Ctrl Pts',(-3.40299004548275,-9.3597861171663,14.0120156414103));
#61985=CARTESIAN_POINT('Ctrl Pts',(-3.66557749758006,-9.29781677171979,
14.0087642670787));
#61986=CARTESIAN_POINT('Ctrl Pts',(-3.92766690418479,-9.22885719918551,
14.0047880768363));
#61987=CARTESIAN_POINT('Ctrl Pts',(-4.19856644078887,-9.15757955204227,
14.0006782270409));
#61988=CARTESIAN_POINT('Ctrl Pts',(-4.46893388554754,-9.07883436253647,
13.9957939467473));
#61989=CARTESIAN_POINT('Ctrl Pts',(-4.73839445092947,-8.99265632800915,
13.9899207517277));
#61990=CARTESIAN_POINT('Ctrl Pts',(-5.03365159885242,-8.89822811120468,
13.9834852912801));
#61991=CARTESIAN_POINT('Ctrl Pts',(-5.32781991713952,-8.79487607792431,
13.9758622779781));
#61992=CARTESIAN_POINT('Ctrl Pts',(-5.62040634468541,-8.68271089253479,
13.9667825708472));
#61993=CARTESIAN_POINT('Ctrl Pts',(-5.83581409549622,-8.60013272748902,
13.9600979159659));
#61994=CARTESIAN_POINT('Ctrl Pts',(-6.05036443188607,-8.51277917745374,
13.9526239758041));
#61995=CARTESIAN_POINT('Ctrl Pts',(-6.26386060047837,-8.42071136785102,
13.944258352743));
#61996=CARTESIAN_POINT('Ctrl Pts',(6.39615021386663,-8.39409409953866,13.9680027128311));
#61997=CARTESIAN_POINT('Ctrl Pts',(6.0981394504413,-8.52955034249946,13.9841958606635));
#61998=CARTESIAN_POINT('Ctrl Pts',(5.13855911511434,-8.93196846881188,14.0292676298103));
#61999=CARTESIAN_POINT('Ctrl Pts',(3.4042278071613,-9.47086396710915,14.0771763067071));
#62000=CARTESIAN_POINT('Ctrl Pts',(1.16260698888612,-9.8259538455241,14.100750462816));
#62001=CARTESIAN_POINT('Ctrl Pts',(-1.16569733333535,-9.82569779920851,
14.1007357383411));
#62002=CARTESIAN_POINT('Ctrl Pts',(-3.40685010597653,-9.47022124827926,
14.0771275227186));
#62003=CARTESIAN_POINT('Ctrl Pts',(-5.140066644375,-8.93138328509499,14.0292067344484));
#62004=CARTESIAN_POINT('Ctrl Pts',(-6.09875459911923,-8.52927070381225,
13.9841624342243));
#62005=CARTESIAN_POINT('Ctrl Pts',(-6.39614996063647,-8.39409419402682,
13.9680027190745));
#62006=CARTESIAN_POINT('Ctrl Pts',(6.17590518600828,-7.95710732525973,13.4973889894963));
#62007=CARTESIAN_POINT('Ctrl Pts',(5.88795326937256,-8.08714184605563,13.5139089189715));
#62008=CARTESIAN_POINT('Ctrl Pts',(4.96084266091442,-8.47346685614734,13.560052102495));
#62009=CARTESIAN_POINT('Ctrl Pts',(3.28578921021426,-8.99076845677069,13.6098152835045));
#62010=CARTESIAN_POINT('Ctrl Pts',(1.12196199728683,-9.33150995192134,13.6348906738451));
#62011=CARTESIAN_POINT('Ctrl Pts',(-1.12494446487316,-9.33126430248581,
13.6348747843078));
#62012=CARTESIAN_POINT('Ctrl Pts',(-3.28832124960869,-8.99015159077933,
13.6097640000083));
#62013=CARTESIAN_POINT('Ctrl Pts',(-4.96229906404752,-8.47290506114866,
13.5599894946589));
#62014=CARTESIAN_POINT('Ctrl Pts',(-5.88854765313263,-8.0868734027617,13.5138748169163));
#62015=CARTESIAN_POINT('Ctrl Pts',(-6.17590494057391,-7.95710741697555,
13.4973889956498));
#62016=CARTESIAN_POINT('Ctrl Pts',(6.16915737727431,-8.01757364818157,12.8211920463632));
#62017=CARTESIAN_POINT('Ctrl Pts',(5.88220122989312,-8.14587304019011,12.8375467559628));
#62018=CARTESIAN_POINT('Ctrl Pts',(4.95802580678134,-8.52723293522564,12.8832472984301));
#62019=CARTESIAN_POINT('Ctrl Pts',(3.28628703195018,-9.03882920094257,12.9325846801364));
#62020=CARTESIAN_POINT('Ctrl Pts',(1.12279040062947,-9.37660072493885,12.9574622751438));
#62021=CARTESIAN_POINT('Ctrl Pts',(-1.12577452523575,-9.3763569576825,12.9574465121303));
#62022=CARTESIAN_POINT('Ctrl Pts',(-3.28881618122004,-9.03821837019887,
12.9325338080592));
#62023=CARTESIAN_POINT('Ctrl Pts',(-4.95947798566805,-8.52667806159099,
12.8831852649638));
#62024=CARTESIAN_POINT('Ctrl Pts',(-5.88279356364298,-8.14560817488497,
12.8375129981983));
#62025=CARTESIAN_POINT('Ctrl Pts',(-6.16915713521142,-8.01757373702705,
12.8211920538159));
#62026=CARTESIAN_POINT('Ctrl Pts',(6.38081597772446,-8.53150930643574,12.4312991541261));
#62027=CARTESIAN_POINT('Ctrl Pts',(6.08506814081239,-8.66302236326436,12.4471168272863));
#62028=CARTESIAN_POINT('Ctrl Pts',(5.1321581266024,-9.05415696406033,12.491182660567));
#62029=CARTESIAN_POINT('Ctrl Pts',(3.40535948165785,-9.58008675116646,12.5381236733996));
#62030=CARTESIAN_POINT('Ctrl Pts',(1.16448971008638,-9.92842720330246,12.5612483214676));
#62031=CARTESIAN_POINT('Ctrl Pts',(-1.16758382053923,-9.92817543434746,
12.5612338845422));
#62032=CARTESIAN_POINT('Ctrl Pts',(-3.40797521272135,-9.579457747783,12.5380758243915));
#62033=CARTESIAN_POINT('Ctrl Pts',(-5.13365605611323,-9.05358750956378,
12.4911230705099));
#62034=CARTESIAN_POINT('Ctrl Pts',(-6.08567863075684,-8.66275085577762,
12.4470841832806));
#62035=CARTESIAN_POINT('Ctrl Pts',(-6.38081573215519,-8.53150939440301,
12.4312991633297));
#62036=CARTESIAN_POINT('',(-6.2499460327501,-8.55169213656735,12.4626541460308));
#62037=CARTESIAN_POINT('Origin',(-6.52772595968144,-9.09522655590529,13.2547537702088));
#62038=CARTESIAN_POINT('Ctrl Pts',(6.2499456683813,-8.55169360934562,12.4626524817952));
#62039=CARTESIAN_POINT('Ctrl Pts',(5.99497571757143,-8.66276623416142,12.4758503685831));
#62040=CARTESIAN_POINT('Ctrl Pts',(5.73509544265912,-8.76842077642134,12.4877092255716));
#62041=CARTESIAN_POINT('Ctrl Pts',(5.47038343317498,-8.868056192506,12.4983674133053));
#62042=CARTESIAN_POINT('Ctrl Pts',(5.26894837630338,-8.94387468576043,12.5064778600375));
#62043=CARTESIAN_POINT('Ctrl Pts',(5.06471576319851,-9.01620688869194,12.5138932611287));
#62044=CARTESIAN_POINT('Ctrl Pts',(4.85775981274984,-9.08476991994723,12.5206818391115));
#62045=CARTESIAN_POINT('Ctrl Pts',(4.61829824467732,-9.1641018306297,12.528536667761));
#62046=CARTESIAN_POINT('Ctrl Pts',(4.3751803125037,-9.23840063347297,12.5355463889511));
#62047=CARTESIAN_POINT('Ctrl Pts',(4.12852312077457,-9.30727351514831,12.5417718905077));
#62048=CARTESIAN_POINT('Ctrl Pts',(4.00519452491001,-9.34170995598598,12.544884641286));
#62049=CARTESIAN_POINT('Ctrl Pts',(3.88098152000299,-9.37479021607175,12.5478007973506));
#62050=CARTESIAN_POINT('Ctrl Pts',(3.75590130472956,-9.40646721059036,12.5505244941746));
#62051=CARTESIAN_POINT('Ctrl Pts',(3.69336119709285,-9.42230570784966,12.5518863425865));
#62052=CARTESIAN_POINT('Ctrl Pts',(3.63060428550466,-9.4377933813947,12.553200066749));
#62053=CARTESIAN_POINT('Ctrl Pts',(3.56763292198375,-9.45292452381646,12.5544659168596));
#62054=CARTESIAN_POINT('Ctrl Pts',(3.5361472402233,-9.46049009502734,12.5550988419149));
#62055=CARTESIAN_POINT('Ctrl Pts',(3.50460794541682,-9.46796653300947,12.5557197978829));
#62056=CARTESIAN_POINT('Ctrl Pts',(3.47301533729935,-9.47535312881161,12.5563288059489));
#62057=CARTESIAN_POINT('Ctrl Pts',(3.46349483562411,-9.47757909564053,12.556512331864));
#62058=CARTESIAN_POINT('Ctrl Pts',(3.45396949300403,-9.47979690408182,12.5566947722591));
#62059=CARTESIAN_POINT('Ctrl Pts',(3.44443931646769,-9.48200653383592,12.5568761285555));
#62060=CARTESIAN_POINT('Ctrl Pts',(3.43815713652989,-9.48346309570109,12.5569956764864));
#62061=CARTESIAN_POINT('Ctrl Pts',(3.43187285611465,-9.48491610368712,12.5571147533454));
#62062=CARTESIAN_POINT('Ctrl Pts',(3.42558647838356,-9.48636555303398,12.5572333589227));
#62063=CARTESIAN_POINT('Ctrl Pts',(3.40976355599046,-9.49001384232061,12.5575318912294));
#62064=CARTESIAN_POINT('Ctrl Pts',(3.39530296967644,-9.49332685868534,12.5578020467836));
#62065=CARTESIAN_POINT('Ctrl Pts',(3.37807788093079,-9.4972426942353,12.5581200099282));
#62066=CARTESIAN_POINT('Ctrl Pts',(3.0751556918768,-9.56610698250018,12.5637117426157));
#62067=CARTESIAN_POINT('Ctrl Pts',(2.76997585607743,-9.62598687169383,12.5682700097437));
#62068=CARTESIAN_POINT('Ctrl Pts',(2.4629153139001,-9.67662910251466,12.5719614267642));
#62069=CARTESIAN_POINT('Ctrl Pts',(2.16108112038875,-9.72640937317084,12.5755900137242));
#62070=CARTESIAN_POINT('Ctrl Pts',(1.85742917537775,-9.76726384928626,12.5783808667533));
#62071=CARTESIAN_POINT('Ctrl Pts',(1.55231579736879,-9.79890195725704,12.5804891643225));
#62072=CARTESIAN_POINT('Ctrl Pts',(1.4240166092259,-9.81220567928168,12.5813756966281));
#62073=CARTESIAN_POINT('Ctrl Pts',(1.29545903789866,-9.82387916506831,12.5821415155451));
#62074=CARTESIAN_POINT('Ctrl Pts',(1.16666981828216,-9.83389804518222,12.5827980829505));
#62075=CARTESIAN_POINT('Ctrl Pts',(0.860216072588966,-9.85773795466922,
12.5843603840599));
#62076=CARTESIAN_POINT('Ctrl Pts',(0.552449700108069,-9.87221279988117,
12.5853043714385));
#62077=CARTESIAN_POINT('Ctrl Pts',(0.243803444773064,-9.87721198877206,
12.5856295548017));
#62078=CARTESIAN_POINT('Ctrl Pts',(0.162408034707189,-9.87853036222625,
12.585715311336));
#62079=CARTESIAN_POINT('Ctrl Pts',(0.0809515130470044,-9.87918946580259,
12.5857580138753));
#62080=CARTESIAN_POINT('Ctrl Pts',(-0.000557986953597959,-9.87918669603315,
12.5857576143789));
#62081=CARTESIAN_POINT('Ctrl Pts',(-0.299520873003152,-9.87917653699318,
12.5857561490943));
#62082=CARTESIAN_POINT('Ctrl Pts',(-0.597728166319448,-9.87028485226777,
12.5851605051845));
#62083=CARTESIAN_POINT('Ctrl Pts',(-0.894817219028394,-9.85261539770727,
12.5839820704873));
#62084=CARTESIAN_POINT('Ctrl Pts',(-0.986618306464046,-9.84715550233833,
12.5836179319043));
#62085=CARTESIAN_POINT('Ctrl Pts',(-1.07831270681731,-9.84085711977231,
12.583198122586));
#62086=CARTESIAN_POINT('Ctrl Pts',(-1.16988990879901,-9.83372233090494,
12.5827229125624));
#62087=CARTESIAN_POINT('Ctrl Pts',(-1.34879551606369,-9.81978377734141,
12.5817945402602));
#62088=CARTESIAN_POINT('Ctrl Pts',(-1.5272538175031,-9.8026534714518,12.5806547311173));
#62089=CARTESIAN_POINT('Ctrl Pts',(-1.70519969857571,-9.78239209576105,
12.57927485804));
#62090=CARTESIAN_POINT('Ctrl Pts',(-1.9871029518838,-9.7502938662921,12.5770888523437));
#62091=CARTESIAN_POINT('Ctrl Pts',(-2.26770623515151,-9.71031298494122,
12.5743222105347));
#62092=CARTESIAN_POINT('Ctrl Pts',(-2.54672767284504,-9.66267617985082,
12.5708491197125));
#62093=CARTESIAN_POINT('Ctrl Pts',(-2.68623839169181,-9.63885777730561,
12.5691125743015));
#62094=CARTESIAN_POINT('Ctrl Pts',(-2.82535386091671,-9.61312634948936,
12.5671981611192));
#62095=CARTESIAN_POINT('Ctrl Pts',(-2.96404008610357,-9.58551587818721,
12.5650827887556));
#62096=CARTESIAN_POINT('Ctrl Pts',(-3.03338319869701,-9.57171064253614,
12.5640251025738));
#62097=CARTESIAN_POINT('Ctrl Pts',(-3.10261899674013,-9.55743563238489,
12.5629171586651));
#62098=CARTESIAN_POINT('Ctrl Pts',(-3.17174332330947,-9.54269552091794,
12.5617555625508));
#62099=CARTESIAN_POINT('Ctrl Pts',(-3.20630548659414,-9.53532546518447,
12.5611747644936));
#62100=CARTESIAN_POINT('Ctrl Pts',(-3.24083978174743,-9.52783913333813,
12.5605805523299));
#62101=CARTESIAN_POINT('Ctrl Pts',(-3.27534569080372,-9.52023711797875,
12.5599724850652));
#62102=CARTESIAN_POINT('Ctrl Pts',(-3.29259864533187,-9.51643611029907,
12.5596684514329));
#62103=CARTESIAN_POINT('Ctrl Pts',(-3.30984450331694,-9.512606181695,12.5593609539618));
#62104=CARTESIAN_POINT('Ctrl Pts',(-3.32708320031767,-9.50874740771603,
12.5590499357491));
#62105=CARTESIAN_POINT('Ctrl Pts',(-3.3443218973184,-9.50488863373705,12.5587389175364));
#62106=CARTESIAN_POINT('Ctrl Pts',(-3.36293312666133,-9.5006873055441,12.5583988970378));
#62107=CARTESIAN_POINT('Ctrl Pts',(-3.378777743974,-9.49708462554388,12.5581062613217));
#62108=CARTESIAN_POINT('Ctrl Pts',(-3.40160033225428,-9.49189532492979,
12.5576847488084));
#62109=CARTESIAN_POINT('Ctrl Pts',(-3.42439545405496,-9.4866585593598,12.5572574659275));
#62110=CARTESIAN_POINT('Ctrl Pts',(-3.44716295235235,-9.48137461708584,
12.5568243760515));
#62111=CARTESIAN_POINT('Ctrl Pts',(-3.72185578882046,-9.41762316437855,
12.5515990902102));
#62112=CARTESIAN_POINT('Ctrl Pts',(-3.99252581059805,-9.34700823075725,
12.5455274359759));
#62113=CARTESIAN_POINT('Ctrl Pts',(-4.2590050846537,-9.27009997597244,12.5385001292223));
#62114=CARTESIAN_POINT('Ctrl Pts',(-4.53204587047232,-9.19129801136636,
12.5312997892896));
#62115=CARTESIAN_POINT('Ctrl Pts',(-4.80068706808185,-9.10588893380199,
12.5230962144446));
#62116=CARTESIAN_POINT('Ctrl Pts',(-5.06476941248447,-9.01443703992606,
12.5137847237623));
#62117=CARTESIAN_POINT('Ctrl Pts',(-5.20182127086784,-8.9669758889857,12.5089523026279));
#62118=CARTESIAN_POINT('Ctrl Pts',(-5.33764561460797,-8.91788641265564,
12.5038216852713));
#62119=CARTESIAN_POINT('Ctrl Pts',(-5.4722222565736,-8.86724255974421,12.498379474696));
#62120=CARTESIAN_POINT('Ctrl Pts',(-5.73629434307178,-8.76786700904469,
12.4877005345708));
#62121=CARTESIAN_POINT('Ctrl Pts',(-5.99556164303099,-8.66250926796784,
12.4758212277278));
#62122=CARTESIAN_POINT('Ctrl Pts',(-6.24994585737753,-8.55169179341496,
12.4626536459473));
#62123=CARTESIAN_POINT('Ctrl Pts',(-6.23452463023104,-8.46817777445814,
13.9793247860141));
#62124=CARTESIAN_POINT('Ctrl Pts',(-6.26883579448648,-8.45422023761174,
13.9766717378257));
#62125=CARTESIAN_POINT('Ctrl Pts',(-6.38681948165088,-8.4004620524671,13.9705684989092));
#62126=CARTESIAN_POINT('Ctrl Pts',(-6.58037374888043,-8.27697442816996,
13.9789814227231));
#62127=CARTESIAN_POINT('Ctrl Pts',(-6.79245627860415,-8.07356528041172,
14.0233019893044));
#62128=CARTESIAN_POINT('Ctrl Pts',(-6.96282724046887,-7.82819097507957,
14.1005711232815));
#62129=CARTESIAN_POINT('Ctrl Pts',(-7.07881819325669,-7.55335221044515,
14.2073541386468));
#62130=CARTESIAN_POINT('Ctrl Pts',(-7.11903847741079,-7.3320169206708,14.3074069407329));
#62131=CARTESIAN_POINT('Ctrl Pts',(-7.1223300547874,-7.20833635409889,14.3683840363599));
#62132=CARTESIAN_POINT('Ctrl Pts',(-7.12201750162379,-7.17914631343674,
14.3830673400188));
#62133=CARTESIAN_POINT('Ctrl Pts',(-6.02296491909003,-8.0229515174066,13.5080161017831));
#62134=CARTESIAN_POINT('Ctrl Pts',(-6.05240779820068,-8.01109502665855,
13.5055635345619));
#62135=CARTESIAN_POINT('Ctrl Pts',(-6.15384509230703,-7.96537876837031,
13.4996013967755));
#62136=CARTESIAN_POINT('Ctrl Pts',(-6.32132139184434,-7.85990580767669,
13.5050734421016));
#62137=CARTESIAN_POINT('Ctrl Pts',(-6.5061768145196,-7.68510794243105,13.5407886398096));
#62138=CARTESIAN_POINT('Ctrl Pts',(-6.65550942751407,-7.4733210730188,13.6052594269033));
#62139=CARTESIAN_POINT('Ctrl Pts',(-6.75751726625292,-7.23561030969866,
13.6959374225502));
#62140=CARTESIAN_POINT('Ctrl Pts',(-6.79287018228396,-7.04443217880955,
13.7817350544861));
#62141=CARTESIAN_POINT('Ctrl Pts',(-6.79574426882679,-6.93808341830671,
13.8341161676123));
#62142=CARTESIAN_POINT('Ctrl Pts',(-6.79546946623675,-6.91302049420525,
13.8467286811972));
#62143=CARTESIAN_POINT('Ctrl Pts',(-6.00126870307733,-8.08913998801194,
12.8295907586597));
#62144=CARTESIAN_POINT('Ctrl Pts',(-6.04284582198358,-8.07265129772834,
12.8262979975003));
#62145=CARTESIAN_POINT('Ctrl Pts',(-6.18536698153368,-8.009419057336,12.8186086282347));
#62146=CARTESIAN_POINT('Ctrl Pts',(-6.41671326094832,-7.86606558233941,
12.8278122909668));
#62147=CARTESIAN_POINT('Ctrl Pts',(-6.66709581952829,-7.63353122744836,
12.8781674889523));
#62148=CARTESIAN_POINT('Ctrl Pts',(-6.86630942062206,-7.35614457211733,
12.9654853766482));
#62149=CARTESIAN_POINT('Ctrl Pts',(-7.00115184090513,-7.04757262155766,
13.085461092087));
#62150=CARTESIAN_POINT('Ctrl Pts',(-7.04795204044777,-6.79933349998106,
13.1977178770678));
#62151=CARTESIAN_POINT('Ctrl Pts',(-7.05182631606654,-6.65991344971732,
13.2664548440122));
#62152=CARTESIAN_POINT('Ctrl Pts',(-7.05146280075313,-6.62694954794606,
13.283035607156));
#62153=CARTESIAN_POINT('Ctrl Pts',(-6.18531856502411,-8.6182879511144,12.440699239874));
#62154=CARTESIAN_POINT('Ctrl Pts',(-6.24714938480481,-8.59382489176563,
12.4361406869405));
#62155=CARTESIAN_POINT('Ctrl Pts',(-6.45830856891384,-8.50034161670644,
12.4261201997568));
#62156=CARTESIAN_POINT('Ctrl Pts',(-6.79671573688593,-8.29094349054743,
12.442996182583));
#62157=CARTESIAN_POINT('Ctrl Pts',(-7.15740948686567,-7.95659180419277,
12.5205192982545));
#62158=CARTESIAN_POINT('Ctrl Pts',(-7.44090723754234,-7.56244152691377,
12.6496041416091));
#62159=CARTESIAN_POINT('Ctrl Pts',(-7.63136485385938,-7.12689428226258,
12.8228324436505));
#62160=CARTESIAN_POINT('Ctrl Pts',(-7.6975468214002,-6.77614844491688,12.9828928517768));
#62161=CARTESIAN_POINT('Ctrl Pts',(-7.70310676159879,-6.5774643832572,13.080963940675));
#62162=CARTESIAN_POINT('Ctrl Pts',(-7.70259301383401,-6.53035544843766,
13.1046469715588));
#62163=CARTESIAN_POINT('',(-7.000004044956,-6.97711954662123,13.9487143140163));
#62164=CARTESIAN_POINT('',(-7.,-8.04450891402614,12.5220421917952));
#62165=CARTESIAN_POINT('Ctrl Pts',(-7.,-6.97711954662123,13.9487143140163));
#62166=CARTESIAN_POINT('Ctrl Pts',(-7.,-7.02109862854982,13.8470307249955));
#62167=CARTESIAN_POINT('Ctrl Pts',(-7.,-7.06256666149218,13.7566966111574));
#62168=CARTESIAN_POINT('Ctrl Pts',(-7.,-7.10064521379527,13.6790951563344));
#62169=CARTESIAN_POINT('Ctrl Pts',(-7.,-7.11968448994682,13.6402944289229));
#62170=CARTESIAN_POINT('Ctrl Pts',(-7.,-7.13783856938113,13.6046507331564));
#62171=CARTESIAN_POINT('Ctrl Pts',(-7.,-7.1548263061793,13.5722133313273));
#62172=CARTESIAN_POINT('Ctrl Pts',(-7.,-7.16332017457839,13.5559946304127));
#62173=CARTESIAN_POINT('Ctrl Pts',(-7.,-7.17152128706493,13.540576415578));
#62174=CARTESIAN_POINT('Ctrl Pts',(-7.,-7.17939021066077,13.5259591637652));
#62175=CARTESIAN_POINT('Ctrl Pts',(-7.,-7.18332467245869,13.5186505378588));
#62176=CARTESIAN_POINT('Ctrl Pts',(-7.,-7.18717608703393,13.5115421527079));
#62177=CARTESIAN_POINT('Ctrl Pts',(-7.,-7.19093943869574,13.5046337282638));
#62178=CARTESIAN_POINT('Ctrl Pts',(-7.,-7.19282111452665,13.5011795160418));
#62179=CARTESIAN_POINT('Ctrl Pts',(-7.,-7.19468077462919,13.4977752939964));
#62180=CARTESIAN_POINT('Ctrl Pts',(-7.,-7.19651779951958,13.4944210212393));
#62181=CARTESIAN_POINT('Ctrl Pts',(-7.,-7.19835482440998,13.4910667484821));
#62182=CARTESIAN_POINT('Ctrl Pts',(-7.,-7.19936191322088,13.4892292594739));
#62183=CARTESIAN_POINT('Ctrl Pts',(-7.,-7.20196035000388,13.4845080053656));
#62184=CARTESIAN_POINT('Ctrl Pts',(-7.,-7.24353533853188,13.4089679396339));
#62185=CARTESIAN_POINT('Ctrl Pts',(-7.,-7.2857875477303,13.3377228575316));
#62186=CARTESIAN_POINT('Ctrl Pts',(-7.,-7.32834490361038,13.2712597190853));
#62187=CARTESIAN_POINT('Ctrl Pts',(-7.,-7.37090225949045,13.204796580639));
#62188=CARTESIAN_POINT('Ctrl Pts',(-7.,-7.41277352570555,13.1444220728118));
#62189=CARTESIAN_POINT('Ctrl Pts',(-7.,-7.45595082571483,13.0864229416019));
#62190=CARTESIAN_POINT('Ctrl Pts',(-7.,-7.54230542573338,12.970424679182));
#62191=CARTESIAN_POINT('Ctrl Pts',(-7.,-7.63588413976072,12.862461076247));
#62192=CARTESIAN_POINT('Ctrl Pts',(-7.,-7.73525747692535,12.7671752392972));
#62193=CARTESIAN_POINT('Ctrl Pts',(-7.,-7.83463081408998,12.6718894023474));
#62194=CARTESIAN_POINT('Ctrl Pts',(-7.,-7.93960130471208,12.589438500359));
#62195=CARTESIAN_POINT('Ctrl Pts',(-7.,-8.04450891402614,12.5220421917952));
#62196=CARTESIAN_POINT('Ctrl Pts',(-6.24994618627715,-8.55169243697437,
12.4626545838199));
#62197=CARTESIAN_POINT('Ctrl Pts',(-6.33574809474198,-8.51432360343295,
12.4582072698156));
#62198=CARTESIAN_POINT('Ctrl Pts',(-6.41863145615134,-8.47241225434573,
12.4571381176112));
#62199=CARTESIAN_POINT('Ctrl Pts',(-6.49887786889414,-8.42605295672793,
12.4592634833518));
#62200=CARTESIAN_POINT('Ctrl Pts',(-6.50612048271016,-8.42186881343789,
12.4594553075437));
#62201=CARTESIAN_POINT('Ctrl Pts',(-6.5133416130754,-8.41764841768038,12.4596731254631));
#62202=CARTESIAN_POINT('Ctrl Pts',(-6.5205414651617,-8.41339182738887,12.4599167852897));
#62203=CARTESIAN_POINT('Ctrl Pts',(-6.60751394034807,-8.3619732441917,12.4628601371768));
#62204=CARTESIAN_POINT('Ctrl Pts',(-6.69138037805353,-8.30527348498648,
12.4695747574696));
#62205=CARTESIAN_POINT('Ctrl Pts',(-6.77140175261942,-8.24377163592341,
12.4799351200026));
#62206=CARTESIAN_POINT('Ctrl Pts',(-6.84299358299183,-8.18874846280749,
12.4892041099578));
#62207=CARTESIAN_POINT('Ctrl Pts',(-6.91150928010844,-8.12988371948789,
12.5013942350656));
#62208=CARTESIAN_POINT('Ctrl Pts',(-6.97699397705138,-8.06692162074103,
12.5165626773547));
#62209=CARTESIAN_POINT('Ctrl Pts',(-6.98470443987939,-8.05950817997358,
12.5183486779913));
#62210=CARTESIAN_POINT('Ctrl Pts',(-6.99237288001724,-8.05203790662405,
12.5201759166414));
#62211=CARTESIAN_POINT('Ctrl Pts',(-6.99999936979046,-8.04451036076635,
12.5220444437838));
#62212=CARTESIAN_POINT('Ctrl Pts',(-6.26385884533749,-8.42070687883871,
13.9442629411756));
#62213=CARTESIAN_POINT('Ctrl Pts',(-6.28164430916676,-8.40909725695394,
13.9397078360192));
#62214=CARTESIAN_POINT('Ctrl Pts',(-6.2993722741453,-8.39692701207701,13.9353443706832));
#62215=CARTESIAN_POINT('Ctrl Pts',(-6.31700919643268,-8.38419168734846,
13.9311816754727));
#62216=CARTESIAN_POINT('Ctrl Pts',(-6.35928365267996,-8.35366601403318,
13.9212039892483));
#62217=CARTESIAN_POINT('Ctrl Pts',(-6.40103811124441,-8.31989232938067,
13.9123793956503));
#62218=CARTESIAN_POINT('Ctrl Pts',(-6.44183020701902,-8.28290854509716,
13.9047743211951));
#62219=CARTESIAN_POINT('Ctrl Pts',(-6.47172512654695,-8.25580458698962,
13.8992008618146));
#62220=CARTESIAN_POINT('Ctrl Pts',(-6.5011023245919,-8.22697699908308,13.8942824354648));
#62221=CARTESIAN_POINT('Ctrl Pts',(-6.52977104801251,-8.19644600892697,
13.8900489259368));
#62222=CARTESIAN_POINT('Ctrl Pts',(-6.53701932860586,-8.1887268935622,13.8889785725589));
#62223=CARTESIAN_POINT('Ctrl Pts',(-6.54422224509448,-8.18089890918468,
13.8879520232168));
#62224=CARTESIAN_POINT('Ctrl Pts',(-6.55137703981767,-8.17296294031462,
13.8869693750377));
#62225=CARTESIAN_POINT('Ctrl Pts',(-6.58908889829235,-8.1311336291371,13.8817899826867));
#62226=CARTESIAN_POINT('Ctrl Pts',(-6.62546758482145,-8.08630270607222,
13.877829455221));
#62227=CARTESIAN_POINT('Ctrl Pts',(-6.66008338922819,-8.03861158643723,
13.8751074498926));
#62228=CARTESIAN_POINT('Ctrl Pts',(-6.66685492532913,-8.02928226002585,
13.8745749718045));
#62229=CARTESIAN_POINT('Ctrl Pts',(-6.67355885667037,-8.01984353880004,
13.8740899238172));
#62230=CARTESIAN_POINT('Ctrl Pts',(-6.68019174663662,-8.01029656021264,
13.8736525109273));
#62231=CARTESIAN_POINT('Ctrl Pts',(-6.69130314370655,-7.99430349075988,
13.8729197581863));
#62232=CARTESIAN_POINT('Ctrl Pts',(-6.70221521440315,-7.97800661125738,
13.8723206718115));
#62233=CARTESIAN_POINT('Ctrl Pts',(-6.71291129475068,-7.96141141158149,
13.8718563685801));
#62234=CARTESIAN_POINT('Ctrl Pts',(-6.72172754331972,-7.94773281151101,
13.8714736664531));
#62235=CARTESIAN_POINT('Ctrl Pts',(-6.73039703334244,-7.93385153469644,
13.8711825417838));
#62236=CARTESIAN_POINT('Ctrl Pts',(-6.73891198148699,-7.91977220431998,
13.8709824492016));
#62237=CARTESIAN_POINT('Ctrl Pts',(-6.74833472334838,-7.90419185157249,
13.8707610243946));
#62238=CARTESIAN_POINT('Ctrl Pts',(-6.75756822273766,-7.88836896209251,
13.8706510740985));
#62239=CARTESIAN_POINT('Ctrl Pts',(-6.76660156287043,-7.87230998751464,
13.8706519436779));
#62240=CARTESIAN_POINT('Ctrl Pts',(-6.77111823293682,-7.8642805002257,13.8706523784676));
#62241=CARTESIAN_POINT('Ctrl Pts',(-6.77558485989446,-7.8561919898451,13.8706805202337));
#62242=CARTESIAN_POINT('Ctrl Pts',(-6.78000003558841,-7.84804528745407,
13.8707362961633));
#62243=CARTESIAN_POINT('Ctrl Pts',(-6.78270660742908,-7.84305123131353,
13.8707704876817));
#62244=CARTESIAN_POINT('Ctrl Pts',(-6.78573601458584,-7.83739413688215,
13.8708206650807));
#62245=CARTESIAN_POINT('Ctrl Pts',(-6.78845606288443,-7.83225166154178,
13.8708779062954));
#62246=CARTESIAN_POINT('Ctrl Pts',(-6.79017317415198,-7.82900532126369,
13.8709140415121));
#62247=CARTESIAN_POINT('Ctrl Pts',(-6.79176802387397,-7.8259647425448,13.870952434692));
#62248=CARTESIAN_POINT('Ctrl Pts',(-6.7930897838889,-7.82343142964423,13.8709864626005));
#62249=CARTESIAN_POINT('Ctrl Pts',(-6.81076623182257,-7.78955237967999,
13.8714415320118));
#62250=CARTESIAN_POINT('Ctrl Pts',(-6.82804731998309,-7.75374239582446,
13.8723500658969));
#62251=CARTESIAN_POINT('Ctrl Pts',(-6.84464290043939,-7.71596402803055,
13.8737975583038));
#62252=CARTESIAN_POINT('Ctrl Pts',(-6.84884551603565,-7.70639714616643,
13.8741641169897));
#62253=CARTESIAN_POINT('Ctrl Pts',(-6.85300394537083,-7.69670415794422,
13.8745652494736));
#62254=CARTESIAN_POINT('Ctrl Pts',(-6.85711299825419,-7.68688471531696,
13.8750023702786));
#62255=CARTESIAN_POINT('Ctrl Pts',(-6.87261613350537,-7.64983672604478,
13.8766515928983));
#62256=CARTESIAN_POINT('Ctrl Pts',(-6.88741903444732,-7.6109861396205,13.8788133699042));
#62257=CARTESIAN_POINT('Ctrl Pts',(-6.90125024927014,-7.57035421419371,
13.8815453788709));
#62258=CARTESIAN_POINT('Ctrl Pts',(-6.91403168206642,-7.53280623081852,
13.8840700297749));
#62259=CARTESIAN_POINT('Ctrl Pts',(-6.92598337927363,-7.49373721201718,
13.8870815422083));
#62260=CARTESIAN_POINT('Ctrl Pts',(-6.93686114758191,-7.45318980081384,
13.8906237642641));
#62261=CARTESIAN_POINT('Ctrl Pts',(-6.94303774585016,-7.43016622991928,
13.8926351035384));
#62262=CARTESIAN_POINT('Ctrl Pts',(-6.94886754432856,-7.40666644740578,
13.8948175490587));
#62263=CARTESIAN_POINT('Ctrl Pts',(-6.95430081976807,-7.38270217973598,
13.8971790243926));
#62264=CARTESIAN_POINT('Ctrl Pts',(-6.96395630575806,-7.34011522582167,
13.9013756075138));
#62265=CARTESIAN_POINT('Ctrl Pts',(-6.9723612927587,-7.29605906095144,13.9061378933399));
#62266=CARTESIAN_POINT('Ctrl Pts',(-6.97925043175555,-7.25064769251095,
13.9114910616584));
#62267=CARTESIAN_POINT('Ctrl Pts',(-6.98579308269724,-7.20752028099744,
13.9165749933015));
#62268=CARTESIAN_POINT('Ctrl Pts',(-6.99096887006084,-7.16317064731089,
13.9221917460347));
#62269=CARTESIAN_POINT('Ctrl Pts',(-6.99451703428925,-7.11772928270794,
13.9283605810957));
#62270=CARTESIAN_POINT('Ctrl Pts',(-6.99591396140104,-7.09983882721493,
13.9307892772863));
#62271=CARTESIAN_POINT('Ctrl Pts',(-6.99705819555185,-7.08177951502153,
13.9333035312008));
#62272=CARTESIAN_POINT('Ctrl Pts',(-6.9979320935569,-7.06356077431209,13.9359044736482));
#62273=CARTESIAN_POINT('Ctrl Pts',(-6.99929644409143,-7.03511723916062,
13.9399651274063));
#62274=CARTESIAN_POINT('Ctrl Pts',(-7.00000204474255,-7.00628463245252,
13.9442371933808));
#62275=CARTESIAN_POINT('Ctrl Pts',(-6.99999554931096,-6.9771195483688,13.9487143130749));
#62276=CARTESIAN_POINT('Ctrl Pts',(-6.2341316903218,-11.8700315082968,24.3933909558656));
#62277=CARTESIAN_POINT('Ctrl Pts',(-6.23490699037994,-11.9504773632788,
23.8924703016508));
#62278=CARTESIAN_POINT('Ctrl Pts',(-6.23649478643264,-12.0627644821299,
22.7260267664735));
#62279=CARTESIAN_POINT('Ctrl Pts',(-6.23804164013149,-11.9701367284916,
20.8893389425408));
#62280=CARTESIAN_POINT('Ctrl Pts',(-6.23759444471014,-11.5416371344917,
18.9411595572409));
#62281=CARTESIAN_POINT('Ctrl Pts',(-6.23570527570309,-10.7961451800346,
17.0892602672504));
#62282=CARTESIAN_POINT('Ctrl Pts',(-6.23205146828093,-9.75631874546476,
15.3875905681178));
#62283=CARTESIAN_POINT('Ctrl Pts',(-6.22726292200935,-8.61699832153917,
14.0755233161913));
#62284=CARTESIAN_POINT('Ctrl Pts',(-6.22400337583775,-7.81350279629324,
13.3673858160704));
#62285=CARTESIAN_POINT('Ctrl Pts',(-6.2226678388619,-7.49367893859873,13.1134099685414));
#62286=CARTESIAN_POINT('Ctrl Pts',(-6.72599077992547,-11.7530848388885,
24.374565981612));
#62287=CARTESIAN_POINT('Ctrl Pts',(-6.72668393615475,-11.832344276316,23.8785345357962));
#62288=CARTESIAN_POINT('Ctrl Pts',(-6.72805219773479,-11.9427130855079,
22.723533396798));
#62289=CARTESIAN_POINT('Ctrl Pts',(-6.7294197444849,-11.8502304322583,20.9054813875764));
#62290=CARTESIAN_POINT('Ctrl Pts',(-6.72902474491262,-11.4262585077992,
18.976797872896));
#62291=CARTESIAN_POINT('Ctrl Pts',(-6.72736869125189,-10.6891570039499,
17.1431712553454));
#62292=CARTESIAN_POINT('Ctrl Pts',(-6.72416503158331,-9.66125809165063,
15.457401490674));
#62293=CARTESIAN_POINT('Ctrl Pts',(-6.71993417357258,-8.53486250336011,
14.1564714981381));
#62294=CARTESIAN_POINT('Ctrl Pts',(-6.717079659789,-7.74007006277861,13.4537931851715));
#62295=CARTESIAN_POINT('Ctrl Pts',(-6.71589093229416,-7.42368913606096,
13.2016833831309));
#62296=CARTESIAN_POINT('Ctrl Pts',(-7.02718513800354,-11.3520754412046,
24.3100156203626));
#62297=CARTESIAN_POINT('Ctrl Pts',(-7.02756383162633,-11.4283591366048,
23.830925349047));
#62298=CARTESIAN_POINT('Ctrl Pts',(-7.02824874199597,-11.5344313266266,
22.7152029731697));
#62299=CARTESIAN_POINT('Ctrl Pts',(-7.02897706253925,-11.4446314644105,
20.9601359261015));
#62300=CARTESIAN_POINT('Ctrl Pts',(-7.02876713792981,-11.035338635164,19.0974438705216));
#62301=CARTESIAN_POINT('Ctrl Pts',(-7.02790260273523,-10.3242142898863,
17.3268280635606));
#62302=CARTESIAN_POINT('Ctrl Pts',(-7.02622925523404,-9.33267502688829,
15.6982407576233));
#62303=CARTESIAN_POINT('Ctrl Pts',(-7.02397923349865,-8.2459987393316,14.440709165306));
#62304=CARTESIAN_POINT('Ctrl Pts',(-7.02249255579137,-7.47887749031547,
13.7610287608176));
#62305=CARTESIAN_POINT('Ctrl Pts',(-7.02184959359837,-7.1735607452346,13.5171523616262));
#62306=CARTESIAN_POINT('Ctrl Pts',(-6.9983806301446,-10.8539092122116,24.2298260574574));
#62307=CARTESIAN_POINT('Ctrl Pts',(-6.99835913464222,-10.9268139731601,
23.7718327055695));
#62308=CARTESIAN_POINT('Ctrl Pts',(-6.99821532667477,-11.0282121120616,
22.7049180447452));
#62309=CARTESIAN_POINT('Ctrl Pts',(-6.99814245624674,-10.9423806584636,
21.0278292308067));
#62310=CARTESIAN_POINT('Ctrl Pts',(-6.99816421977348,-10.5510772324376,
19.2468670090286));
#62311=CARTESIAN_POINT('Ctrl Pts',(-6.99828069438708,-9.87141121253356,
17.5546312641458));
#62312=CARTESIAN_POINT('Ctrl Pts',(-6.99850457248202,-8.92372034671503,
15.9978548351403));
#62313=CARTESIAN_POINT('Ctrl Pts',(-6.99873523799494,-7.88504859624807,
14.795751341076));
#62314=CARTESIAN_POINT('Ctrl Pts',(-6.99894168320714,-7.15167106408799,
14.1458852642028));
#62315=CARTESIAN_POINT('Ctrl Pts',(-6.99898903509106,-6.85988342429147,
13.9127707408451));
#62316=CARTESIAN_POINT('',(-7.00000308919771,-10.9277695878957,24.1259430625668));
#62317=CARTESIAN_POINT('Origin',(-5.99998370364536,-10.9277595200191,24.1259473098659));
#62318=CARTESIAN_POINT('Ctrl Pts',(-7.00001101651408,-10.9277661740993,
24.1259401090719));
#62319=CARTESIAN_POINT('Ctrl Pts',(-7.00001786889488,-10.9560762031794,
23.9375964225754));
#62320=CARTESIAN_POINT('Ctrl Pts',(-7.0000180252376,-10.9791075349139,23.751169245318));
#62321=CARTESIAN_POINT('Ctrl Pts',(-7.0000155683987,-10.9972399153364,23.5670036403763));
#62322=CARTESIAN_POINT('Ctrl Pts',(-7.00001306417673,-11.0157220002865,
23.3792861826514));
#62323=CARTESIAN_POINT('Ctrl Pts',(-7.00000784356584,-11.0291144018999,
23.1939182824481));
#62324=CARTESIAN_POINT('Ctrl Pts',(-7.00000354838541,-11.0378129296526,
23.011211620191));
#62325=CARTESIAN_POINT('Ctrl Pts',(-7.00000225630628,-11.04042962677,22.9562496760505));
#62326=CARTESIAN_POINT('Ctrl Pts',(-7.00000104345542,-11.0426215149221,
22.9015281983146));
#62327=CARTESIAN_POINT('Ctrl Pts',(-6.99999999753982,-11.0443992483831,
22.8470547661776));
#62328=CARTESIAN_POINT('Ctrl Pts',(-6.99999887666316,-11.046304392478,22.7886772085523));
#62329=CARTESIAN_POINT('Ctrl Pts',(-6.99999794690482,-11.0477338974152,
22.7305845211254));
#62330=CARTESIAN_POINT('Ctrl Pts',(-6.99999718086736,-11.0487021770247,
22.6727837229349));
#62331=CARTESIAN_POINT('Ctrl Pts',(-6.99999462214162,-11.0519364339199,
22.4797169390654));
#62332=CARTESIAN_POINT('Ctrl Pts',(-6.99999387750136,-11.0500263261682,
22.2899104602776));
#62333=CARTESIAN_POINT('Ctrl Pts',(-6.99999403434629,-11.043495911084,22.1035935549034));
#62334=CARTESIAN_POINT('Ctrl Pts',(-6.99999406716594,-11.0421294278094,
22.0646069159697));
#62335=CARTESIAN_POINT('Ctrl Pts',(-6.99999414003137,-11.0405605734448,
22.0257729004208));
#62336=CARTESIAN_POINT('Ctrl Pts',(-6.99999424548543,-11.0387940382169,
21.9870933459717));
#62337=CARTESIAN_POINT('Ctrl Pts',(-6.99999432422075,-11.0374750876385,
21.9582139780964));
#62338=CARTESIAN_POINT('Ctrl Pts',(-6.99999441862992,-11.0360814573681,
21.9301066666266));
#62339=CARTESIAN_POINT('Ctrl Pts',(-6.99999453138847,-11.0345337323243,
21.9011846437886));
#62340=CARTESIAN_POINT('Ctrl Pts',(-6.99999463682025,-11.0330865746049,
21.8741419020701));
#62341=CARTESIAN_POINT('Ctrl Pts',(-6.9999947584713,-11.0315045785116,21.8463868423182));
#62342=CARTESIAN_POINT('Ctrl Pts',(-6.99999490350797,-11.0296819417538,
21.8166248372066));
#62343=CARTESIAN_POINT('Ctrl Pts',(-6.99999520366033,-11.025910007751,21.755032576106));
#62344=CARTESIAN_POINT('Ctrl Pts',(-6.99999556265624,-11.0216269204843,
21.6935869074157));
#62345=CARTESIAN_POINT('Ctrl Pts',(-6.99999595370107,-11.0168388725623,
21.632295583509));
#62346=CARTESIAN_POINT('Ctrl Pts',(-6.99999673579073,-11.0072627767184,
21.5097129356955));
#62347=CARTESIAN_POINT('Ctrl Pts',(-6.99999764537197,-10.9956668382537,
21.3877476670165));
#62348=CARTESIAN_POINT('Ctrl Pts',(-6.99999847632105,-10.9821001926362,
21.2664591708761));
#62349=CARTESIAN_POINT('Ctrl Pts',(-6.99999902465854,-10.9731476580993,
21.1864217407523));
#62350=CARTESIAN_POINT('Ctrl Pts',(-6.99999953897964,-10.9633369529758,
21.1066789596586));
#62351=CARTESIAN_POINT('Ctrl Pts',(-6.99999996276679,-10.9526820926811,
21.0272472280891));
#62352=CARTESIAN_POINT('Ctrl Pts',(-7.00000126736906,-10.919881771297,20.7827216077141));
#62353=CARTESIAN_POINT('Ctrl Pts',(-7.00000171385151,-10.8790827758835,
20.5411475182533));
#62354=CARTESIAN_POINT('Ctrl Pts',(-7.00000170643222,-10.8307712017266,
20.303018538099));
#62355=CARTESIAN_POINT('Ctrl Pts',(-7.0000016989336,-10.7819430682013,20.0623434236541));
#62356=CARTESIAN_POINT('Ctrl Pts',(-7.00000122940885,-10.7254408509918,
19.8251874411523));
#62357=CARTESIAN_POINT('Ctrl Pts',(-7.00000072342005,-10.6617508826813,
19.5920091224918));
#62358=CARTESIAN_POINT('Ctrl Pts',(-7.00000046988404,-10.6298377246556,
19.4751703686194));
#62359=CARTESIAN_POINT('Ctrl Pts',(-7.00000020716509,-10.596119684273,19.3593295013968));
#62360=CARTESIAN_POINT('Ctrl Pts',(-6.99999998766534,-10.5606564961048,
19.2445395219721));
#62361=CARTESIAN_POINT('Ctrl Pts',(-6.9999999392903,-10.5528408476764,19.2192412290483));
#62362=CARTESIAN_POINT('Ctrl Pts',(-6.99999989300842,-10.5449404325926,
19.1939939665953));
#62363=CARTESIAN_POINT('Ctrl Pts',(-6.9999998487871,-10.5369560034589,19.168798203842));
#62364=CARTESIAN_POINT('Ctrl Pts',(-6.99999965374745,-10.5017404042032,
19.0576714258086));
#62365=CARTESIAN_POINT('Ctrl Pts',(-6.99999949863786,-10.4648906001592,
18.9475466497737));
#62366=CARTESIAN_POINT('Ctrl Pts',(-6.99999938184555,-10.4264703353217,
18.8384626494681));
#62367=CARTESIAN_POINT('Ctrl Pts',(-6.99999932344939,-10.4072602029029,
18.7839206493154));
#62368=CARTESIAN_POINT('Ctrl Pts',(-6.99999927466386,-10.3876574552857,
18.7296388430949));
#62369=CARTESIAN_POINT('Ctrl Pts',(-6.99999923547135,-10.3676699120197,
18.6756218120257));
#62370=CARTESIAN_POINT('Ctrl Pts',(-6.9999992158751,-10.3576761403867,18.6486132964911));
#62371=CARTESIAN_POINT('Ctrl Pts',(-6.99999919867912,-10.3475861698415,
18.6216709747444));
#62372=CARTESIAN_POINT('Ctrl Pts',(-6.99999918389318,-10.3374009734139,
18.5947954116279));
#62373=CARTESIAN_POINT('Ctrl Pts',(-6.99999917282785,-10.329778691202,18.5746825813911));
#62374=CARTESIAN_POINT('Ctrl Pts',(-6.99999916268459,-10.321739978571,18.5536617628498));
#62375=CARTESIAN_POINT('Ctrl Pts',(-6.99999915445592,-10.31409939832,18.5338560637672));
#62376=CARTESIAN_POINT('Ctrl Pts',(-6.99999915168912,-10.3115303315763,
18.5271966005881));
#62377=CARTESIAN_POINT('Ctrl Pts',(-6.99999914912874,-10.3090066973727,
18.5206743536049));
#62378=CARTESIAN_POINT('Ctrl Pts',(-6.9999991467833,-10.3065606770019,18.5143695585423));
#62379=CARTESIAN_POINT('Ctrl Pts',(-6.99999907528818,-10.231999700937,18.3221832303493));
#62380=CARTESIAN_POINT('Ctrl Pts',(-6.99999912491176,-10.1510711355307,
18.1296181412436));
#62381=CARTESIAN_POINT('Ctrl Pts',(-6.99999933315459,-10.0634926000564,
17.9371553317586));
#62382=CARTESIAN_POINT('Ctrl Pts',(-6.99999947285314,-10.0047410237252,
17.8080427200765));
#62383=CARTESIAN_POINT('Ctrl Pts',(-6.99999968442971,-9.94299694259285,
17.6789771457935));
#62384=CARTESIAN_POINT('Ctrl Pts',(-6.99999998816768,-9.87817779118915,
17.5501167562952));
#62385=CARTESIAN_POINT('Ctrl Pts',(-7.00000042904169,-9.78409314535192,
17.3630766015592));
#62386=CARTESIAN_POINT('Ctrl Pts',(-7.00000106782039,-9.68352889475653,
17.1764665511887));
#62387=CARTESIAN_POINT('Ctrl Pts',(-7.00000153333001,-9.57627847396805,
16.9908083130017));
#62388=CARTESIAN_POINT('Ctrl Pts',(-7.00000199137045,-9.47074890330964,
16.8081289908971));
#62389=CARTESIAN_POINT('Ctrl Pts',(-7.00000228134333,-9.35874595195695,
16.6263711514362));
#62390=CARTESIAN_POINT('Ctrl Pts',(-7.00000202664151,-9.24008883380642,
16.446079218847));
#62391=CARTESIAN_POINT('Ctrl Pts',(-7.00000181210071,-9.1401414001778,16.2942154600847));
#62392=CARTESIAN_POINT('Ctrl Pts',(-7.00000121063313,-9.03547304290156,
16.1433925290633));
#62393=CARTESIAN_POINT('Ctrl Pts',(-6.99999998662452,-8.92598518393872,
15.9939629313457));
#62394=CARTESIAN_POINT('Ctrl Pts',(-6.99999852879618,-8.79558209416524,
15.8159881181512));
#62395=CARTESIAN_POINT('Ctrl Pts',(-6.9999961728163,-8.6583410520032,15.6399892306821));
#62396=CARTESIAN_POINT('Ctrl Pts',(-6.9999944983877,-8.51418146148609,15.4665322542966));
#62397=CARTESIAN_POINT('Ctrl Pts',(-6.99999284818175,-8.37210731493886,
15.2955845442328));
#62398=CARTESIAN_POINT('Ctrl Pts',(-6.99999186149943,-8.22331328898852,
15.1271057140513));
#62399=CARTESIAN_POINT('Ctrl Pts',(-6.99999320063754,-8.0677498898833,14.9616796343078));
#62400=CARTESIAN_POINT('Ctrl Pts',(-6.99999413393874,-7.9593312685555,14.8463872994744));
#62401=CARTESIAN_POINT('Ctrl Pts',(-6.99999620011487,-7.84762514473388,
14.7325786384935));
#62402=CARTESIAN_POINT('Ctrl Pts',(-6.99999999965493,-7.73262311891675,
14.6204637825058));
#62403=CARTESIAN_POINT('Ctrl Pts',(-7.00000506889666,-7.57919058243494,
14.4708832285177));
#62404=CARTESIAN_POINT('Ctrl Pts',(-7.00001329865542,-7.4198895840185,14.3243159680113));
#62405=CARTESIAN_POINT('Ctrl Pts',(-7.00001657747118,-7.25480415599887,
14.1813331106406));
#62406=CARTESIAN_POINT('Ctrl Pts',(-7.00001838123028,-7.16398650538121,
14.1026746406546));
#62407=CARTESIAN_POINT('Ctrl Pts',(-7.00001867170311,-7.07141884697089,
14.0251016321159));
#62408=CARTESIAN_POINT('Ctrl Pts',(-7.00001598754464,-6.97711954671267,
13.9487143134838));
#62409=CARTESIAN_POINT('Origin',(-5.9999949808,-10.9277770011797,24.1259380084106));
#62410=CARTESIAN_POINT('Origin',(-6.,-10.9277790621883,24.1259427055448));
#62411=CARTESIAN_POINT('Ctrl Pts',(-7.10692994354395,-5.08477020587198,
15.2195232722513));
#62412=CARTESIAN_POINT('Ctrl Pts',(-7.10723905417148,-5.05413024983052,
15.2296541384606));
#62413=CARTESIAN_POINT('Ctrl Pts',(-7.10399806473613,-4.92454784617344,
15.2736511084783));
#62414=CARTESIAN_POINT('Ctrl Pts',(-7.06411031942477,-4.69882499679942,
15.3588366457335));
#62415=CARTESIAN_POINT('Ctrl Pts',(-6.94880758813024,-4.43055877160903,
15.4770235844201));
#62416=CARTESIAN_POINT('Ctrl Pts',(-6.77939710086492,-4.20377723167178,
15.5952641304998));
#62417=CARTESIAN_POINT('Ctrl Pts',(-6.56851488585849,-4.02968927075824,
15.7071589740343));
#62418=CARTESIAN_POINT('Ctrl Pts',(-6.38416972253453,-3.94091623381668,
15.7846830843128));
#62419=CARTESIAN_POINT('Ctrl Pts',(-6.27575645452224,-3.90850154064671,
15.8240515790601));
#62420=CARTESIAN_POINT('Ctrl Pts',(-6.25032976362752,-3.90191196399198,
15.8329676265128));
#62421=CARTESIAN_POINT('Ctrl Pts',(-6.8147193961081,-4.89995455584871,14.669953164421));
#62422=CARTESIAN_POINT('Ctrl Pts',(-6.81499727225807,-4.87301572262855,
14.678855934617));
#62423=CARTESIAN_POINT('Ctrl Pts',(-6.812099620586,-4.75899734568318,14.7176111603106));
#62424=CARTESIAN_POINT('Ctrl Pts',(-6.77625084285897,-4.55998596348717,
14.7932537684509));
#62425=CARTESIAN_POINT('Ctrl Pts',(-6.67257963290984,-4.323764131131,14.8988444918356));
#62426=CARTESIAN_POINT('Ctrl Pts',(-6.52065733174994,-4.12487388367177,
15.0046751914328));
#62427=CARTESIAN_POINT('Ctrl Pts',(-6.33237309875386,-3.97312546011465,
15.1046826999853));
#62428=CARTESIAN_POINT('Ctrl Pts',(-6.16872308841693,-3.89638081767529,
15.1736714985496));
#62429=CARTESIAN_POINT('Ctrl Pts',(-6.07292775271076,-3.86852699329058,
15.2085479485238));
#62430=CARTESIAN_POINT('Ctrl Pts',(-6.05048519755294,-3.86287441690861,
15.21643737952));
#62431=CARTESIAN_POINT('Ctrl Pts',(-7.05843403097223,-4.7130617286742,14.0978966120729));
#62432=CARTESIAN_POINT('Ctrl Pts',(-7.05879586671931,-4.67818074142654,
14.1094309207911));
#62433=CARTESIAN_POINT('Ctrl Pts',(-7.05495515045979,-4.53092818779582,
14.1594239869758));
#62434=CARTESIAN_POINT('Ctrl Pts',(-7.00823869674784,-4.2757195561268,14.2556529815483));
#62435=CARTESIAN_POINT('Ctrl Pts',(-6.87332612944898,-3.97204539859998,
14.3892289048133));
#62436=CARTESIAN_POINT('Ctrl Pts',(-6.67392435495462,-3.71358706477726,
14.5238465046092));
#62437=CARTESIAN_POINT('Ctrl Pts',(-6.42325605566937,-3.51309045810733,
14.6528732158932));
#62438=CARTESIAN_POINT('Ctrl Pts',(-6.20134644756911,-3.40949261292977,
14.7438913470207));
#62439=CARTESIAN_POINT('Ctrl Pts',(-6.06951804969259,-3.37139329470379,
14.7908144841238));
#62440=CARTESIAN_POINT('Ctrl Pts',(-6.03852631344346,-3.3636365870849,14.8014824694433));
#62441=CARTESIAN_POINT('Ctrl Pts',(-7.6717391352104,-4.65164535922602,13.8937800218627));
#62442=CARTESIAN_POINT('Ctrl Pts',(-7.67224282244008,-4.60259943959517,
13.9100094857634));
#62443=CARTESIAN_POINT('Ctrl Pts',(-7.66681627817998,-4.39599674101868,
13.9800501817312));
#62444=CARTESIAN_POINT('Ctrl Pts',(-7.60174266337897,-4.04003661333773,
14.1129447256398));
#62445=CARTESIAN_POINT('Ctrl Pts',(-7.41403799907221,-3.61544944133095,
14.2959874416183));
#62446=CARTESIAN_POINT('Ctrl Pts',(-7.13459369944867,-3.25061869911762,
14.4809417081011));
#62447=CARTESIAN_POINT('Ctrl Pts',(-6.77913623589666,-2.96355669078003,
14.6600886342619));
#62448=CARTESIAN_POINT('Ctrl Pts',(-6.45977429108566,-2.81255128298632,
14.7886657841067));
#62449=CARTESIAN_POINT('Ctrl Pts',(-6.2678543001219,-2.75639262976502,14.8559525099445));
#62450=CARTESIAN_POINT('Ctrl Pts',(-6.22261485799,-2.74492672320326,14.8713078648157));
#62451=CARTESIAN_POINT('',(-6.26385971950436,-3.9057407515351,15.8144217911625));
#62452=CARTESIAN_POINT('',(-6.249946055744,-2.76546777341919,14.8593868371358));
#62453=CARTESIAN_POINT('Ctrl Pts',(-6.26385883867456,-3.90574397279466,
15.8144218264466));
#62454=CARTESIAN_POINT('Ctrl Pts',(-6.2543726558507,-3.90347224101743,15.7850081696593));
#62455=CARTESIAN_POINT('Ctrl Pts',(-6.24505636291581,-3.8997586331618,15.754970629442));
#62456=CARTESIAN_POINT('Ctrl Pts',(-6.23601489483689,-3.89445412934997,
15.7244810600636));
#62457=CARTESIAN_POINT('Ctrl Pts',(-6.22720005999169,-3.88928258811033,
15.6947557415395));
#62458=CARTESIAN_POINT('Ctrl Pts',(-6.21864673046565,-3.88259822555066,
15.6646010810059));
#62459=CARTESIAN_POINT('Ctrl Pts',(-6.21045783981734,-3.87429084484968,
15.6342165675576));
#62460=CARTESIAN_POINT('Ctrl Pts',(-6.20239515995553,-3.86611150115605,
15.6043003536025));
#62461=CARTESIAN_POINT('Ctrl Pts',(-6.194686087777,-3.85635816263781,15.5741617702321));
#62462=CARTESIAN_POINT('Ctrl Pts',(-6.18743004151878,-3.84496269666555,
15.5440252032908));
#62463=CARTESIAN_POINT('Ctrl Pts',(-6.1803014986827,-3.83376747209979,15.5144181968401));
#62464=CARTESIAN_POINT('Ctrl Pts',(-6.17361052747927,-3.82098688893042,
15.4848137750982));
#62465=CARTESIAN_POINT('Ctrl Pts',(-6.16744778180624,-3.80660015448518,
15.455449660021));
#62466=CARTESIAN_POINT('Ctrl Pts',(-6.16664974576687,-3.80473716464505,
15.4516471954477));
#62467=CARTESIAN_POINT('Ctrl Pts',(-6.16586055826526,-3.80284730797896,
15.4478487871275));
#62468=CARTESIAN_POINT('Ctrl Pts',(-6.16508040712673,-3.80093059948325,
15.4440549731565));
#62469=CARTESIAN_POINT('Ctrl Pts',(-6.15914772012249,-3.78635492174353,
15.415204780251));
#62470=CARTESIAN_POINT('Ctrl Pts',(-6.15373872498253,-3.77022241680086,
15.3866195641388));
#62471=CARTESIAN_POINT('Ctrl Pts',(-6.14892799956234,-3.75256704171994,
15.3585423290757));
#62472=CARTESIAN_POINT('Ctrl Pts',(-6.14417890446739,-3.73513785009647,
15.3308247921824));
#62473=CARTESIAN_POINT('Ctrl Pts',(-6.1400131210743,-3.71622457870713,15.3036031100997));
#62474=CARTESIAN_POINT('Ctrl Pts',(-6.13648912711731,-3.69590886727287,
15.2771119965196));
#62475=CARTESIAN_POINT('Ctrl Pts',(-6.13298582646184,-3.67571245205408,
15.2507764418331));
#62476=CARTESIAN_POINT('Ctrl Pts',(-6.13011701977104,-3.65413023060548,
15.2251637063787));
#62477=CARTESIAN_POINT('Ctrl Pts',(-6.12792325820837,-3.63128946871226,
15.2004932784671));
#62478=CARTESIAN_POINT('Ctrl Pts',(-6.12573694009297,-3.60852620567283,
15.1759065574781));
#62479=CARTESIAN_POINT('Ctrl Pts',(-6.12422123270962,-3.58451335694736,
15.1522565058577));
#62480=CARTESIAN_POINT('Ctrl Pts',(-6.12339673479099,-3.55941899377354,
15.1297376556406));
#62481=CARTESIAN_POINT('Ctrl Pts',(-6.12257297899932,-3.53434721792593,
15.1072390745419));
#62482=CARTESIAN_POINT('Ctrl Pts',(-6.12243923347756,-3.50819648918428,
15.0858702824523));
#62483=CARTESIAN_POINT('Ctrl Pts',(-6.12299510830259,-3.48116867719233,
15.0657922315937));
#62484=CARTESIAN_POINT('Ctrl Pts',(-6.12355369181233,-3.45400916321,15.045616343764));
#62485=CARTESIAN_POINT('Ctrl Pts',(-6.12480858945358,-3.42596474665878,
15.0267442829828));
#62486=CARTESIAN_POINT('Ctrl Pts',(-6.12673821499426,-3.39726457790098,
15.0092975879348));
#62487=CARTESIAN_POINT('Ctrl Pts',(-6.12867530627466,-3.36845336791503,
14.9917833914565));
#62488=CARTESIAN_POINT('Ctrl Pts',(-6.13129220496638,-3.33898216552069,
14.9757058503849));
#62489=CARTESIAN_POINT('Ctrl Pts',(-6.13454725450644,-3.30909513575427,
14.9611404987692));
#62490=CARTESIAN_POINT('Ctrl Pts',(-6.13783970378742,-3.27886471116188,
14.9464077947461));
#62491=CARTESIAN_POINT('Ctrl Pts',(-6.14178482931182,-3.24820971518353,
14.9332222789991));
#62492=CARTESIAN_POINT('Ctrl Pts',(-6.14632210404467,-3.21738239942496,
14.9216113893742));
#62493=CARTESIAN_POINT('Ctrl Pts',(-6.14962626908504,-3.19493312204694,
14.9131560284262));
#62494=CARTESIAN_POINT('Ctrl Pts',(-6.15324407131646,-3.17239248102998,
14.9055346078699));
#62495=CARTESIAN_POINT('Ctrl Pts',(-6.15714760202756,-3.14985391999966,
14.8987414182892));
#62496=CARTESIAN_POINT('Ctrl Pts',(-6.16260353328767,-3.11835196733577,
14.8892466357111));
#62497=CARTESIAN_POINT('Ctrl Pts',(-6.16861736085895,-3.08685531503858,
14.8813716106451));
#62498=CARTESIAN_POINT('Ctrl Pts',(-6.17510251310507,-3.05559890399993,
14.8750608827783));
#62499=CARTESIAN_POINT('Ctrl Pts',(-6.1817360245337,-3.02362744797641,14.8686057859913));
#62500=CARTESIAN_POINT('Ctrl Pts',(-6.18886232032284,-2.99190798960375,
14.8637868692114));
#62501=CARTESIAN_POINT('Ctrl Pts',(-6.1963828858837,-2.96065839512122,14.8605021501051));
#62502=CARTESIAN_POINT('Ctrl Pts',(-6.20401485935838,-2.92894587639438,
14.8571687719318));
#62503=CARTESIAN_POINT('Ctrl Pts',(-6.21205251543249,-2.89771762699749,
14.8554146667487));
#62504=CARTESIAN_POINT('Ctrl Pts',(-6.22039239040567,-2.86715933990464,
14.8550993693122));
#62505=CARTESIAN_POINT('Ctrl Pts',(-6.22893231697086,-2.83586804014653,
14.8547765087223));
#62506=CARTESIAN_POINT('Ctrl Pts',(-6.23778880583662,-2.8052794442995,14.8559615384475));
#62507=CARTESIAN_POINT('Ctrl Pts',(-6.24685554194399,-2.77554449068749,
14.8584798139296));
#62508=CARTESIAN_POINT('Ctrl Pts',(-6.24788307588537,-2.77217462597323,
14.858765210295));
#62509=CARTESIAN_POINT('Ctrl Pts',(-6.24891331808174,-2.76881567367841,
14.8590677131818));
#62510=CARTESIAN_POINT('Ctrl Pts',(-6.24994612027011,-2.76546781425246,
14.8593870565277));
#62511=CARTESIAN_POINT('',(-6.99999916823336,-3.16610397564684,14.5427478336087));
#62512=CARTESIAN_POINT('Ctrl Pts',(-6.99999900599707,-3.16610410860577,
14.542748444324));
#62513=CARTESIAN_POINT('Ctrl Pts',(-6.93510613246198,-3.10957084743748,
14.5767970301523));
#62514=CARTESIAN_POINT('Ctrl Pts',(-6.86717629266027,-3.05807923643768,
14.6100325970789));
#62515=CARTESIAN_POINT('Ctrl Pts',(-6.79616395204171,-3.01141659815692,
14.6426005706686));
#62516=CARTESIAN_POINT('Ctrl Pts',(-6.7879512091426,-3.00601995515295,14.6463671328112));
#62517=CARTESIAN_POINT('Ctrl Pts',(-6.77969723483539,-3.0006878852849,14.6501247109457));
#62518=CARTESIAN_POINT('Ctrl Pts',(-6.77140195753717,-2.99542004685623,
14.6538734876845));
#62519=CARTESIAN_POINT('Ctrl Pts',(-6.6913806973046,-2.9446032923814,14.6900364546582));
#62520=CARTESIAN_POINT('Ctrl Pts',(-6.60751418106424,-2.89976441230501,
14.7253809261968));
#62521=CARTESIAN_POINT('Ctrl Pts',(-6.52054164996745,-2.86132532829294,
14.7596579913119));
#62522=CARTESIAN_POINT('Ctrl Pts',(-6.44075323615254,-2.8260613949206,14.7911036974594));
#62523=CARTESIAN_POINT('Ctrl Pts',(-6.35835204191316,-2.79618437114786,
14.8216547520575));
#62524=CARTESIAN_POINT('Ctrl Pts',(-6.27305667611768,-2.77189333807855,
14.8513785255834));
#62525=CARTESIAN_POINT('Ctrl Pts',(-6.2653767150535,-2.76970618305036,14.8540548424176));
#62526=CARTESIAN_POINT('Ctrl Pts',(-6.25767328747102,-2.76756430839692,
14.8567244179092));
#62527=CARTESIAN_POINT('Ctrl Pts',(-6.24994618613909,-2.76546785592883,
14.8593872804758));
#62528=CARTESIAN_POINT('',(-7.000004116699,-4.92966193703766,14.7967990007598));
#62529=CARTESIAN_POINT('Ctrl Pts',(-7.000004116699,-4.92966193703766,14.7967990007598));
#62530=CARTESIAN_POINT('Ctrl Pts',(-7.,-4.84202472118207,14.7620803736131));
#62531=CARTESIAN_POINT('Ctrl Pts',(-7.,-4.69429463291145,14.707019515926));
#62532=CARTESIAN_POINT('Ctrl Pts',(-7.,-4.55642586372495,14.6619279529231));
#62533=CARTESIAN_POINT('Ctrl Pts',(-7.,-4.48005872682265,14.6386028054155));
#62534=CARTESIAN_POINT('Ctrl Pts',(-7.,-4.46232340867955,14.6333102630297));
#62535=CARTESIAN_POINT('Ctrl Pts',(-7.,-4.28372294397391,14.5814732655434));
#62536=CARTESIAN_POINT('Ctrl Pts',(-7.,-4.12833425220785,14.5473037835001));
#62537=CARTESIAN_POINT('Ctrl Pts',(-7.,-3.68749188829301,14.4827479384111));
#62538=CARTESIAN_POINT('Ctrl Pts',(-7.,-3.41573088208626,14.4884018589627));
#62539=CARTESIAN_POINT('Ctrl Pts',(-6.999998498703,-3.16610377894933,14.5427469301253));
#62540=CARTESIAN_POINT('Ctrl Pts',(-6.99999573616303,-4.92966193411623,
14.796799002087));
#62541=CARTESIAN_POINT('Ctrl Pts',(-7.00000221239064,-4.90604265398912,
14.8141315164145));
#62542=CARTESIAN_POINT('Ctrl Pts',(-6.9993066547385,-4.88279824389592,14.8313751281873));
#62543=CARTESIAN_POINT('Ctrl Pts',(-6.99796128285892,-4.85997235031371,
14.8484950322261));
#62544=CARTESIAN_POINT('Ctrl Pts',(-6.9957659811257,-4.82272634829462,14.876430323263));
#62545=CARTESIAN_POINT('Ctrl Pts',(-6.99184296717533,-4.78659534704214,
14.9040352250922));
#62546=CARTESIAN_POINT('Ctrl Pts',(-6.98646530326381,-4.75166688168638,
14.9311959838139));
#62547=CARTESIAN_POINT('Ctrl Pts',(-6.98080871742447,-4.71492679049211,
14.9597654827076));
#62548=CARTESIAN_POINT('Ctrl Pts',(-6.97354226261009,-4.67951736798576,
14.9878435992541));
#62549=CARTESIAN_POINT('Ctrl Pts',(-6.96494107209083,-4.64551155726207,
15.0153240744984));
#62550=CARTESIAN_POINT('Ctrl Pts',(-6.96162739700404,-4.63241055600544,
15.0259111398571));
#62551=CARTESIAN_POINT('Ctrl Pts',(-6.95811521673422,-4.6195175780179,15.0364097634807));
#62552=CARTESIAN_POINT('Ctrl Pts',(-6.95441888664791,-4.60683565951141,
15.0468148125601));
#62553=CARTESIAN_POINT('Ctrl Pts',(-6.94894998148114,-4.58807212702781,
15.0622096028904));
#62554=CARTESIAN_POINT('Ctrl Pts',(-6.94307818160796,-4.56977068691385,
15.0773994620523));
#62555=CARTESIAN_POINT('Ctrl Pts',(-6.93685437929836,-4.55193409922293,
15.0923701643997));
#62556=CARTESIAN_POINT('Ctrl Pts',(-6.92516109036544,-4.51842269203608,
15.1204971419883));
#62557=CARTESIAN_POINT('Ctrl Pts',(-6.91222767712603,-4.48655359241521,
15.1478491401164));
#62558=CARTESIAN_POINT('Ctrl Pts',(-6.89835605056547,-4.45632482916625,
15.1743509988416));
#62559=CARTESIAN_POINT('Ctrl Pts',(-6.88963414684376,-4.43731823599328,
15.1910142689519));
#62560=CARTESIAN_POINT('Ctrl Pts',(-6.88054042884793,-4.41895960534933,
15.2073419408165));
#62561=CARTESIAN_POINT('Ctrl Pts',(-6.87114205357841,-4.40124336406645,
15.2233198223925));
#62562=CARTESIAN_POINT('Ctrl Pts',(-6.86659238605382,-4.39266709366747,
15.2310545687537));
#62563=CARTESIAN_POINT('Ctrl Pts',(-6.86197124058544,-4.38424130608127,
15.2387073925565));
#62564=CARTESIAN_POINT('Ctrl Pts',(-6.85728579233503,-4.37596505290805,
15.2462769460957));
#62565=CARTESIAN_POINT('Ctrl Pts',(-6.84943500692511,-4.36209763101185,
15.2589602449625));
#62566=CARTESIAN_POINT('Ctrl Pts',(-6.84140385349202,-4.3486500597749,15.2714097024552));
#62567=CARTESIAN_POINT('Ctrl Pts',(-6.83322795534013,-4.33561341799617,
15.2836203187907));
#62568=CARTESIAN_POINT('Ctrl Pts',(-6.82670026643618,-4.32520488057279,
15.2933693522648));
#62569=CARTESIAN_POINT('Ctrl Pts',(-6.8200802521166,-4.31505827299739,15.3029661600629));
#62570=CARTESIAN_POINT('Ctrl Pts',(-6.81338485309185,-4.30516863997901,
15.312408702571));
#62571=CARTESIAN_POINT('Ctrl Pts',(-6.81003715357948,-4.30022382346981,
15.317129973825));
#62572=CARTESIAN_POINT('Ctrl Pts',(-6.80667060001253,-4.29534325631977,
15.3218126790656));
#62573=CARTESIAN_POINT('Ctrl Pts',(-6.80328720608736,-4.29052626895533,
15.3264566119654));
#62574=CARTESIAN_POINT('Ctrl Pts',(-6.80115374659458,-4.28748883150449,
15.3293849268315));
#62575=CARTESIAN_POINT('Ctrl Pts',(-6.79936460844594,-4.28496954309885,
15.3318215832851));
#62576=CARTESIAN_POINT('Ctrl Pts',(-6.79725830305816,-4.2820342222537,15.3346675785447));
#62577=CARTESIAN_POINT('Ctrl Pts',(-6.79602427745879,-4.28031449961219,
15.3363349678161));
#62578=CARTESIAN_POINT('Ctrl Pts',(-6.79468083205484,-4.27845241274624,
15.3381428279873));
#62579=CARTESIAN_POINT('Ctrl Pts',(-6.79308848615342,-4.27626539522726,
15.3402718894587));
#62580=CARTESIAN_POINT('Ctrl Pts',(-6.76811254009625,-4.24196202462714,
15.3736662194302));
#62581=CARTESIAN_POINT('Ctrl Pts',(-6.74136333482385,-4.20967407704942,
15.4063529011943));
#62582=CARTESIAN_POINT('Ctrl Pts',(-6.71310658826184,-4.17952400533597,
15.4382319962378));
#62583=CARTESIAN_POINT('Ctrl Pts',(-6.68059306941946,-4.14483193905004,
15.4749135566963));
#62584=CARTESIAN_POINT('Ctrl Pts',(-6.64608492528658,-4.11296986352685,
15.5105256057665));
#62585=CARTESIAN_POINT('Ctrl Pts',(-6.6100324935685,-4.08402521452437,15.5449441229869));
#62586=CARTESIAN_POINT('Ctrl Pts',(-6.58409154092629,-4.06319855365195,
15.5697094184935));
#62587=CARTESIAN_POINT('Ctrl Pts',(-6.55734985374155,-4.04388242560808,
15.5938572668279));
#62588=CARTESIAN_POINT('Ctrl Pts',(-6.52996021466892,-4.02610795854003,
15.617348183742));
#62589=CARTESIAN_POINT('Ctrl Pts',(-6.49082222870598,-4.00070941857521,
15.6509151531351));
#62590=CARTESIAN_POINT('Ctrl Pts',(-6.45036364595694,-3.9784582337298,15.6831400763665));
#62591=CARTESIAN_POINT('Ctrl Pts',(-6.40906282430625,-3.95933753692462,
15.7139351622328));
#62592=CARTESIAN_POINT('Ctrl Pts',(-6.37882678006827,-3.94533940779895,
15.736480030382));
#62593=CARTESIAN_POINT('Ctrl Pts',(-6.34813818136118,-3.9330192341771,15.7582589726189));
#62594=CARTESIAN_POINT('Ctrl Pts',(-6.3171683875425,-3.92236897336695,15.7792438726914));
#62595=CARTESIAN_POINT('Ctrl Pts',(-6.29947922520236,-3.91628581396529,
15.7912299164554));
#62596=CARTESIAN_POINT('Ctrl Pts',(-6.28169810243252,-3.91074736146905,
15.8029570173119));
#62597=CARTESIAN_POINT('Ctrl Pts',(-6.26385883869961,-3.90574397280168,
15.8144218264305));
#62598=CARTESIAN_POINT('Ctrl Pts',(-6.2226708194252,-3.9737511002187,14.5714076900287));
#62599=CARTESIAN_POINT('Ctrl Pts',(-6.22400636097445,-3.92718923052127,
14.9771467016005));
#62600=CARTESIAN_POINT('Ctrl Pts',(-6.2272659484764,-3.85976063408221,16.0460349316959));
#62601=CARTESIAN_POINT('Ctrl Pts',(-6.23205447278337,-3.98191121156329,
17.77942854308));
#62602=CARTESIAN_POINT('Ctrl Pts',(-6.2357082843596,-4.449905047104,19.7179590903193));
#62603=CARTESIAN_POINT('Ctrl Pts',(-6.23759745006902,-5.23225314551589,
21.5545919051479));
#62604=CARTESIAN_POINT('Ctrl Pts',(-6.23804464574047,-6.30682892892631,
23.2351575907732));
#62605=CARTESIAN_POINT('Ctrl Pts',(-6.23649779618595,-7.5400629509749,24.5993867713103));
#62606=CARTESIAN_POINT('Ctrl Pts',(-6.23491000958653,-8.44425820931118,
25.3447854154734));
#62607=CARTESIAN_POINT('Ctrl Pts',(-6.23413471759127,-8.85534285870587,
25.642104093556));
#62608=CARTESIAN_POINT('Ctrl Pts',(-6.71589153124125,-4.08566112089493,
14.5843363286704));
#62609=CARTESIAN_POINT('Ctrl Pts',(-6.71708025714564,-4.04021428388655,
14.9863212787434));
#62610=CARTESIAN_POINT('Ctrl Pts',(-6.71993478201462,-3.97507949372222,
16.045195140519));
#62611=CARTESIAN_POINT('Ctrl Pts',(-6.72416562750028,-4.09849404470664,
17.7615741310517));
#62612=CARTESIAN_POINT('Ctrl Pts',(-6.72736928264046,-4.56367891552375,
19.680427526418));
#62613=CARTESIAN_POINT('Ctrl Pts',(-6.72902533305614,-5.33903915516719,
21.4982065115222));
#62614=CARTESIAN_POINT('Ctrl Pts',(-6.72942032908318,-6.40303073142038,
23.1617848480856));
#62615=CARTESIAN_POINT('Ctrl Pts',(-6.72805279807952,-7.62318976665027,
24.5127338221719));
#62616=CARTESIAN_POINT('Ctrl Pts',(-6.72668452560022,-8.5179375479919,25.2513978787936));
#62617=CARTESIAN_POINT('Ctrl Pts',(-6.72599138112137,-8.92472608290391,
25.5460982756379));
#62618=CARTESIAN_POINT('Ctrl Pts',(-7.02184863765555,-4.48559734860376,
14.6305391207282));
#62619=CARTESIAN_POINT('Ctrl Pts',(-7.02249159491149,-4.44215217831574,
15.0188786224887));
#62620=CARTESIAN_POINT('Ctrl Pts',(-7.02397825402112,-4.38032190132887,
16.0419240163869));
#62621=CARTESIAN_POINT('Ctrl Pts',(-7.02622828780661,-4.50113493796852,
17.6995301397592));
#62622=CARTESIAN_POINT('Ctrl Pts',(-7.02790163053151,-4.95159591349138,
19.5522395072536));
#62623=CARTESIAN_POINT('Ctrl Pts',(-7.02876616760263,-5.70076950232316,
21.3070947338483));
#62624=CARTESIAN_POINT('Ctrl Pts',(-7.02897608662855,-6.72847789631824,
22.9136305902866));
#62625=CARTESIAN_POINT('Ctrl Pts',(-7.02824778608318,-7.90599710067593,
24.2181457116981));
#62626=CARTESIAN_POINT('Ctrl Pts',(-7.02756284280684,-8.7699326895579,24.9320738472432));
#62627=CARTESIAN_POINT('Ctrl Pts',(-7.02718415948163,-9.16263800955179,
25.2168992871523));
#62628=CARTESIAN_POINT('Ctrl Pts',(-6.99898915419192,-4.98714300774216,
14.6884801944114));
#62629=CARTESIAN_POINT('Ctrl Pts',(-6.99894179675862,-4.9456545700149,15.0596433930229));
#62630=CARTESIAN_POINT('Ctrl Pts',(-6.99873531351085,-4.8866027815796,16.0377464795711));
#62631=CARTESIAN_POINT('Ctrl Pts',(-6.99850468239117,-5.00216659736996,
17.6222150007892));
#62632=CARTESIAN_POINT('Ctrl Pts',(-6.99828080321693,-5.43285519889442,
19.3931412354428));
#62633=CARTESIAN_POINT('Ctrl Pts',(-6.99816433590801,-6.14885025059248,
21.0703293239026));
#62634=CARTESIAN_POINT('Ctrl Pts',(-6.99814256690665,-7.13148754762239,
22.6063533322588));
#62635=CARTESIAN_POINT('Ctrl Pts',(-6.9982154541888,-8.25667422537784,23.8529237825218));
#62636=CARTESIAN_POINT('Ctrl Pts',(-6.99835921786227,-9.08279282579766,
24.5356449639657));
#62637=CARTESIAN_POINT('Ctrl Pts',(-6.99838071869229,-9.4581913229097,24.807942025549));
#62638=CARTESIAN_POINT('',(-7.00000355772211,-9.33251602987223,24.7867164860314));
#62639=CARTESIAN_POINT('Ctrl Pts',(-7.00001601661652,-4.92966193654956,
14.796799000911));
#62640=CARTESIAN_POINT('Ctrl Pts',(-7.00002088999999,-4.90663940747915,
15.0161850414432));
#62641=CARTESIAN_POINT('Ctrl Pts',(-7.00001598308917,-4.89043247070465,
15.2342926627982));
#62642=CARTESIAN_POINT('Ctrl Pts',(-7.00000988156703,-4.8806944323136,15.4506299953074));
#62643=CARTESIAN_POINT('Ctrl Pts',(-7.00000652467011,-4.87533681985134,
15.569653102648));
#62644=CARTESIAN_POINT('Ctrl Pts',(-7.0000027909423,-4.87193735837233,15.6881412924022));
#62645=CARTESIAN_POINT('Ctrl Pts',(-6.99999999965555,-4.87043886014772,
15.8060193287844));
#62646=CARTESIAN_POINT('Ctrl Pts',(-6.9999945542241,-4.86751548822153,16.0359837936163));
#62647=CARTESIAN_POINT('Ctrl Pts',(-6.99999266080783,-4.87182625069152,
16.2636232331228));
#62648=CARTESIAN_POINT('Ctrl Pts',(-6.99999257345254,-4.88291897763752,
16.4885266234839));
#62649=CARTESIAN_POINT('Ctrl Pts',(-6.99999248483235,-4.89417232596976,
16.7166865885812));
#62650=CARTESIAN_POINT('Ctrl Pts',(-6.99999425319978,-4.91240544047496,
16.942030746898));
#62651=CARTESIAN_POINT('Ctrl Pts',(-6.99999619758638,-4.93715680472449,
17.1641828826339));
#62652=CARTESIAN_POINT('Ctrl Pts',(-6.99999754425264,-4.95429939706919,
17.3180436340265));
#62653=CARTESIAN_POINT('Ctrl Pts',(-6.99999897835612,-4.97456890745326,
17.4703743349893));
#62654=CARTESIAN_POINT('Ctrl Pts',(-6.99999998662336,-4.99781500190131,
17.621064298088));
#62655=CARTESIAN_POINT('Ctrl Pts',(-7.00000143709326,-5.0312562950098,17.83784338912));
#62656=CARTESIAN_POINT('Ctrl Pts',(-7.00000201442432,-5.07085616110269,
18.0512249470974));
#62657=CARTESIAN_POINT('Ctrl Pts',(-7.00000210876094,-5.11608689795626,
18.2609145834918));
#62658=CARTESIAN_POINT('Ctrl Pts',(-7.00000220461171,-5.16204361117133,
18.4739698453407));
#62659=CARTESIAN_POINT('Ctrl Pts',(-7.00000180216916,-5.21381338809911,
18.6832137767012));
#62660=CARTESIAN_POINT('Ctrl Pts',(-7.00000129011751,-5.27086637534113,
18.8883864605185));
#62661=CARTESIAN_POINT('Ctrl Pts',(-7.00000086166881,-5.31860429121544,
19.0600604918576));
#62662=CARTESIAN_POINT('Ctrl Pts',(-7.00000035619199,-5.37004149973613,
19.2288850931687));
#62663=CARTESIAN_POINT('Ctrl Pts',(-6.99999998816684,-5.42488007155213,
19.3947330695011));
#62664=CARTESIAN_POINT('Ctrl Pts',(-6.9999997037336,-5.46726280749537,19.5229109332719));
#62665=CARTESIAN_POINT('Ctrl Pts',(-6.99999950019787,-5.51167741653189,
19.6493113182398));
#62666=CARTESIAN_POINT('Ctrl Pts',(-6.99999936067318,-5.55798420403389,
19.7738901676013));
#62667=CARTESIAN_POINT('Ctrl Pts',(-6.99999924478743,-5.59644547559882,
19.8773622764436));
#62668=CARTESIAN_POINT('Ctrl Pts',(-6.99999917321303,-5.63621215991117,
19.9795779219696));
#62669=CARTESIAN_POINT('Ctrl Pts',(-6.99999913936352,-5.67720658690967,
20.0805154959337));
#62670=CARTESIAN_POINT('Ctrl Pts',(-6.99999912243876,-5.69770380040891,
20.1309842829157));
#62671=CARTESIAN_POINT('Ctrl Pts',(-6.99999911498658,-5.71850794957971,
20.1811335520072));
#62672=CARTESIAN_POINT('Ctrl Pts',(-6.99999911639991,-5.73960956221651,
20.2309609599606));
#62673=CARTESIAN_POINT('Ctrl Pts',(-6.99999911710658,-5.75016036853491,
20.2558746639373));
#62674=CARTESIAN_POINT('Ctrl Pts',(-6.99999912003183,-5.76078554071981,
20.2807079026295));
#62675=CARTESIAN_POINT('Ctrl Pts',(-6.99999912511198,-5.77148390107702,
20.3054603924112));
#62676=CARTESIAN_POINT('Ctrl Pts',(-6.99999912765206,-5.77683308125563,
20.3178366373021));
#62677=CARTESIAN_POINT('Ctrl Pts',(-6.99999913073098,-5.78220055847731,
20.3301926949653));
#62678=CARTESIAN_POINT('Ctrl Pts',(-6.99999913434149,-5.78758618636081,
20.3425285311915));
#62679=CARTESIAN_POINT('Ctrl Pts',(-6.9999991374978,-5.79229430622029,20.3533125282993));
#62680=CARTESIAN_POINT('Ctrl Pts',(-6.99999914056833,-5.79641054508912,
20.362704005978));
#62681=CARTESIAN_POINT('Ctrl Pts',(-6.99999914483362,-5.8015232358369,20.3743145323038));
#62682=CARTESIAN_POINT('Ctrl Pts',(-6.9999991454474,-5.80225896243464,20.3759853106577));
#62683=CARTESIAN_POINT('Ctrl Pts',(-6.99999914608787,-5.80301540258001,
20.3777020058122));
#62684=CARTESIAN_POINT('Ctrl Pts',(-6.99999914676096,-5.80379737586325,
20.3794753417173));
#62685=CARTESIAN_POINT('Ctrl Pts',(-6.99999923697272,-5.9086019813435,20.6171481291404));
#62686=CARTESIAN_POINT('Ctrl Pts',(-6.9999995214456,-6.02101207659238,20.8492773392419));
#62687=CARTESIAN_POINT('Ctrl Pts',(-6.9999999901846,-6.14041758229643,21.0754641373822));
#62688=CARTESIAN_POINT('Ctrl Pts',(-7.00000044364547,-6.25593116937927,
21.2942785735333));
#62689=CARTESIAN_POINT('Ctrl Pts',(-7.00000106797197,-6.37799088575244,
21.5075321997706));
#62690=CARTESIAN_POINT('Ctrl Pts',(-7.00000142593383,-6.50595763999341,
21.7149317398955));
#62691=CARTESIAN_POINT('Ctrl Pts',(-7.00000178765916,-6.63526978485192,
21.9245117947721));
#62692=CARTESIAN_POINT('Ctrl Pts',(-7.0000018762761,-6.77061383934092,22.128114062787));
#62693=CARTESIAN_POINT('Ctrl Pts',(-7.00000131559658,-6.9113633296045,22.3254778245801));
#62694=CARTESIAN_POINT('Ctrl Pts',(-7.00000103873753,-6.9808642997602,22.4229344682418));
#62695=CARTESIAN_POINT('Ctrl Pts',(-7.0000006048128,-7.05168378324631,22.5188706100842));
#62696=CARTESIAN_POINT('Ctrl Pts',(-6.99999997635844,-7.12374925579272,
22.6132585158635));
#62697=CARTESIAN_POINT('Ctrl Pts',(-6.99999887928061,-7.24955223556239,
22.7780292359001));
#62698=CARTESIAN_POINT('Ctrl Pts',(-6.99999719586419,-7.37915115146265,
22.938081068345));
#62699=CARTESIAN_POINT('Ctrl Pts',(-6.99999590263475,-7.51215861026573,
23.0933375004005));
#62700=CARTESIAN_POINT('Ctrl Pts',(-6.99999568171318,-7.53488019054777,
23.1198598587479));
#62701=CARTESIAN_POINT('Ctrl Pts',(-6.99999546002071,-7.55895205348164,
23.1476959584348));
#62702=CARTESIAN_POINT('Ctrl Pts',(-6.99999525388495,-7.58352667533906,
23.1758121710142));
#62703=CARTESIAN_POINT('Ctrl Pts',(-6.99999512029718,-7.59945243752027,
23.1940330867854));
#62704=CARTESIAN_POINT('Ctrl Pts',(-6.99999499323651,-7.61558858282698,
23.212372274829));
#62705=CARTESIAN_POINT('Ctrl Pts',(-6.99999487630705,-7.63169547194886,
23.2305561143529));
#62706=CARTESIAN_POINT('Ctrl Pts',(-6.99999457894682,-7.67265647511351,
23.2767989550805));
#62707=CARTESIAN_POINT('Ctrl Pts',(-6.99999434327586,-7.71387574907449,
23.3225495461325));
#62708=CARTESIAN_POINT('Ctrl Pts',(-6.99999419420493,-7.75533999032782,
23.3678081095132));
#62709=CARTESIAN_POINT('Ctrl Pts',(-6.9999936547506,-7.90538979191992,23.5315887130004));
#62710=CARTESIAN_POINT('Ctrl Pts',(-6.99999426200499,-8.05864834217112,
23.6889265209168));
#62711=CARTESIAN_POINT('Ctrl Pts',(-6.99999708872685,-8.21453766136163,
23.8398712965581));
#62712=CARTESIAN_POINT('Ctrl Pts',(-6.99999738651101,-8.23095999526624,
23.8557727420171));
#62713=CARTESIAN_POINT('Ctrl Pts',(-6.99999770877356,-8.24741156308034,
23.8716032672587));
#62714=CARTESIAN_POINT('Ctrl Pts',(-6.9999980566607,-8.26389171586799,23.8873629503283));
#62715=CARTESIAN_POINT('Ctrl Pts',(-6.99999863110429,-8.29110432907967,
23.91338589837));
#62716=CARTESIAN_POINT('Ctrl Pts',(-6.99999927542335,-8.3183948795832,23.939215688115));
#62717=CARTESIAN_POINT('Ctrl Pts',(-6.99999999465543,-8.3457604764835,23.9648526933387));
#62718=CARTESIAN_POINT('Ctrl Pts',(-7.00000393348348,-8.49562640279979,
24.1052520988337));
#62719=CARTESIAN_POINT('Ctrl Pts',(-7.00001006471687,-8.64773932553411,
24.2398676036782));
#62720=CARTESIAN_POINT('Ctrl Pts',(-7.00001375741759,-8.80155013567985,
24.3687621556948));
#62721=CARTESIAN_POINT('Ctrl Pts',(-7.00001750460692,-8.95763054129899,
24.4995586448479));
#62722=CARTESIAN_POINT('Ctrl Pts',(-7.00001874206943,-9.11545935639289,
24.624464169466));
#62723=CARTESIAN_POINT('Ctrl Pts',(-7.00001328591826,-9.27450984411414,
24.7435698673835));
#62724=CARTESIAN_POINT('Ctrl Pts',(-7.0000126232107,-9.29382821661489,24.7580365205343));
#62725=CARTESIAN_POINT('Ctrl Pts',(-7.00001186252235,-9.31316466773027,
24.7724176402076));
#62726=CARTESIAN_POINT('Ctrl Pts',(-7.00001099698708,-9.33251829944508,
24.786713413932));
#62727=CARTESIAN_POINT('',(-6.271594443024,-8.76071211955051,25.5608538793679));
#62728=CARTESIAN_POINT('Origin',(-5.99998362344619,-9.33252812839836,24.7867137519315));
#62729=CARTESIAN_POINT('Ctrl Pts',(-6.26386060032414,-3.90573753027274,
15.8144217558848));
#62730=CARTESIAN_POINT('Ctrl Pts',(-6.26455152175083,-3.90327936026393,
16.0555052700955));
#62731=CARTESIAN_POINT('Ctrl Pts',(-6.26520986012939,-3.9081043619149,16.2942816114619));
#62732=CARTESIAN_POINT('Ctrl Pts',(-6.26583561550458,-3.91978362271735,
16.5303239214902));
#62733=CARTESIAN_POINT('Ctrl Pts',(-6.26647067022013,-3.93163644882302,
16.769874052416));
#62734=CARTESIAN_POINT('Ctrl Pts',(-6.26707216630542,-3.95054874472424,
17.0066083324543));
#62735=CARTESIAN_POINT('Ctrl Pts',(-6.26764010380723,-3.97608047843518,
17.2401341043066));
#62736=CARTESIAN_POINT('Ctrl Pts',(-6.26812468823025,-3.99786505932561,
17.4393865767204));
#62737=CARTESIAN_POINT('Ctrl Pts',(-6.26858484164298,-4.02446879834471,
17.6363041707521));
#62738=CARTESIAN_POINT('Ctrl Pts',(-6.26902056407448,-4.05562321000105,
17.8306725463686));
#62739=CARTESIAN_POINT('Ctrl Pts',(-6.26953467329408,-4.09238232338637,
18.0600079367018));
#62740=CARTESIAN_POINT('Ctrl Pts',(-6.2700147705382,-4.13547525594668,18.2857935310089));
#62741=CARTESIAN_POINT('Ctrl Pts',(-6.27046085585454,-4.18435811903019,
18.5077389773028));
#62742=CARTESIAN_POINT('Ctrl Pts',(-6.27062083612231,-4.2018890559131,18.5873356163904));
#62743=CARTESIAN_POINT('Ctrl Pts',(-6.27077644189198,-4.22016489628043,
18.6664387862204));
#62744=CARTESIAN_POINT('Ctrl Pts',(-6.27092767316578,-4.23916129209173,
18.7450365386642));
#62745=CARTESIAN_POINT('Ctrl Pts',(-6.27136815335618,-4.29449069476137,
18.9739624221364));
#62746=CARTESIAN_POINT('Ctrl Pts',(-6.27177152290998,-4.3559308539005,19.1985968468994));
#62747=CARTESIAN_POINT('Ctrl Pts',(-6.27213778182718,-4.42289857364307,
19.418679912614));
#62748=CARTESIAN_POINT('Ctrl Pts',(-6.27250404074439,-4.48986629338564,
19.6387629783285));
#62749=CARTESIAN_POINT('Ctrl Pts',(-6.27283318902499,-4.56236163369194,
19.8542948916035));
#62750=CARTESIAN_POINT('Ctrl Pts',(-6.27312522666899,-4.6398280945072,20.0650658431881));
#62751=CARTESIAN_POINT('Ctrl Pts',(-6.27334041971111,-4.69691061009187,
20.2203761026475));
#62752=CARTESIAN_POINT('Ctrl Pts',(-6.27353526211499,-4.75658572964704,
20.372823953505));
#62753=CARTESIAN_POINT('Ctrl Pts',(-6.273709975537,-4.8187447529144,20.5226551291307));
#62754=CARTESIAN_POINT('Ctrl Pts',(-6.27388468895901,-4.88090377618176,
20.6724863047565));
#62755=CARTESIAN_POINT('Ctrl Pts',(-6.27403927339914,-4.94554697291618,
20.8197011373369));
#62756=CARTESIAN_POINT('Ctrl Pts',(-6.27417395051376,-5.01262254851192,
20.9645377631236));
#62757=CARTESIAN_POINT('Ctrl Pts',(-6.2742701358658,-5.06052740502531,21.0679789593351));
#62758=CARTESIAN_POINT('Ctrl Pts',(-6.27435616707685,-5.10967408453046,
21.1702069755043));
#62759=CARTESIAN_POINT('Ctrl Pts',(-6.27443212489378,-5.16004936933893,
21.2713099134374));
#62760=CARTESIAN_POINT('Ctrl Pts',(-6.27457884399237,-5.25735359261647,
21.4665989898976));
#62761=CARTESIAN_POINT('Ctrl Pts',(-6.27469165383684,-5.36122084707669,
21.6616529330288));
#62762=CARTESIAN_POINT('Ctrl Pts',(-6.27477055442719,-5.47186421246134,
21.8559699205302));
#62763=CARTESIAN_POINT('Ctrl Pts',(-6.27484862758721,-5.58134726110199,
22.0482491061854));
#62764=CARTESIAN_POINT('Ctrl Pts',(-6.27489349897643,-5.697465120118,22.239806792428));
#62765=CARTESIAN_POINT('Ctrl Pts',(-6.27490516859484,-5.82040639948584,
22.4301097733835));
#62766=CARTESIAN_POINT('Ctrl Pts',(-6.27491664462263,-5.94130817094473,
22.6172557639712));
#62767=CARTESIAN_POINT('Ctrl Pts',(-6.27489601132961,-6.06880890001566,
22.8031883574526));
#62768=CARTESIAN_POINT('Ctrl Pts',(-6.27484326871578,-6.20306971746703,
22.9873540527557));
#62769=CARTESIAN_POINT('Ctrl Pts',(-6.27479056618878,-6.33722849050585,
23.1713797736377));
#62770=CARTESIAN_POINT('Ctrl Pts',(-6.27470580313154,-6.4781371784492,23.3536414281399));
#62771=CARTESIAN_POINT('Ctrl Pts',(-6.27458897954408,-6.62593698870859,
23.5335386059839));
#62772=CARTESIAN_POINT('Ctrl Pts',(-6.27454781339659,-6.67801849828322,
23.5969305452151));
#62773=CARTESIAN_POINT('Ctrl Pts',(-6.27450266631469,-6.73095549786687,
23.6600284363159));
#62774=CARTESIAN_POINT('Ctrl Pts',(-6.2744535382863,-6.78475355160887,23.7228045291512));
#62775=CARTESIAN_POINT('Ctrl Pts',(-6.27431624073854,-6.9351023666132,23.8982441689131));
#62776=CARTESIAN_POINT('Ctrl Pts',(-6.27414785086344,-7.09217875388589,
24.0711732067128));
#62777=CARTESIAN_POINT('Ctrl Pts',(-6.27394836839685,-7.25599608303936,
24.2410353888947));
#62778=CARTESIAN_POINT('Ctrl Pts',(-6.27375072698655,-7.41830151528236,
24.4093298852295));
#62779=CARTESIAN_POINT('Ctrl Pts',(-6.27352256425359,-7.58722412006469,
24.5746139216277));
#62780=CARTESIAN_POINT('Ctrl Pts',(-6.27326387994108,-7.76274424252956,
24.7363078359475));
#62781=CARTESIAN_POINT('Ctrl Pts',(-6.27300884359698,-7.93578917870382,
24.8957215412841));
#62782=CARTESIAN_POINT('Ctrl Pts',(-6.27272414043476,-8.11524691732745,
25.05164567822));
#62783=CARTESIAN_POINT('Ctrl Pts',(-6.27240977020824,-8.30106579828263,
25.2034866126879));
#62784=CARTESIAN_POINT('Ctrl Pts',(-6.27215746706192,-8.45019788635873,
25.3253491247008));
#62785=CARTESIAN_POINT('Ctrl Pts',(-6.27188605495391,-8.60342667624941,
25.444580887195));
#62786=CARTESIAN_POINT('Ctrl Pts',(-6.27159553375696,-8.76070944735565,
25.5608567073969));
#62787=CARTESIAN_POINT('Origin',(-5.999994993365,-9.33250915082771,24.786719601394));
#62788=CARTESIAN_POINT('',(-5.98852246669791,-9.69456809148781,25.7188096068216));
#62789=CARTESIAN_POINT('Origin',(-5.999994993365,-9.33250915082771,24.786719601394));
#62790=CARTESIAN_POINT('Origin',(-6.,-9.33251101023518,24.7867243682986));
#62791=CARTESIAN_POINT('Ctrl Pts',(-5.98841833135407,-9.69410638613233,
25.7189877568217));
#62792=CARTESIAN_POINT('Ctrl Pts',(-5.98810627251156,-9.81679902707702,
25.6713270235229));
#62793=CARTESIAN_POINT('Ctrl Pts',(-5.9872640505419,-10.2439465987631,25.5029619509409));
#62794=CARTESIAN_POINT('Ctrl Pts',(-5.98726405054096,-10.7897532367295,
25.2768814390181));
#62795=CARTESIAN_POINT('Ctrl Pts',(-5.9881062725289,-11.2108442676179,25.0938945781174));
#62796=CARTESIAN_POINT('Ctrl Pts',(-5.98841833138675,-11.331302297366,25.0408390057578));
#62797=CARTESIAN_POINT('Ctrl Pts',(-6.5801963768428,-9.69658810056987,25.7253769392478));
#62798=CARTESIAN_POINT('Ctrl Pts',(-6.57988216944744,-9.81936870227868,
25.6778801647674));
#62799=CARTESIAN_POINT('Ctrl Pts',(-6.57903377815079,-10.246776088706,25.509948484126));
#62800=CARTESIAN_POINT('Ctrl Pts',(-6.57903377814996,-10.7926927101977,
25.2838224155365));
#62801=CARTESIAN_POINT('Ctrl Pts',(-6.57988216946375,-11.2136610034673,
25.1003453834807));
#62802=CARTESIAN_POINT('Ctrl Pts',(-6.58019637687482,-11.3340652944744,
25.0471116770712));
#62803=CARTESIAN_POINT('Ctrl Pts',(-7.00079677511913,-9.5458459940663,25.3372908855745));
#62804=CARTESIAN_POINT('Ctrl Pts',(-7.00061249046053,-9.66739287514854,
25.2904141399614));
#62805=CARTESIAN_POINT('Ctrl Pts',(-7.00011448997313,-10.0904742321413,
25.1245686165554));
#62806=CARTESIAN_POINT('Ctrl Pts',(-7.00011448997309,-10.6307100951158,
24.9007955951957));
#62807=CARTESIAN_POINT('Ctrl Pts',(-7.00061249047014,-11.0471442876849,
24.7189023919596));
#62808=CARTESIAN_POINT('Ctrl Pts',(-7.00079677513743,-11.166237779811,24.66610263116));
#62809=CARTESIAN_POINT('Ctrl Pts',(-6.99999917318234,-9.33157249891016,
24.7856430605173));
#62810=CARTESIAN_POINT('Ctrl Pts',(-6.99999957776342,-9.45129805339181,
24.7394735044865));
#62811=CARTESIAN_POINT('Ctrl Pts',(-7.00000004362102,-9.8680415619029,24.576125658625));
#62812=CARTESIAN_POINT('Ctrl Pts',(-7.00000004362183,-10.4001860098336,
24.3557042111086));
#62813=CARTESIAN_POINT('Ctrl Pts',(-6.99999957776368,-10.8103725420085,
24.1765264188007));
#62814=CARTESIAN_POINT('Ctrl Pts',(-6.99999917318159,-10.9276781031443,
24.1245144718731));
#62815=CARTESIAN_POINT('Origin',(-5.98852353414949,4.7522901968022,-11.4730434396584));
#62816=CARTESIAN_POINT('Origin',(-7.00021006966348,4.74293596854153,-11.4504602201464));
#62817=CARTESIAN_POINT('Ctrl Pts',(-6.05512388577107,-9.37217231939293,
25.8431943550442));
#62818=CARTESIAN_POINT('Ctrl Pts',(-4.03674925718073,-8.81555631688386,
26.0304372976439));
#62819=CARTESIAN_POINT('Ctrl Pts',(7.61020413204277E-7,-8.27057817080118,
26.2482647770642));
#62820=CARTESIAN_POINT('Ctrl Pts',(4.03675077922157,-8.81555652236587,26.0304372155136));
#62821=CARTESIAN_POINT('Ctrl Pts',(6.05512616883189,-9.37217294900257,25.8431941432457));
#62822=CARTESIAN_POINT('Ctrl Pts',(-6.05512388577107,-10.1400098573304,
25.5527871582871));
#62823=CARTESIAN_POINT('Ctrl Pts',(-4.03674925718073,-9.95059989273131,
25.6069155418854));
#62824=CARTESIAN_POINT('Ctrl Pts',(7.61020413204277E-7,-9.81341069027344,
25.7964954224481));
#62825=CARTESIAN_POINT('Ctrl Pts',(4.03675077922157,-9.95059994445685,25.6069154704024));
#62826=CARTESIAN_POINT('Ctrl Pts',(6.05512616883189,-10.1400100715769,25.5527870970548));
#62827=CARTESIAN_POINT('Ctrl Pts',(-6.05512388577107,-10.8990877228837,
25.2383593897359));
#62828=CARTESIAN_POINT('Ctrl Pts',(-4.03674925718073,-11.0715845951584,
25.1425759551505));
#62829=CARTESIAN_POINT('Ctrl Pts',(7.61020413651836E-7,-11.3029258412939,
25.1794677576838));
#62830=CARTESIAN_POINT('Ctrl Pts',(4.03675077922157,-11.0715845079327,25.1425759412421));
#62831=CARTESIAN_POINT('Ctrl Pts',(6.05512616883189,-10.8990875277674,25.238359498084));
#62832=CARTESIAN_POINT('Ctrl Pts',(-6.05512388577107,-11.6473739575525,
24.9007527141814));
#62833=CARTESIAN_POINT('Ctrl Pts',(-4.03674925718073,-12.1736465516541,
24.6394332194205));
#62834=CARTESIAN_POINT('Ctrl Pts',(7.61020413651836E-7,-12.7132798561856,
24.4078866218257));
#62835=CARTESIAN_POINT('Ctrl Pts',(4.03675077922157,-12.1736463481894,24.639433306728));
#62836=CARTESIAN_POINT('Ctrl Pts',(6.05512616883189,-11.6473733622648,24.9007530097704));
#62837=CARTESIAN_POINT('Ctrl Pts',(-5.98852262888646,-9.69456765092853,
25.7188097475992));
#62838=CARTESIAN_POINT('Ctrl Pts',(-5.93898436053355,-9.67817087502701,
25.7245691049754));
#62839=CARTESIAN_POINT('Ctrl Pts',(-5.88247527727907,-9.65963316949226,
25.7310995806593));
#62840=CARTESIAN_POINT('Ctrl Pts',(-5.81892446422276,-9.63914044126316,
25.7383491666606));
#62841=CARTESIAN_POINT('Ctrl Pts',(-5.75779203952735,-9.61942755160809,
25.745322873982));
#62842=CARTESIAN_POINT('Ctrl Pts',(-5.69014336124076,-9.59790579669414,
25.7529620583438));
#62843=CARTESIAN_POINT('Ctrl Pts',(-5.61590486620461,-9.57478231219134,
25.7612053328932));
#62844=CARTESIAN_POINT('Ctrl Pts',(-5.54019770411008,-9.55120137364199,
25.7696116849104));
#62845=CARTESIAN_POINT('Ctrl Pts',(-5.45763719809451,-9.52595445950312,
25.7786465156618));
#62846=CARTESIAN_POINT('Ctrl Pts',(-5.36813769574401,-9.49930636707747,
25.7882262167553));
#62847=CARTESIAN_POINT('Ctrl Pts',(-5.32338794456876,-9.48598232086465,
25.7930160673021));
#62848=CARTESIAN_POINT('Ctrl Pts',(-5.2769033461206,-9.47230870126358,25.7979418256434));
#62849=CARTESIAN_POINT('Ctrl Pts',(-5.2286727814214,-9.45832303024694,25.8029910315361));
#62850=CARTESIAN_POINT('Ctrl Pts',(-5.20455749907179,-9.45133019473862,
25.8055156344824));
#62851=CARTESIAN_POINT('Ctrl Pts',(-5.18000572518015,-9.44425934494013,
25.808071095541));
#62852=CARTESIAN_POINT('Ctrl Pts',(-5.15501605465378,-9.43711552411567,
25.8106556929332));
#62853=CARTESIAN_POINT('Ctrl Pts',(-5.13002638412742,-9.4299717032912,25.8132402903255));
#62854=CARTESIAN_POINT('Ctrl Pts',(-5.10342519951994,-9.42242436287353,
25.8159738674462));
#62855=CARTESIAN_POINT('Ctrl Pts',(-5.07873195594013,-9.41547021113734,
25.8184951418982));
#62856=CARTESIAN_POINT('Ctrl Pts',(-5.06392831161827,-9.41130118455604,
25.8200066505059));
#62857=CARTESIAN_POINT('Ctrl Pts',(-5.04923287210674,-9.40718159317273,
25.8215011286591));
#62858=CARTESIAN_POINT('Ctrl Pts',(-5.03464595226408,-9.40311067339794,
25.8229787770826));
#62859=CARTESIAN_POINT('Ctrl Pts',(-4.9173131829933,-9.37036542657352,25.8348645338705));
#62860=CARTESIAN_POINT('Ctrl Pts',(-4.80700429114233,-9.3407658895739,25.8456618845693));
#62861=CARTESIAN_POINT('Ctrl Pts',(-4.70385804214751,-9.31394075329404,
25.8554800114032));
#62862=CARTESIAN_POINT('Ctrl Pts',(-4.60105414252729,-9.28720465145526,
25.8652655512102));
#62863=CARTESIAN_POINT('Ctrl Pts',(-4.50536510919138,-9.26322438846416,
25.8740785601528));
#62864=CARTESIAN_POINT('Ctrl Pts',(-4.41690034486915,-9.24167510219215,
25.8820193538411));
#62865=CARTESIAN_POINT('Ctrl Pts',(-4.3842827801574,-9.2337297327012,25.8849471788794));
#62866=CARTESIAN_POINT('Ctrl Pts',(-4.35264706504086,-9.22611527434213,
25.88775633941));
#62867=CARTESIAN_POINT('Ctrl Pts',(-4.32199784036469,-9.21881698675232,
25.8904515152313));
#62868=CARTESIAN_POINT('Ctrl Pts',(-4.28740661835289,-9.21058001864,25.8934933352506));
#62869=CARTESIAN_POINT('Ctrl Pts',(-4.25407197310449,-9.20274575444108,
25.8963899723563));
#62870=CARTESIAN_POINT('Ctrl Pts',(-4.22199993581219,-9.19529432826471,
25.8991478200083));
#62871=CARTESIAN_POINT('Ctrl Pts',(-4.20596391716604,-9.19156861517652,
25.9005267438343));
#62872=CARTESIAN_POINT('Ctrl Pts',(-4.19024355050934,-9.18793861239127,
25.9018709724553));
#62873=CARTESIAN_POINT('Ctrl Pts',(-4.17483951758381,-9.18440199481933,
25.9031812605705));
#62874=CARTESIAN_POINT('Ctrl Pts',(-4.16713750112104,-9.18263368603336,
25.903836404628));
#62875=CARTESIAN_POINT('Ctrl Pts',(-4.15951456809107,-9.1808887235961,25.9044830636818));
#62876=CARTESIAN_POINT('Ctrl Pts',(-4.15197080194161,-9.17916682159851,
25.9051213311328));
#62877=CARTESIAN_POINT('Ctrl Pts',(-4.14819891886689,-9.17830587059972,
25.9054404648582));
#62878=CARTESIAN_POINT('Ctrl Pts',(-4.1444468275123,-9.1774506847135,25.9057575006902));
#62879=CARTESIAN_POINT('Ctrl Pts',(-4.1407145380735,-9.17660122874452,25.9060724501517));
#62880=CARTESIAN_POINT('Ctrl Pts',(-4.13884839335409,-9.17617650076003,
25.9062299248824));
#62881=CARTESIAN_POINT('Ctrl Pts',(-4.13698719911364,-9.17575320525501,
25.906386878021));
#62882=CARTESIAN_POINT('Ctrl Pts',(-4.13513095661149,-9.17533133786587,
25.9065433109975));
#62883=CARTESIAN_POINT('Ctrl Pts',(-4.13327471410933,-9.17490947047673,
25.9066997439741));
#62884=CARTESIAN_POINT('Ctrl Pts',(-4.13318162789786,-9.17488804538954,
25.906707680303));
#62885=CARTESIAN_POINT('Ctrl Pts',(-4.12957708557479,-9.17407001569364,
25.907011050869));
#62886=CARTESIAN_POINT('Ctrl Pts',(-4.08632512252271,-9.16425423687577,
25.9106512834799));
#62887=CARTESIAN_POINT('Ctrl Pts',(-4.04419451593996,-9.15484676570599,
25.9141451442275));
#62888=CARTESIAN_POINT('Ctrl Pts',(-4.00319215047733,-9.14582510012115,
25.9174997768095));
#62889=CARTESIAN_POINT('Ctrl Pts',(-3.90003901700451,-9.12312852972282,
25.9259393109333));
#62890=CARTESIAN_POINT('Ctrl Pts',(-3.80402833489472,-9.10287062112949,
25.9334985127824));
#62891=CARTESIAN_POINT('Ctrl Pts',(-3.71525318357639,-9.08472321242478,
25.9402858927437));
#62892=CARTESIAN_POINT('Ctrl Pts',(-3.62699494431028,-9.06668147083678,
25.9470337517529));
#62893=CARTESIAN_POINT('Ctrl Pts',(-3.54588795407541,-9.05072561884383,
25.9530188688104));
#62894=CARTESIAN_POINT('Ctrl Pts',(-3.4720030082679,-9.0365784472142,25.9583351550519));
#62895=CARTESIAN_POINT('Ctrl Pts',(-3.41340786055448,-9.02535890035922,
25.9625512856074));
#62896=CARTESIAN_POINT('Ctrl Pts',(-3.35935453569501,-9.01527776895949,
25.9663465298263));
#62897=CARTESIAN_POINT('Ctrl Pts',(-3.3098705527171,-9.00621781931329,25.9697613075137));
#62898=CARTESIAN_POINT('Ctrl Pts',(-3.27660567797744,-9.00012740233405,
25.9720568412441));
#62899=CARTESIAN_POINT('Ctrl Pts',(-3.24540555097381,-8.99449884385767,
25.9741803228472));
#62900=CARTESIAN_POINT('Ctrl Pts',(-3.21627699481478,-8.98930142713313,
25.9761424569287));
#62901=CARTESIAN_POINT('Ctrl Pts',(-3.20171271673527,-8.98670271877085,
25.9771235239694));
#62902=CARTESIAN_POINT('Ctrl Pts',(-3.18766633137259,-8.98421179646901,
25.9780642558627));
#62903=CARTESIAN_POINT('Ctrl Pts',(-3.17413856470909,-8.9818252665669,25.978965841365));
#62904=CARTESIAN_POINT('Ctrl Pts',(-3.16737468137735,-8.98063200161584,
25.9794166341161));
#62905=CARTESIAN_POINT('Ctrl Pts',(-3.16074045272067,-8.97946483479674,
25.9798576403585));
#62906=CARTESIAN_POINT('Ctrl Pts',(-3.15423596653136,-8.97832335474324,
25.9802890046405));
#62907=CARTESIAN_POINT('Ctrl Pts',(-3.15098372343671,-8.97775261471649,
25.9805046867815));
#62908=CARTESIAN_POINT('Ctrl Pts',(-3.14776391595891,-8.97718829638282,
25.9807179584371));
#62909=CARTESIAN_POINT('Ctrl Pts',(-3.14457655464353,-8.97663034991889,
25.9809288371351));
#62910=CARTESIAN_POINT('Ctrl Pts',(-3.14138919332815,-8.97607240345496,
25.9811397158331));
#62911=CARTESIAN_POINT('Ctrl Pts',(-3.13654159639592,-8.97522524816651,
25.9814599337183));
#62912=CARTESIAN_POINT('Ctrl Pts',(-3.13511181960606,-8.97497557679973,
25.9815543117296));
#62913=CARTESIAN_POINT('Ctrl Pts',(-3.11926201300701,-8.97220784207018,
25.98260054023));
#62914=CARTESIAN_POINT('Ctrl Pts',(-3.09633139320336,-8.96820454104232,
25.9841138922302));
#62915=CARTESIAN_POINT('Ctrl Pts',(-3.06630403421781,-8.96304322994323,
25.986066638726));
#62916=CARTESIAN_POINT('Ctrl Pts',(-3.0363918420494,-8.95790171451689,25.9880118956654));
#62917=CARTESIAN_POINT('Ctrl Pts',(-2.99943716317865,-8.951611038267,25.9903932118209));
#62918=CARTESIAN_POINT('Ctrl Pts',(-2.95541545647122,-8.94429571968719,
25.9931657462656));
#62919=CARTESIAN_POINT('Ctrl Pts',(-2.93782840563912,-8.94137318693372,
25.9942733976462));
#62920=CARTESIAN_POINT('Ctrl Pts',(-2.91911331508352,-8.93828765186099,
25.9954432923733));
#62921=CARTESIAN_POINT('Ctrl Pts',(-2.89926827636051,-8.93504921567418,
25.9966717693497));
#62922=CARTESIAN_POINT('Ctrl Pts',(-2.84975151646082,-8.92696876446665,
25.9997370291525));
#62923=CARTESIAN_POINT('Ctrl Pts',(-2.79320020456681,-8.91793299536115,
26.0031682944269));
#62924=CARTESIAN_POINT('Ctrl Pts',(-2.72958061231902,-8.90813227349094,
26.0068961507412));
#62925=CARTESIAN_POINT('Ctrl Pts',(-2.66637937430061,-8.8983959999031,26.0105994931533));
#62926=CARTESIAN_POINT('Ctrl Pts',(-2.5962023367641,-8.88790478805659,26.0145955811916));
#62927=CARTESIAN_POINT('Ctrl Pts',(-2.51901249338794,-8.87689297298689,
26.018797979586));
#62928=CARTESIAN_POINT('Ctrl Pts',(-2.46596176830785,-8.86932481701785,
26.0216861870514));
#62929=CARTESIAN_POINT('Ctrl Pts',(-2.40959846992732,-8.86151174051651,
26.0246714661818));
#62930=CARTESIAN_POINT('Ctrl Pts',(-2.34991019551084,-8.85354310269698,
26.0277204859783));
#62931=CARTESIAN_POINT('Ctrl Pts',(-2.31814365623095,-8.84930213495624,
26.0293431967717));
#62932=CARTESIAN_POINT('Ctrl Pts',(-2.2854353336339,-8.8450172898929,26.030983887705));
#62933=CARTESIAN_POINT('Ctrl Pts',(-2.25178337805218,-8.840703317834,26.0326370147983));
#62934=CARTESIAN_POINT('Ctrl Pts',(-2.23495740026131,-8.83854633180455,
26.0334635783449));
#62935=CARTESIAN_POINT('Ctrl Pts',(-2.21789551422063,-8.83638206375512,
26.0342932501494));
#62936=CARTESIAN_POINT('Ctrl Pts',(-2.20059749295585,-8.83421245826841,
26.0351252967679));
#62937=CARTESIAN_POINT('Ctrl Pts',(-2.19194848232346,-8.83312765552505,
26.0355413200772));
#62938=CARTESIAN_POINT('Ctrl Pts',(-2.1832404378848,-8.83204151840427,26.0359579370378));
#62939=CARTESIAN_POINT('Ctrl Pts',(-2.17447333152382,-8.83095429277892,
26.0363750546369));
#62940=CARTESIAN_POINT('Ctrl Pts',(-2.16789800175309,-8.83013887355991,
26.0366878928362));
#62941=CARTESIAN_POINT('Ctrl Pts',(-2.16128944965104,-8.82932284205554,
26.0370010126402));
#62942=CARTESIAN_POINT('Ctrl Pts',(-2.1546476634258,-8.82850630317931,26.037314374306));
#62943=CARTESIAN_POINT('Ctrl Pts',(-2.15243373468405,-8.8282341235539,26.0374188281946));
#62944=CARTESIAN_POINT('Ctrl Pts',(-2.14891110169832,-8.827801919456,26.0375847057948));
#62945=CARTESIAN_POINT('Ctrl Pts',(-2.14799479872992,-8.82768959917277,
26.037627815079));
#62946=CARTESIAN_POINT('Ctrl Pts',(-2.01247654850243,-8.81107779197115,
26.0440035390174));
#62947=CARTESIAN_POINT('Ctrl Pts',(-1.87292257322361,-8.79561898355788,
26.0499626459348));
#62948=CARTESIAN_POINT('Ctrl Pts',(-1.72934633996503,-8.78158412302116,
26.0553978387469));
#62949=CARTESIAN_POINT('Ctrl Pts',(-1.55028977293231,-8.76408098974171,
26.0621761678897));
#62950=CARTESIAN_POINT('Ctrl Pts',(-1.36497648425363,-8.74879217455378,
26.0681404534892));
#62951=CARTESIAN_POINT('Ctrl Pts',(-1.17345041796963,-8.73624782919835,
26.0730613254694));
#62952=CARTESIAN_POINT('Ctrl Pts',(-0.994937122853128,-8.72455577877448,
26.0776478608119));
#62953=CARTESIAN_POINT('Ctrl Pts',(-0.811026655105664,-8.71524826294544,
26.0813278035741));
#62954=CARTESIAN_POINT('Ctrl Pts',(-0.621779446010509,-8.70877956174966,
26.0838948793462));
#62955=CARTESIAN_POINT('Ctrl Pts',(-0.437414705199804,-8.70247774929471,
26.0863957260516));
#62956=CARTESIAN_POINT('Ctrl Pts',(-0.247983386096974,-8.69887045341315,
26.0878397960718));
#62957=CARTESIAN_POINT('Ctrl Pts',(-0.0536310989065854,-8.69839216830185,
26.0880416703161));
#62958=CARTESIAN_POINT('Ctrl Pts',(0.0580839165268676,-8.69811724676959,
26.0881577090036));
#62959=CARTESIAN_POINT('Ctrl Pts',(0.171424025792903,-8.69887651459616,
26.087863092153));
#62960=CARTESIAN_POINT('Ctrl Pts',(0.286354490943671,-8.70075531922724,
26.0871207012052));
#62961=CARTESIAN_POINT('Ctrl Pts',(0.308564744031445,-8.70111839725276,
26.0869772345376));
#62962=CARTESIAN_POINT('Ctrl Pts',(0.330834373102222,-8.70152329087806,
26.0868170413609));
#62963=CARTESIAN_POINT('Ctrl Pts',(0.353163103461588,-8.70197062504175,
26.0866398476152));
#62964=CARTESIAN_POINT('Ctrl Pts',(0.484464472008564,-8.70460111889181,
26.0855978814603));
#62965=CARTESIAN_POINT('Ctrl Pts',(0.617809998392041,-8.70869875543607,
26.0839680017488));
#62966=CARTESIAN_POINT('Ctrl Pts',(0.753157416662829,-8.71440146455451,
26.0817096126577));
#62967=CARTESIAN_POINT('Ctrl Pts',(0.832339520725286,-8.7177377122098,26.0803883905589));
#62968=CARTESIAN_POINT('Ctrl Pts',(0.912206730531842,-8.72162325745983,
26.0788521144128));
#62969=CARTESIAN_POINT('Ctrl Pts',(0.992749474308896,-8.72608667555154,
26.0770927025014));
#62970=CARTESIAN_POINT('Ctrl Pts',(1.03302084619742,-8.7283183845974,26.0762129965457));
#62971=CARTESIAN_POINT('Ctrl Pts',(1.07346110157823,-8.73069456314185,26.0752775105416));
#62972=CARTESIAN_POINT('Ctrl Pts',(1.11406896962032,-8.73321881095825,26.0742852517176));
#62973=CARTESIAN_POINT('Ctrl Pts',(1.13437290364137,-8.73448093486644,26.0737891223056));
#62974=CARTESIAN_POINT('Ctrl Pts',(1.1547187408289,-8.73578007617861,26.0732787999421));
#62975=CARTESIAN_POINT('Ctrl Pts',(1.17510631899125,-8.73711668864689,26.0727541609786));
#62976=CARTESIAN_POINT('Ctrl Pts',(1.18530010807242,-8.73778499488104,26.0724918414968));
#62977=CARTESIAN_POINT('Ctrl Pts',(1.19550433239735,-8.73846266890964,26.0722259428812));
#62978=CARTESIAN_POINT('Ctrl Pts',(1.20571897138345,-8.73914976768477,26.0719564497065));
#62979=CARTESIAN_POINT('Ctrl Pts',(1.20976726658234,-8.73942208065406,26.0718496433939));
#62980=CARTESIAN_POINT('Ctrl Pts',(1.21381719763114,-8.73969587397374,26.071742272482));
#62981=CARTESIAN_POINT('Ctrl Pts',(1.21786876323936,-8.73997115120274,26.0716343360093));
#62982=CARTESIAN_POINT('Ctrl Pts',(1.21892864306473,-8.74004316306423,26.0716061000875));
#62983=CARTESIAN_POINT('Ctrl Pts',(1.21998863474838,-8.74011527647456,26.0715778254625));
#62984=CARTESIAN_POINT('Ctrl Pts',(1.22104873826724,-8.7401874914914,26.0715495121158));
#62985=CARTESIAN_POINT('Ctrl Pts',(1.22360500038343,-8.74036162591175,26.0714812392215));
#62986=CARTESIAN_POINT('Ctrl Pts',(1.22616191276806,-8.74053635114404,26.0714127411729));
#62987=CARTESIAN_POINT('Ctrl Pts',(1.2287194750979,-8.74071166796458,26.0713440177222));
#62988=CARTESIAN_POINT('Ctrl Pts',(1.23127703742774,-8.74088698478512,26.0712752942715));
#62989=CARTESIAN_POINT('Ctrl Pts',(1.23521161045926,-8.74115782948028,26.0711691378197));
#62990=CARTESIAN_POINT('Ctrl Pts',(1.23639411159791,-8.74123939403498,26.0711371708931));
#62991=CARTESIAN_POINT('Ctrl Pts',(1.30374576804469,-8.74588506217585,26.0693164323025));
#62992=CARTESIAN_POINT('Ctrl Pts',(1.37824680873525,-8.75142078003761,26.0671523857232));
#62993=CARTESIAN_POINT('Ctrl Pts',(1.45986555292161,-8.75810195128712,26.0645490720026));
#62994=CARTESIAN_POINT('Ctrl Pts',(1.54153671708015,-8.76478741354618,26.0619440862932));
#62995=CARTESIAN_POINT('Ctrl Pts',(1.63033495238198,-8.7726198465256,26.0588991994326));
#62996=CARTESIAN_POINT('Ctrl Pts',(1.72621529430777,-8.78190290107649,26.0553019027112));
#62997=CARTESIAN_POINT('Ctrl Pts',(1.81098051183597,-8.79010979857526,26.0521216299568));
#62998=CARTESIAN_POINT('Ctrl Pts',(1.9012809281609,-8.79945118708362,26.0485093304685));
#62999=CARTESIAN_POINT('Ctrl Pts',(1.99707461557457,-8.81016746024439,26.0443773365715));
#63000=CARTESIAN_POINT('Ctrl Pts',(2.10637322501788,-8.82239450553838,26.0396628172816));
#63001=CARTESIAN_POINT('Ctrl Pts',(2.22282381531433,-8.83641075654679,26.0342718356153));
#63002=CARTESIAN_POINT('Ctrl Pts',(2.34634426221008,-8.85261426659337,26.0280625761146));
#63003=CARTESIAN_POINT('Ctrl Pts',(2.4625641280895,-8.86786008064049,26.0222203101212));
#63004=CARTESIAN_POINT('Ctrl Pts',(2.58504288732567,-8.88504271884099,26.0156534249642));
#63005=CARTESIAN_POINT('Ctrl Pts',(2.71369126659325,-8.90452916042472,26.0082345163188));
#63006=CARTESIAN_POINT('Ctrl Pts',(2.74242434444493,-8.90888137571313,26.0065775340785));
#63007=CARTESIAN_POINT('Ctrl Pts',(2.77146509461616,-8.91334864511851,26.0048780180626));
#63008=CARTESIAN_POINT('Ctrl Pts',(2.80081237645999,-8.91793523390627,26.0031345111935));
#63009=CARTESIAN_POINT('Ctrl Pts',(2.82623497984273,-8.92190844778861,26.0016241674464));
#63010=CARTESIAN_POINT('Ctrl Pts',(2.85468152296542,-8.92641169081457,25.9999134386759));
#63011=CARTESIAN_POINT('Ctrl Pts',(2.88336004684574,-8.93102387982404,25.9981627588254));
#63012=CARTESIAN_POINT('Ctrl Pts',(2.89852589836326,-8.93346290960048,25.9972369597578));
#63013=CARTESIAN_POINT('Ctrl Pts',(2.91375676620661,-8.93593162566564,25.9963002705621));
#63014=CARTESIAN_POINT('Ctrl Pts',(2.92864080883696,-8.93836217409121,25.9953784262594));
#63015=CARTESIAN_POINT('Ctrl Pts',(3.02398869251615,-8.95393238269068,25.9894730478935));
#63016=CARTESIAN_POINT('Ctrl Pts',(3.11236106131741,-8.96910574908508,25.98373320408));
#63017=CARTESIAN_POINT('Ctrl Pts',(3.19380697504853,-8.98358951228705,25.9782657807705));
#63018=CARTESIAN_POINT('Ctrl Pts',(3.25102861306154,-8.9937654022371,25.9744245209313));
#63019=CARTESIAN_POINT('Ctrl Pts',(3.30483132057741,-9.00360193840428,25.9707173021471));
#63020=CARTESIAN_POINT('Ctrl Pts',(3.3552315455841,-9.01301185398277,25.967175534456));
#63021=CARTESIAN_POINT('Ctrl Pts',(3.42777143265541,-9.02655532949947,25.9620779495085));
#63022=CARTESIAN_POINT('Ctrl Pts',(3.49326333427343,-9.03921296686623,25.9573238865908));
#63023=CARTESIAN_POINT('Ctrl Pts',(3.55175248027868,-9.05076599743781,25.9529912121744));
#63024=CARTESIAN_POINT('Ctrl Pts',(3.61052885977499,-9.06237576361814,25.9486372604906));
#63025=CARTESIAN_POINT('Ctrl Pts',(3.66223368766563,-9.07287010118517,25.9447087798008));
#63026=CARTESIAN_POINT('Ctrl Pts',(3.70690581587701,-9.08207595684254,25.9412664733879));
#63027=CARTESIAN_POINT('Ctrl Pts',(3.7518036529799,-9.09132832569636,25.9378067744935));
#63028=CARTESIAN_POINT('Ctrl Pts',(3.7895976665208,-9.09927919185978,25.9348381263405));
#63029=CARTESIAN_POINT('Ctrl Pts',(3.82031812519521,-9.10580154271587,25.9324045714528));
#63030=CARTESIAN_POINT('Ctrl Pts',(3.82672446119443,-9.10716169073748,25.9318970865077));
#63031=CARTESIAN_POINT('Ctrl Pts',(3.83282315114527,-9.10845988334454,25.9314128120963));
#63032=CARTESIAN_POINT('Ctrl Pts',(3.83861441268323,-9.10969523198207,25.9309520546069));
#63033=CARTESIAN_POINT('Ctrl Pts',(3.85088587684816,-9.11231288902232,25.9299757269135));
#63034=CARTESIAN_POINT('Ctrl Pts',(3.86177701482641,-9.11464825921153,25.9291050310371));
#63035=CARTESIAN_POINT('Ctrl Pts',(3.87128958500804,-9.11669424188912,25.9283424094287));
#63036=CARTESIAN_POINT('Ctrl Pts',(3.87604587009886,-9.11771723322791,25.9279610986245));
#63037=CARTESIAN_POINT('Ctrl Pts',(3.88045751324117,-9.11866787784305,25.9276068068093));
#63038=CARTESIAN_POINT('Ctrl Pts',(3.8845246859424,-9.11954549169954,25.9272797680479));
#63039=CARTESIAN_POINT('Ctrl Pts',(3.88655827229301,-9.11998429862778,25.9271162486671));
#63040=CARTESIAN_POINT('Ctrl Pts',(3.88850574103339,-9.12040484787707,25.9269595425791));
#63041=CARTESIAN_POINT('Ctrl Pts',(3.89036711217908,-9.12080705957815,25.9268096771908));
#63042=CARTESIAN_POINT('Ctrl Pts',(3.89129779775192,-9.12100816542869,25.9267347444967));
#63043=CARTESIAN_POINT('Ctrl Pts',(3.8922069589261,-9.12120468689288,25.9266615219794));
#63044=CARTESIAN_POINT('Ctrl Pts',(3.89309459803728,-9.12139661467507,25.926590012827));
#63045=CARTESIAN_POINT('Ctrl Pts',(3.89353841759287,-9.12149257856616,25.9265542582508));
#63046=CARTESIAN_POINT('Ctrl Pts',(3.89397685661728,-9.12158739409787,25.9265189319951));
#63047=CARTESIAN_POINT('Ctrl Pts',(3.89440722718893,-9.1216804777983,25.9264842514026));
#63048=CARTESIAN_POINT('Ctrl Pts',(3.89483759776058,-9.12177356149873,25.92644957081));
#63049=CARTESIAN_POINT('Ctrl Pts',(3.895265294967,-9.12186600409454,25.9264151272914));
#63050=CARTESIAN_POINT('Ctrl Pts',(3.89699038974,-9.12223935851648,25.9262760320526));
#63051=CARTESIAN_POINT('Ctrl Pts',(3.9058558713217,-9.12415807440555,25.9255612039185));
#63052=CARTESIAN_POINT('Ctrl Pts',(3.91470223383361,-9.12607907064862,25.924845712656));
#63053=CARTESIAN_POINT('Ctrl Pts',(3.92352948621133,-9.12800226777178,25.9241295886134));
#63054=CARTESIAN_POINT('Ctrl Pts',(4.08352764301896,-9.1628611323105,25.9111494990041));
#63055=CARTESIAN_POINT('Ctrl Pts',(4.23724642884231,-9.19843930276484,25.8979635305305));
#63056=CARTESIAN_POINT('Ctrl Pts',(4.38474644283691,-9.23428576561917,25.8847437456403));
#63057=CARTESIAN_POINT('Ctrl Pts',(4.40472431506602,-9.23914092485187,25.8829532158209));
#63058=CARTESIAN_POINT('Ctrl Pts',(4.42458812289106,-9.24400107295718,25.8811620300429));
#63059=CARTESIAN_POINT('Ctrl Pts',(4.44433803305825,-9.24886515182633,25.8793705828725));
#63060=CARTESIAN_POINT('Ctrl Pts',(4.59308014861258,-9.28549789471451,25.8658786915283));
#63061=CARTESIAN_POINT('Ctrl Pts',(4.735361183775,-9.32234986748804,25.8523740435749));
#63062=CARTESIAN_POINT('Ctrl Pts',(4.87125703060614,-9.35899576461154,25.8390153114756));
#63063=CARTESIAN_POINT('Ctrl Pts',(4.89542625203067,-9.36551327653359,25.8366394467117));
#63064=CARTESIAN_POINT('Ctrl Pts',(4.91939352613502,-9.37202438504967,25.8342681342935));
#63065=CARTESIAN_POINT('Ctrl Pts',(4.94315930694047,-9.37852684538982,25.8319021865218));
#63066=CARTESIAN_POINT('Ctrl Pts',(5.0799456786358,-9.41595241807781,25.8182847331775));
#63067=CARTESIAN_POINT('Ctrl Pts',(5.21005664561422,-9.45308782973976,25.8048471457304));
#63068=CARTESIAN_POINT('Ctrl Pts',(5.33358032146309,-9.48953465680202,25.7917336133098));
#63069=CARTESIAN_POINT('Ctrl Pts',(5.36978266052729,-9.50021649882182,25.7878902970892));
#63070=CARTESIAN_POINT('Ctrl Pts',(5.40541921763921,-9.51083948984573,25.7840746454648));
#63071=CARTESIAN_POINT('Ctrl Pts',(5.44049229352746,-9.52139432680783,25.7802898776826));
#63072=CARTESIAN_POINT('Ctrl Pts',(5.56339587865327,-9.55838074075091,25.767027239105));
#63073=CARTESIAN_POINT('Ctrl Pts',(5.67937988110502,-9.59452680014436,25.7541459868581));
#63074=CARTESIAN_POINT('Ctrl Pts',(5.78854158574026,-9.62946566961129,25.7417723345422));
#63075=CARTESIAN_POINT('Ctrl Pts',(5.84236905305293,-9.64669397197664,25.7356709057692));
#63076=CARTESIAN_POINT('Ctrl Pts',(5.89453776479577,-9.66362944720222,25.7296924705973));
#63077=CARTESIAN_POINT('Ctrl Pts',(5.94505953414157,-9.68023211648962,25.7238498365264));
#63078=CARTESIAN_POINT('Ctrl Pts',(5.95968624764569,-9.68503880656035,25.7221583174888));
#63079=CARTESIAN_POINT('Ctrl Pts',(5.97417491774219,-9.689817618351,25.7204781719848));
#63080=CARTESIAN_POINT('Ctrl Pts',(5.98852581858683,-9.69456763491412,25.7188097024708));
#63081=CARTESIAN_POINT('Ctrl Pts',(-6.39567216128937,-8.78352116600331,
25.5334667473151));
#63082=CARTESIAN_POINT('Ctrl Pts',(-6.35564926200295,-8.77012417292118,
25.5378747904695));
#63083=CARTESIAN_POINT('Ctrl Pts',(-5.98525108497463,-8.6474022387759,25.5783535630118));
#63084=CARTESIAN_POINT('Ctrl Pts',(-5.25617064763411,-8.42856486724208,
25.6522243920981));
#63085=CARTESIAN_POINT('Ctrl Pts',(-4.1757682916681,-8.16491404339211,25.7436212722339));
#63086=CARTESIAN_POINT('Ctrl Pts',(-3.01937523383598,-7.95089183270233,
25.8195369244464));
#63087=CARTESIAN_POINT('Ctrl Pts',(-1.83578803503655,-7.80507994015202,
25.8725332968182));
#63088=CARTESIAN_POINT('Ctrl Pts',(-0.697918458997622,-7.73463067220822,
25.8989855255588));
#63089=CARTESIAN_POINT('Ctrl Pts',(0.331420580112759,-7.72744138102246,
25.9017875116284));
#63090=CARTESIAN_POINT('Ctrl Pts',(1.24582508159658,-7.76509367288467,25.8874715584761));
#63091=CARTESIAN_POINT('Ctrl Pts',(2.0703196582245,-7.83520521068097,25.8615905206106));
#63092=CARTESIAN_POINT('Ctrl Pts',(2.81708947245881,-7.92875821572134,25.8276627710151));
#63093=CARTESIAN_POINT('Ctrl Pts',(3.49020566169626,-8.0378827718874,25.7886670556739));
#63094=CARTESIAN_POINT('Ctrl Pts',(4.09499065512871,-8.15592645391314,25.7470103559732));
#63095=CARTESIAN_POINT('Ctrl Pts',(4.6500687649082,-8.28093222016087,25.7034061523398));
#63096=CARTESIAN_POINT('Ctrl Pts',(5.18051476211263,-8.41545434309806,25.6570328769038));
#63097=CARTESIAN_POINT('Ctrl Pts',(5.70543165760628,-8.56333660797456,25.6067222305036));
#63098=CARTESIAN_POINT('Ctrl Pts',(6.10978786803773,-8.68891156621066,25.5646816773211));
#63099=CARTESIAN_POINT('Ctrl Pts',(6.34031815825487,-8.76499287475972,25.5395628680216));
#63100=CARTESIAN_POINT('Ctrl Pts',(6.39541677748914,-8.78343677823537,25.5334956641249));
#63101=CARTESIAN_POINT('Ctrl Pts',(-6.33018726788419,-9.06735941059648,
25.7767207816065));
#63102=CARTESIAN_POINT('Ctrl Pts',(-6.29063853345883,-9.05404377495881,
25.7811614548819));
#63103=CARTESIAN_POINT('Ctrl Pts',(-5.92460132235373,-8.93205700834798,
25.8219427981682));
#63104=CARTESIAN_POINT('Ctrl Pts',(-5.20364012968939,-8.71436432674133,
25.8964109697843));
#63105=CARTESIAN_POINT('Ctrl Pts',(-4.13466953168284,-8.4518979752872,25.9886148633439));
#63106=CARTESIAN_POINT('Ctrl Pts',(-2.99013639985378,-8.23872575964737,
26.0652406032874));
#63107=CARTESIAN_POINT('Ctrl Pts',(-1.81835116362302,-8.09343232209409,
26.1187453572149));
#63108=CARTESIAN_POINT('Ctrl Pts',(-0.691521315650298,-8.02320579194545,
26.1454462283406));
#63109=CARTESIAN_POINT('Ctrl Pts',(0.328421662670315,-8.01603646606291,
26.1482731581728));
#63110=CARTESIAN_POINT('Ctrl Pts',(1.2341212032938,-8.05357459156658,26.1338249563432));
#63111=CARTESIAN_POINT('Ctrl Pts',(2.0505435657801,-8.12345060526913,26.1076971639241));
#63112=CARTESIAN_POINT('Ctrl Pts',(2.78985534531287,-8.21666682407695,26.0734453634407));
#63113=CARTESIAN_POINT('Ctrl Pts',(3.45613744599942,-8.32537207799168,26.0340816249332));
#63114=CARTESIAN_POINT('Ctrl Pts',(4.05468755882963,-8.44293303358733,25.9920402440002));
#63115=CARTESIAN_POINT('Ctrl Pts',(4.60395024836123,-8.56739478506552,25.9480446147656));
#63116=CARTESIAN_POINT('Ctrl Pts',(5.12873138731788,-8.70129134259621,25.9012692232388));
#63117=CARTESIAN_POINT('Ctrl Pts',(5.64789963752306,-8.84843173585835,25.8505405843021));
#63118=CARTESIAN_POINT('Ctrl Pts',(6.04766646809667,-8.97331569512675,25.8081692666362));
#63119=CARTESIAN_POINT('Ctrl Pts',(6.2754891998086,-9.04894368857853,25.7828620346657));
#63120=CARTESIAN_POINT('Ctrl Pts',(6.32993458718007,-9.06727543043847,25.7767498760472));
#63121=CARTESIAN_POINT('Ctrl Pts',(-6.21932701877927,-9.42526885393706,
25.8366567723188));
#63122=CARTESIAN_POINT('Ctrl Pts',(-6.18048214170466,-9.4121663308803,25.8411264604673));
#63123=CARTESIAN_POINT('Ctrl Pts',(-5.82094578598021,-9.29212707116419,
25.8821758663682));
#63124=CARTESIAN_POINT('Ctrl Pts',(-5.11256644425228,-9.07783407043934,
25.9571568476127));
#63125=CARTESIAN_POINT('Ctrl Pts',(-4.06220274945981,-8.81944032503722,
26.0500340658684));
#63126=CARTESIAN_POINT('Ctrl Pts',(-2.93773889681033,-8.60958787110744,
26.127238451141));
#63127=CARTESIAN_POINT('Ctrl Pts',(-1.78661058007677,-8.46656410207219,
26.1811448105063));
#63128=CARTESIAN_POINT('Ctrl Pts',(-0.679622419473119,-8.39742515837133,
26.2080312380617));
#63129=CARTESIAN_POINT('Ctrl Pts',(0.322802864782609,-8.39036439860734,
26.2108752950314));
#63130=CARTESIAN_POINT('Ctrl Pts',(1.21266718731651,-8.42732524877291,26.1963309615885));
#63131=CARTESIAN_POINT('Ctrl Pts',(2.01471122069113,-8.49611283173201,26.1700131751107));
#63132=CARTESIAN_POINT('Ctrl Pts',(2.74099430211639,-8.58787416570904,26.1355048218257));
#63133=CARTESIAN_POINT('Ctrl Pts',(3.39556606614342,-8.69488456823181,26.0958439655793));
#63134=CARTESIAN_POINT('Ctrl Pts',(3.98363652396525,-8.81061649534371,26.0534875495589));
#63135=CARTESIAN_POINT('Ctrl Pts',(4.52331543764338,-8.93314488999573,26.0091674680472));
#63136=CARTESIAN_POINT('Ctrl Pts',(5.03895717721903,-9.06496118679828,25.9620547272721));
#63137=CARTESIAN_POINT('Ctrl Pts',(5.54907347998645,-9.20980765316832,25.9109704011966));
#63138=CARTESIAN_POINT('Ctrl Pts',(5.94182258892166,-9.33272612605645,25.8683120901775));
#63139=CARTESIAN_POINT('Ctrl Pts',(6.1656025554792,-9.40714791972507,25.8428381607526));
#63140=CARTESIAN_POINT('Ctrl Pts',(6.21907854257829,-9.42518611321531,25.8366860115496));
#63141=CARTESIAN_POINT('Ctrl Pts',(-6.09477777755571,-9.75501019029731,
25.6963138452313));
#63142=CARTESIAN_POINT('Ctrl Pts',(-6.05666531980665,-9.74219158610546,
25.7008006525782));
#63143=CARTESIAN_POINT('Ctrl Pts',(-5.70391204412257,-9.62475519120128,
25.742007112709));
#63144=CARTESIAN_POINT('Ctrl Pts',(-5.00898154501689,-9.41514444969426,
25.8172700391757));
#63145=CARTESIAN_POINT('Ctrl Pts',(-3.9790819862615,-9.16254640127591,25.9104947771135));
#63146=CARTESIAN_POINT('Ctrl Pts',(-2.87716051673702,-8.95753370316113,
25.98798127695));
#63147=CARTESIAN_POINT('Ctrl Pts',(-1.74963953464299,-8.81788142038787,
26.0420678997381));
#63148=CARTESIAN_POINT('Ctrl Pts',(-0.66562326086846,-8.75038371137221,
26.0690238753989));
#63149=CARTESIAN_POINT('Ctrl Pts',(0.31617042790742,-8.74348905173393,26.0718723597058));
#63150=CARTESIAN_POINT('Ctrl Pts',(1.18759586946167,-8.77957470163612,26.0572954265023));
#63151=CARTESIAN_POINT('Ctrl Pts',(1.97306545476681,-8.84673237888208,26.0308986009111));
#63152=CARTESIAN_POINT('Ctrl Pts',(2.6844732657847,-8.93633699629108,25.9962743802485));
#63153=CARTESIAN_POINT('Ctrl Pts',(3.32580559191093,-9.04086190150178,25.9564720770166));
#63154=CARTESIAN_POINT('Ctrl Pts',(3.90214690596376,-9.15394176510944,25.9139601535985));
#63155=CARTESIAN_POINT('Ctrl Pts',(4.4312128214806,-9.27370054758531,25.8694751653495));
#63156=CARTESIAN_POINT('Ctrl Pts',(4.93685264935617,-9.40257696777726,25.8221860981219));
#63157=CARTESIAN_POINT('Ctrl Pts',(5.43720062470865,-9.54423361014413,25.7709098835103));
#63158=CARTESIAN_POINT('Ctrl Pts',(5.82250913003638,-9.66447427448976,25.7280902474343));
#63159=CARTESIAN_POINT('Ctrl Pts',(6.04206637679057,-9.7372819550532,25.7025189180159));
#63160=CARTESIAN_POINT('Ctrl Pts',(6.09453380570084,-9.75492916631022,25.696343155098));
#63161=CARTESIAN_POINT('',(6.27159454902671,-8.76071457519094,25.5608537658479));
#63162=CARTESIAN_POINT('Origin',(5.999999949031,-9.33250966434584,24.7867247244592));
#63163=CARTESIAN_POINT('Ctrl Pts',(-6.27159387328075,-8.76070928018809,
25.560857166473));
#63164=CARTESIAN_POINT('Ctrl Pts',(-6.1323966152263,-8.71504797181017,25.5759656528077));
#63165=CARTESIAN_POINT('Ctrl Pts',(-5.98564485576888,-8.66855400399287,
25.5914802336782));
#63166=CARTESIAN_POINT('Ctrl Pts',(-5.83132853839285,-8.62173957209145,
25.6072278332491));
#63167=CARTESIAN_POINT('Ctrl Pts',(-5.67907395050422,-8.57555060026016,
25.622765038411));
#63168=CARTESIAN_POINT('Ctrl Pts',(-5.51945529064096,-8.52904980925714,
25.6385292621719));
#63169=CARTESIAN_POINT('Ctrl Pts',(-5.35247220392677,-8.4827683508267,25.6543232525887));
#63170=CARTESIAN_POINT('Ctrl Pts',(-5.32566844713921,-8.47533935319614,
25.6568584690957));
#63171=CARTESIAN_POINT('Ctrl Pts',(-5.2986749639072,-8.4679160874565,25.6593943834507));
#63172=CARTESIAN_POINT('Ctrl Pts',(-5.27149178336552,-8.46050084257278,
25.6619300990734));
#63173=CARTESIAN_POINT('Ctrl Pts',(-5.14595766075532,-8.42625664296592,
25.6736402385623));
#63174=CARTESIAN_POINT('Ctrl Pts',(-5.01637753192559,-8.3921823907687,25.6853467760197));
#63175=CARTESIAN_POINT('Ctrl Pts',(-4.88275736863916,-8.35851823696374,
25.6969639538638));
#63176=CARTESIAN_POINT('Ctrl Pts',(-4.71106402408442,-8.31526195725101,
25.7118912827137));
#63177=CARTESIAN_POINT('Ctrl Pts',(-4.53269542172315,-8.27268029475778,
25.7266725174848));
#63178=CARTESIAN_POINT('Ctrl Pts',(-4.34764537476528,-8.23131615277371,
25.7411116072797));
#63179=CARTESIAN_POINT('Ctrl Pts',(-4.29584306648741,-8.21973680940182,
25.7451536391144));
#63180=CARTESIAN_POINT('Ctrl Pts',(-4.24351727085387,-8.20825312966762,
25.7491687071653));
#63181=CARTESIAN_POINT('Ctrl Pts',(-4.19066810075872,-8.19687761788522,
25.7531521496353));
#63182=CARTESIAN_POINT('Ctrl Pts',(-4.14339042324644,-8.18670134119786,
25.7567156475699));
#63183=CARTESIAN_POINT('Ctrl Pts',(-4.0956939046934,-8.17661163141362,25.7602538330852));
#63184=CARTESIAN_POINT('Ctrl Pts',(-4.047578973713,-8.16661761355435,25.7637634434875));
#63185=CARTESIAN_POINT('Ctrl Pts',(-3.90056245654704,-8.13608061249819,
25.7744871562197));
#63186=CARTESIAN_POINT('Ctrl Pts',(-3.7496359565824,-8.10643536805442,25.7849451020033));
#63187=CARTESIAN_POINT('Ctrl Pts',(-3.59479964942688,-8.0779501732433,25.7950405868657));
#63188=CARTESIAN_POINT('Ctrl Pts',(-3.51738149584912,-8.06370757583774,
25.8000883292969));
#63189=CARTESIAN_POINT('Ctrl Pts',(-3.43898588186198,-8.0497552353687,25.8050453472066));
#63190=CARTESIAN_POINT('Ctrl Pts',(-3.35961278010336,-8.03612820885441,
25.8098988471816));
#63191=CARTESIAN_POINT('Ctrl Pts',(-3.31992622922405,-8.02931469559726,
25.8123255971691));
#63192=CARTESIAN_POINT('Ctrl Pts',(-3.27999530401069,-8.02258252072975,
25.81472645521));
#63193=CARTESIAN_POINT('Ctrl Pts',(-3.23982000049219,-8.01593617299398,
25.8170997788106));
#63194=CARTESIAN_POINT('Ctrl Pts',(-3.21973234873293,-8.01261299912609,
25.8182864406108));
#63195=CARTESIAN_POINT('Ctrl Pts',(-3.1995836022476,-8.00931128268966,25.8194662179862));
#63196=CARTESIAN_POINT('Ctrl Pts',(-3.17937376004829,-8.00603159000866,
25.8206389016039));
#63197=CARTESIAN_POINT('Ctrl Pts',(-3.16169014812389,-8.00316185891278,
25.8216649997694));
#63198=CARTESIAN_POINT('Ctrl Pts',(-3.14395975978476,-8.00030898979315,
25.8226856667284));
#63199=CARTESIAN_POINT('Ctrl Pts',(-3.12618259427586,-7.99747336460349,
25.8237007607655));
#63200=CARTESIAN_POINT('Ctrl Pts',(-3.12364299920317,-7.99706827529068,
25.8238457741994));
#63201=CARTESIAN_POINT('Ctrl Pts',(-3.11986202403536,-7.99646617108508,
25.8240613390158));
#63202=CARTESIAN_POINT('Ctrl Pts',(-3.11856094515192,-7.99625915356409,
25.8241354594592));
#63203=CARTESIAN_POINT('Ctrl Pts',(-3.09161528851505,-7.99197177090832,
25.8256705116704));
#63204=CARTESIAN_POINT('Ctrl Pts',(-3.06344467690482,-7.9875467889361,25.8272569731113));
#63205=CARTESIAN_POINT('Ctrl Pts',(-3.03404913715077,-7.98300009354392,
25.8288891657581));
#63206=CARTESIAN_POINT('Ctrl Pts',(-2.96198356806363,-7.97185349805207,
25.83289061948));
#63207=CARTESIAN_POINT('Ctrl Pts',(-2.88255590909974,-7.95997199195539,
25.8371681774551));
#63208=CARTESIAN_POINT('Ctrl Pts',(-2.79576579462087,-7.9476233532413,25.8416259690135));
#63209=CARTESIAN_POINT('Ctrl Pts',(-2.70930593296023,-7.93532170343557,
25.846066797831));
#63210=CARTESIAN_POINT('Ctrl Pts',(-2.61553929356376,-7.92255647438925,
25.8506865367989));
#63211=CARTESIAN_POINT('Ctrl Pts',(-2.51446660864717,-7.9096408053862,25.8553721684044));
#63212=CARTESIAN_POINT('Ctrl Pts',(-2.50260224764738,-7.90812470675151,
25.8559221886688));
#63213=CARTESIAN_POINT('Ctrl Pts',(-2.49063721965791,-7.9066065901873,25.8564730956623));
#63214=CARTESIAN_POINT('Ctrl Pts',(-2.47857152941463,-7.90508700613539,
25.8570246895332));
#63215=CARTESIAN_POINT('Ctrl Pts',(-2.37688572601341,-7.8922804346058,25.861673347404));
#63216=CARTESIAN_POINT('Ctrl Pts',(-2.26804993547395,-7.87936601620428,
25.8663725584229));
#63217=CARTESIAN_POINT('Ctrl Pts',(-2.15206295112008,-7.8667005243223,25.8709938985986));
#63218=CARTESIAN_POINT('Ctrl Pts',(-2.11969748351752,-7.86316629529255,
25.8722834556689));
#63219=CARTESIAN_POINT('Ctrl Pts',(-2.08677523011003,-7.85965173436756,
25.8735668343966));
#63220=CARTESIAN_POINT('Ctrl Pts',(-2.05329628484806,-7.85616525875198,
25.8748409739275));
#63221=CARTESIAN_POINT('Ctrl Pts',(-1.97656815473855,-7.84817484111597,
25.8777610881349));
#63222=CARTESIAN_POINT('Ctrl Pts',(-1.89691554666913,-7.84033139559416,
25.8806329582618));
#63223=CARTESIAN_POINT('Ctrl Pts',(-1.8143384154204,-7.83274216428475,25.8834176179311));
#63224=CARTESIAN_POINT('Ctrl Pts',(-1.81240217498234,-7.83256421457479,
25.8834829116823));
#63225=CARTESIAN_POINT('Ctrl Pts',(-1.81046432668551,-7.83238640486458,
25.8835481572174));
#63226=CARTESIAN_POINT('Ctrl Pts',(-1.8085248705108,-7.83220873662038,25.8836133540381));
#63227=CARTESIAN_POINT('Ctrl Pts',(-1.76910718840288,-7.82859779121116,
25.884938420098));
#63228=CARTESIAN_POINT('Ctrl Pts',(-1.72902532971431,-7.82504524963275,
25.8862433793847));
#63229=CARTESIAN_POINT('Ctrl Pts',(-1.68827931773378,-7.82156332449908,
25.8875239411442));
#63230=CARTESIAN_POINT('Ctrl Pts',(-1.66690390495163,-7.81973670188275,
25.8881957255686));
#63231=CARTESIAN_POINT('Ctrl Pts',(-1.64534571176604,-7.81792951698791,
25.8888607907406));
#63232=CARTESIAN_POINT('Ctrl Pts',(-1.62360473903617,-7.81614356896003,
25.8895184936256));
#63233=CARTESIAN_POINT('Ctrl Pts',(-1.61273425267123,-7.81525059494608,
25.8898473450681));
#63234=CARTESIAN_POINT('Ctrl Pts',(-1.60181807138526,-7.81436293042739,
25.890174355595));
#63235=CARTESIAN_POINT('Ctrl Pts',(-1.59085619528081,-7.81348080326641,
25.8904994437807));
#63236=CARTESIAN_POINT('Ctrl Pts',(-1.58537525722859,-7.81303973968592,
25.8906619878735));
#63237=CARTESIAN_POINT('Ctrl Pts',(-1.57988289546958,-7.81260006046241,
25.8908240513594));
#63238=CARTESIAN_POINT('Ctrl Pts',(-1.57437911001673,-7.81216179426874,
25.8909856239973));
#63239=CARTESIAN_POINT('Ctrl Pts',(-1.56887532456389,-7.81172352807508,
25.8911471966352));
#63240=CARTESIAN_POINT('Ctrl Pts',(-1.56205959677632,-7.81118421457966,
25.8913460660047));
#63241=CARTESIAN_POINT('Ctrl Pts',(-1.55783348258494,-7.8108512635462,25.8914688590589));
#63242=CARTESIAN_POINT('Ctrl Pts',(-1.33210030446669,-7.79306705527876,
25.8980277131554));
#63243=CARTESIAN_POINT('Ctrl Pts',(-1.11005375162319,-7.77943810586309,
25.9030588947695));
#63244=CARTESIAN_POINT('Ctrl Pts',(-0.891696882492288,-7.76958903507536,
25.9066954247431));
#63245=CARTESIAN_POINT('Ctrl Pts',(-0.848420665378784,-7.76763704461373,
25.9074161497713));
#63246=CARTESIAN_POINT('Ctrl Pts',(-0.805289271297393,-7.7658336506397,
25.9080820807832));
#63247=CARTESIAN_POINT('Ctrl Pts',(-0.76230257197877,-7.76417611439376,
25.9086942333594));
#63248=CARTESIAN_POINT('Ctrl Pts',(-0.724714216543341,-7.76272673441003,
25.9092295107587));
#63249=CARTESIAN_POINT('Ctrl Pts',(-0.687236480829822,-7.76138885372218,
25.9097236478486));
#63250=CARTESIAN_POINT('Ctrl Pts',(-0.649869562680107,-7.76016057469741,
25.9101772242416));
#63251=CARTESIAN_POINT('Ctrl Pts',(-0.558060599569084,-7.75714274424043,
25.9112916425663));
#63252=CARTESIAN_POINT('Ctrl Pts',(-0.466920649099576,-7.75478646686927,
25.912161232118));
#63253=CARTESIAN_POINT('Ctrl Pts',(-0.376448945799055,-7.75306363563768,
25.9127967462999));
#63254=CARTESIAN_POINT('Ctrl Pts',(-0.312801772326068,-7.75185161757831,
25.9132438328464));
#63255=CARTESIAN_POINT('Ctrl Pts',(-0.249485486100613,-7.75095306723222,
25.9135750128796));
#63256=CARTESIAN_POINT('Ctrl Pts',(-0.186500087442505,-7.7503583424659,
25.9137938244159));
#63257=CARTESIAN_POINT('Ctrl Pts',(-0.15500738811345,-7.75006098008275,
25.913903230184));
#63258=CARTESIAN_POINT('Ctrl Pts',(-0.123597410553174,-7.74983957602615,
25.9139845414595));
#63259=CARTESIAN_POINT('Ctrl Pts',(-0.0922701543828133,-7.74969293858145,
25.9140381884101));
#63260=CARTESIAN_POINT('Ctrl Pts',(-0.0647192855148777,-7.74956397774978,
25.914085368415));
#63261=CARTESIAN_POINT('Ctrl Pts',(-0.0383381923124055,-7.74949397676687,
25.9141107439043));
#63262=CARTESIAN_POINT('Ctrl Pts',(-0.0102093864688425,-7.74947894153103,
25.9141157544645));
#63263=CARTESIAN_POINT('Ctrl Pts',(-0.00635378156109146,-7.74947688065687,
25.9141164412601));
#63264=CARTESIAN_POINT('Ctrl Pts',(-0.0024653403777432,-7.74947592698224,
25.9141167172151));
#63265=CARTESIAN_POINT('Ctrl Pts',(0.00146345041170125,-7.74947614296011,
25.9141165584631));
#63266=CARTESIAN_POINT('Ctrl Pts',(0.124001691178138,-7.74948287926902,
25.9141116070182));
#63267=CARTESIAN_POINT('Ctrl Pts',(0.246536534909898,-7.75063935015112,
25.91369518508));
#63268=CARTESIAN_POINT('Ctrl Pts',(0.369073085050784,-7.75293732746282,
25.9128590542009));
#63269=CARTESIAN_POINT('Ctrl Pts',(0.644887810889202,-7.75810979218033,
25.910977026276));
#63270=CARTESIAN_POINT('Ctrl Pts',(0.92071099518736,-7.76906234542254,25.9069696802048));
#63271=CARTESIAN_POINT('Ctrl Pts',(1.1965320497517,-7.78581292554686,25.9008588258509));
#63272=CARTESIAN_POINT('Ctrl Pts',(1.22213119051329,-7.78736755834716,25.900291673278));
#63273=CARTESIAN_POINT('Ctrl Pts',(1.24773031471214,-7.7889721694523,25.8997063896472));
#63274=CARTESIAN_POINT('Ctrl Pts',(1.27332941464932,-7.79062679485959,25.8991029852857));
#63275=CARTESIAN_POINT('Ctrl Pts',(1.37083893333184,-7.79692942766547,25.8968045580361));
#63276=CARTESIAN_POINT('Ctrl Pts',(1.46834810130389,-7.80395767161213,25.8942432317263));
#63277=CARTESIAN_POINT('Ctrl Pts',(1.5658568717593,-7.81170938517129,25.8914183110703));
#63278=CARTESIAN_POINT('Ctrl Pts',(1.74018694254622,-7.82556820799489,25.8863678051966));
#63279=CARTESIAN_POINT('Ctrl Pts',(1.91451739829087,-7.84174034092828,25.8804757772071));
#63280=CARTESIAN_POINT('Ctrl Pts',(2.08884740122651,-7.86022612185766,25.8737415026613));
#63281=CARTESIAN_POINT('Ctrl Pts',(2.1752494959535,-7.86938811444681,25.8704038360667));
#63282=CARTESIAN_POINT('Ctrl Pts',(2.2616514622376,-7.87911855871861,25.8668592399187));
#63283=CARTESIAN_POINT('Ctrl Pts',(2.34805359106619,-7.88941699552813,25.8631079381382));
#63284=CARTESIAN_POINT('Ctrl Pts',(2.47841969135101,-7.90495558310797,25.857447862504));
#63285=CARTESIAN_POINT('Ctrl Pts',(2.60878583075759,-7.92178731750336,25.8513174296772));
#63286=CARTESIAN_POINT('Ctrl Pts',(2.73915198198545,-7.939912050948,25.8447165665306));
#63287=CARTESIAN_POINT('Ctrl Pts',(2.77255377534431,-7.94455588368756,25.8430253248644));
#63288=CARTESIAN_POINT('Ctrl Pts',(2.80595557540632,-7.94928459706181,25.8413031872238));
#63289=CARTESIAN_POINT('Ctrl Pts',(2.8393573637312,-7.95409821372544,25.8395501483932));
#63290=CARTESIAN_POINT('Ctrl Pts',(2.8711386411965,-7.95867829444779,25.8378821594538));
#63291=CARTESIAN_POINT('Ctrl Pts',(2.90291990800943,-7.96333524011162,25.8361861949494));
#63292=CARTESIAN_POINT('Ctrl Pts',(2.93470118017488,-7.96806902124732,25.8344622613891));
#63293=CARTESIAN_POINT('Ctrl Pts',(2.98358847136506,-7.97535072273512,25.8318104341899));
#63294=CARTESIAN_POINT('Ctrl Pts',(3.03247575908502,-7.98281424431422,25.8290924421403));
#63295=CARTESIAN_POINT('Ctrl Pts',(3.08136304923064,-7.99045953912554,25.8263083281147));
#63296=CARTESIAN_POINT('Ctrl Pts',(3.09765881261251,-7.99300797072931,25.8253802901061));
#63297=CARTESIAN_POINT('Ctrl Pts',(3.11203760285011,-7.99527205976141,25.8245558044054));
#63298=CARTESIAN_POINT('Ctrl Pts',(3.13025034020354,-7.99816542434384,25.8235021736296));
#63299=CARTESIAN_POINT('Ctrl Pts',(3.25878004893528,-8.01858428285028,25.8160665611734));
#63300=CARTESIAN_POINT('Ctrl Pts',(3.38588994776671,-8.04008769017049,25.808299088878));
#63301=CARTESIAN_POINT('Ctrl Pts',(3.5115662710351,-8.0625905343887,25.8002296274968));
#63302=CARTESIAN_POINT('Ctrl Pts',(3.71382498700818,-8.09880575981026,25.7872429418976));
#63303=CARTESIAN_POINT('Ctrl Pts',(3.91236990026725,-8.13760860679937,25.773474678434));
#63304=CARTESIAN_POINT('Ctrl Pts',(4.10716724986624,-8.17865262650198,25.7590464903351));
#63305=CARTESIAN_POINT('Ctrl Pts',(4.29251707950218,-8.21770604316864,25.7453180581382));
#63306=CARTESIAN_POINT('Ctrl Pts',(4.47447431949519,-8.25878866878335,25.7309921243262));
#63307=CARTESIAN_POINT('Ctrl Pts',(4.65302915034081,-8.30161628112533,25.7161694333478));
#63308=CARTESIAN_POINT('Ctrl Pts',(4.83066811792946,-8.34422421732446,25.7014227725612));
#63309=CARTESIAN_POINT('Ctrl Pts',(5.00493963976845,-8.38855938233988,25.6861844892871));
#63310=CARTESIAN_POINT('Ctrl Pts',(5.17584967464822,-8.43435907663826,25.6705507275121));
#63311=CARTESIAN_POINT('Ctrl Pts',(5.35322086172,-8.48189020113277,25.6543259406738));
#63312=CARTESIAN_POINT('Ctrl Pts',(5.52697168029971,-8.53099876652162,25.6376753760724));
#63313=CARTESIAN_POINT('Ctrl Pts',(5.69712367345923,-8.58141411828093,25.6207040708845));
#63314=CARTESIAN_POINT('Ctrl Pts',(5.87745455215751,-8.63484543291804,25.6027175029908));
#63315=CARTESIAN_POINT('Ctrl Pts',(6.0537431675926,-8.68974474910015,25.584371006453));
#63316=CARTESIAN_POINT('Ctrl Pts',(6.22602835761291,-8.74582172598816,25.565788475961));
#63317=CARTESIAN_POINT('Ctrl Pts',(6.24124881340971,-8.75077582069497,25.5641468108595));
#63318=CARTESIAN_POINT('Ctrl Pts',(6.25643802960122,-8.75573911480345,25.5625032922101));
#63319=CARTESIAN_POINT('Ctrl Pts',(6.27159604049145,-8.76071143385986,25.5608580131143));
#63320=CARTESIAN_POINT('Origin',(5.999999999061,-9.33250979146063,24.7867247845918));
#63321=CARTESIAN_POINT('Origin',(5.9999696860333,-9.33251391797614,24.7866936474829));
#63322=CARTESIAN_POINT('Ctrl Pts',(6.25606545383873,-3.90351699726741,15.8245348638446));
#63323=CARTESIAN_POINT('Ctrl Pts',(6.27805137190582,-3.90938776964027,15.8167706309341));
#63324=CARTESIAN_POINT('Ctrl Pts',(6.38303596649425,-3.94105812481732,15.7785558941617));
#63325=CARTESIAN_POINT('Ctrl Pts',(6.5644009396555,-4.02787637947969,15.7024427068931));
#63326=CARTESIAN_POINT('Ctrl Pts',(6.77569464165061,-4.20161916671313,15.5905393483866));
#63327=CARTESIAN_POINT('Ctrl Pts',(6.94551705571754,-4.42824393788803,15.4722330995486));
#63328=CARTESIAN_POINT('Ctrl Pts',(7.06116197196841,-4.69652825400431,15.3539457728218));
#63329=CARTESIAN_POINT('Ctrl Pts',(7.10123737675459,-4.92249133588564,15.2686302662615));
#63330=CARTESIAN_POINT('Ctrl Pts',(7.10450937548937,-5.05228130021626,15.2245558649972));
#63331=CARTESIAN_POINT('Ctrl Pts',(7.10419841572891,-5.08306982967337,15.214375952807));
#63332=CARTESIAN_POINT('Ctrl Pts',(6.05790170975049,-3.86072516060592,15.2131216290605));
#63333=CARTESIAN_POINT('Ctrl Pts',(6.0774019058006,-3.86578803164919,15.2062195803066));
#63334=CARTESIAN_POINT('Ctrl Pts',(6.17060154414674,-3.89313992573329,15.1722159993409));
#63335=CARTESIAN_POINT('Ctrl Pts',(6.33230417363677,-3.96853916358796,15.1042106702778));
#63336=CARTESIAN_POINT('Ctrl Pts',(6.52172609417125,-4.12063635096875,15.0038198058236));
#63337=CARTESIAN_POINT('Ctrl Pts',(6.67461078702923,-4.3201963578824,14.8975475181414));
#63338=CARTESIAN_POINT('Ctrl Pts',(6.77898374399282,-4.55736055760934,14.7914865810048));
#63339=CARTESIAN_POINT('Ctrl Pts',(6.81513903772793,-4.75736053874658,14.7154446390863));
#63340=CARTESIAN_POINT('Ctrl Pts',(6.81807628979981,-4.87201821631841,14.6764666609063));
#63341=CARTESIAN_POINT('Ctrl Pts',(6.81779568545588,-4.89919678109847,14.6674846276254));
#63342=CARTESIAN_POINT('Ctrl Pts',(6.04883558612803,-3.36577005918539,14.8011311726366));
#63343=CARTESIAN_POINT('Ctrl Pts',(6.07566935314429,-3.37269321401156,14.7918321486262));
#63344=CARTESIAN_POINT('Ctrl Pts',(6.20353926856132,-3.40998966365746,14.7462158572278));
#63345=CARTESIAN_POINT('Ctrl Pts',(6.42226858523589,-3.51153022966031,14.6566846143631));
#63346=CARTESIAN_POINT('Ctrl Pts',(6.67386632509817,-3.71204279852219,14.5274200429916));
#63347=CARTESIAN_POINT('Ctrl Pts',(6.87408391635468,-3.97082561139319,14.3925000997621));
#63348=CARTESIAN_POINT('Ctrl Pts',(7.0096100495298,-4.27508245854162,14.2585887417136));
#63349=CARTESIAN_POINT('Ctrl Pts',(7.05661851482608,-4.53102183000274,14.1620489883948));
#63350=CARTESIAN_POINT('Ctrl Pts',(7.06050233450235,-4.67877914994309,14.1118773452502));
#63351=CARTESIAN_POINT('Ctrl Pts',(7.06013777230322,-4.71389394697659,14.1002657353677));
#63352=CARTESIAN_POINT('Ctrl Pts',(6.23484754158759,-2.75271794669507,14.8662289006106));
#63353=CARTESIAN_POINT('Ctrl Pts',(6.27388224199307,-2.76291330524427,14.8528923137333));
#63354=CARTESIAN_POINT('Ctrl Pts',(6.45946683867096,-2.81770168594271,14.7876810214237));
#63355=CARTESIAN_POINT('Ctrl Pts',(6.77340486060312,-2.96529042143721,14.6615258505952));
#63356=CARTESIAN_POINT('Ctrl Pts',(7.12924177467691,-3.2515836066926,14.4824993052424));
#63357=CARTESIAN_POINT('Ctrl Pts',(7.40910112429138,-3.61588219559613,14.2975958045458));
#63358=CARTESIAN_POINT('Ctrl Pts',(7.59716915501324,-4.04013483631764,14.1145649290726));
#63359=CARTESIAN_POINT('Ctrl Pts',(7.66247539438356,-4.39613857922254,13.9815985925293));
#63360=CARTESIAN_POINT('Ctrl Pts',(7.66794792454828,-4.60287447369357,13.9115025369606));
#63361=CARTESIAN_POINT('Ctrl Pts',(7.66744178437245,-4.65211218126055,13.8952097092579));
#63362=CARTESIAN_POINT('',(6.999992922344,-4.92966736222272,14.7967908129515));
#63363=CARTESIAN_POINT('',(6.99999949429353,-3.16610543777311,14.5427473811435));
#63364=CARTESIAN_POINT('Ctrl Pts',(7.,-4.92966736222272,14.7967908129515));
#63365=CARTESIAN_POINT('Ctrl Pts',(7.,-4.82678420804455,14.7560363096686));
#63366=CARTESIAN_POINT('Ctrl Pts',(7.,-4.7336540376644,14.7215027168286));
#63367=CARTESIAN_POINT('Ctrl Pts',(7.,-4.65186515615285,14.6935521165994));
#63368=CARTESIAN_POINT('Ctrl Pts',(7.,-4.61097071539707,14.6795768164848));
#63369=CARTESIAN_POINT('Ctrl Pts',(7.,-4.5729198001806,14.6672023399456));
#63370=CARTESIAN_POINT('Ctrl Pts',(7.,-4.53794478179076,14.6562662959784));
#63371=CARTESIAN_POINT('Ctrl Pts',(7.,-4.52045727259585,14.6507982739948));
#63372=CARTESIAN_POINT('Ctrl Pts',(7.,-4.50373880126536,14.6456882660439));
#63373=CARTESIAN_POINT('Ctrl Pts',(7.,-4.48781746868666,14.6409089126752));
#63374=CARTESIAN_POINT('Ctrl Pts',(7.,-4.4798568023973,14.6385192359908));
#63375=CARTESIAN_POINT('Ctrl Pts',(7.,-4.4720954207959,14.636212222952));
#63376=CARTESIAN_POINT('Ctrl Pts',(7.,-4.46453666087317,14.6339841494894));
#63377=CARTESIAN_POINT('Ctrl Pts',(7.,-4.46075728091181,14.6328701127582));
#63378=CARTESIAN_POINT('Ctrl Pts',(7.,-4.45702855637012,14.631775810921));
#63379=CARTESIAN_POINT('Ctrl Pts',(7.,-4.4533508950384,14.6307007794326));
#63380=CARTESIAN_POINT('Ctrl Pts',(7.,-4.44967323370668,14.6296257479442));
#63381=CARTESIAN_POINT('Ctrl Pts',(7.,-4.44764784207163,14.6290344140039));
#63382=CARTESIAN_POINT('Ctrl Pts',(7.,-4.44247150462448,14.6275330288263));
#63383=CARTESIAN_POINT('Ctrl Pts',(7.,-4.35965010547007,14.603510865984));
#63384=CARTESIAN_POINT('Ctrl Pts',(7.,-4.27939235138988,14.583009037268));
#63385=CARTESIAN_POINT('Ctrl Pts',(7.,-4.20230683567458,14.5661068011664));
#63386=CARTESIAN_POINT('Ctrl Pts',(7.,-4.12522131995927,14.5492045650647));
#63387=CARTESIAN_POINT('Ctrl Pts',(7.,-4.05295459894647,14.5361280509262));
#63388=CARTESIAN_POINT('Ctrl Pts',(7.,-3.98140820749628,14.5256481770255));
#63389=CARTESIAN_POINT('Ctrl Pts',(7.,-3.8383154245959,14.5046884292241));
#63390=CARTESIAN_POINT('Ctrl Pts',(7.,-3.69579585817385,14.4945162284038));
#63391=CARTESIAN_POINT('Ctrl Pts',(7.,-3.55814223775101,14.4974061202244));
#63392=CARTESIAN_POINT('Ctrl Pts',(7.,-3.42048861732817,14.500296012045));
#63393=CARTESIAN_POINT('Ctrl Pts',(7.,-3.28795185895767,14.516219567648));
#63394=CARTESIAN_POINT('Ctrl Pts',(7.,-3.16610527255026,14.542746622232));
#63395=CARTESIAN_POINT('',(6.25003741340704,-2.76548799388388,14.8593558170211));
#63396=CARTESIAN_POINT('Ctrl Pts',(6.25007095100041,-2.7654967482904,14.8593452070851));
#63397=CARTESIAN_POINT('Ctrl Pts',(6.33587163725197,-2.78878256441424,14.8297752073987));
#63398=CARTESIAN_POINT('Ctrl Pts',(6.41875467614383,-2.81766749093033,14.7993819051698));
#63399=CARTESIAN_POINT('Ctrl Pts',(6.49900053547044,-2.85195696894397,14.7681022183498));
#63400=CARTESIAN_POINT('Ctrl Pts',(6.50620156545211,-2.85503400695321,14.7652952702469));
#63401=CARTESIAN_POINT('Ctrl Pts',(6.51338135583404,-2.85815456038784,14.7624811504726));
#63402=CARTESIAN_POINT('Ctrl Pts',(6.52054010747125,-2.86131848501783,14.7596597937132));
#63403=CARTESIAN_POINT('Ctrl Pts',(6.60751266789611,-2.89975739727608,14.7253827809508));
#63404=CARTESIAN_POINT('Ctrl Pts',(6.6913787906444,-2.94459799689971,14.6900381286337));
#63405=CARTESIAN_POINT('Ctrl Pts',(6.77140018943003,-2.99541632456422,14.6538748180838));
#63406=CARTESIAN_POINT('Ctrl Pts',(6.84311703907017,-3.04096077166697,14.6214645035361));
#63407=CARTESIAN_POINT('Ctrl Pts',(6.91174725714638,-3.09130726141184,14.5884002469452));
#63408=CARTESIAN_POINT('Ctrl Pts',(6.97733631082931,-3.14667082030927,14.5545423490562));
#63409=CARTESIAN_POINT('Ctrl Pts',(6.984931283593,-3.15308171813926,14.5506217281924));
#63410=CARTESIAN_POINT('Ctrl Pts',(6.99248547643967,-3.15955987192872,14.5466904104436));
#63411=CARTESIAN_POINT('Ctrl Pts',(6.9999989586745,-3.16610560191081,14.5427481350708));
#63412=CARTESIAN_POINT('',(6.26385797816486,-3.90573660195549,15.8144409703668));
#63413=CARTESIAN_POINT('Origin',(6.527982188659,-2.94130808174632,15.8037261610702));
#63414=CARTESIAN_POINT('Ctrl Pts',(6.2638990751077,-3.90574413173893,15.8144151702401));
#63415=CARTESIAN_POINT('Ctrl Pts',(6.2809593183397,-3.91053019376344,15.803450612777));
#63416=CARTESIAN_POINT('Ctrl Pts',(6.29796648298088,-3.91580576242035,15.7922459989039));
#63417=CARTESIAN_POINT('Ctrl Pts',(6.31489097527796,-3.92157938126428,15.7808042255943));
#63418=CARTESIAN_POINT('Ctrl Pts',(6.35719245850541,-3.93601010310817,15.752206382111));
#63419=CARTESIAN_POINT('Ctrl Pts',(6.39898060511237,-3.95355296513967,15.7221256451606));
#63420=CARTESIAN_POINT('Ctrl Pts',(6.43981311987819,-3.97422893257098,15.6906354985908));
#63421=CARTESIAN_POINT('Ctrl Pts',(6.46987737873425,-3.98945228191695,15.6674498602994));
#63422=CARTESIAN_POINT('Ctrl Pts',(6.49942273048966,-4.00637382707713,15.64350052591));
#63423=CARTESIAN_POINT('Ctrl Pts',(6.52825572691364,-4.02500083391913,15.6188233092075));
#63424=CARTESIAN_POINT('Ctrl Pts',(6.53601349370777,-4.0300125910403,15.6121836908519));
#63425=CARTESIAN_POINT('Ctrl Pts',(6.54371960345473,-4.03514781599872,15.6054914107273));
#63426=CARTESIAN_POINT('Ctrl Pts',(6.55137068364015,-4.04040583335116,15.5987473160714));
#63427=CARTESIAN_POINT('Ctrl Pts',(6.58876385834978,-4.06610337627599,15.5657868577292));
#63428=CARTESIAN_POINT('Ctrl Pts',(6.6248461275891,-4.09473439723206,15.5315871554488));
#63429=CARTESIAN_POINT('Ctrl Pts',(6.65919837855307,-4.12621552301973,15.4962590980255));
#63430=CARTESIAN_POINT('Ctrl Pts',(6.67729063309629,-4.14279564586684,15.4776529167861));
#63431=CARTESIAN_POINT('Ctrl Pts',(6.6949022981319,-4.16016622314613,15.458734086895));
#63432=CARTESIAN_POINT('Ctrl Pts',(6.71196671988954,-4.1783148174862,15.4395211563086));
#63433=CARTESIAN_POINT('Ctrl Pts',(6.72110227292727,-4.18803078961281,15.4292353846091));
#63434=CARTESIAN_POINT('Ctrl Pts',(6.7300809057676,-4.19796975487159,15.4188653497671));
#63435=CARTESIAN_POINT('Ctrl Pts',(6.73889398719123,-4.20812767161503,15.4084142443932));
#63436=CARTESIAN_POINT('Ctrl Pts',(6.74831600968466,-4.21898745100916,15.39724101846));
#63437=CARTESIAN_POINT('Ctrl Pts',(6.75754881892868,-4.23009748370278,15.3859751293313));
#63438=CARTESIAN_POINT('Ctrl Pts',(6.76658149289953,-4.24145275839218,15.374620672648));
#63439=CARTESIAN_POINT('Ctrl Pts',(6.77109782988495,-4.24713039573687,15.3689434443064));
#63440=CARTESIAN_POINT('Ctrl Pts',(6.77556412974877,-4.25286934629214,15.363244074211));
#63441=CARTESIAN_POINT('Ctrl Pts',(6.77997898367324,-4.25866897270543,15.3575230980767));
#63442=CARTESIAN_POINT('Ctrl Pts',(6.7826892751254,-4.26222937994938,15.354010974464));
#63443=CARTESIAN_POINT('Ctrl Pts',(6.78572125911814,-4.26626855845317,15.3500426898254));
#63444=CARTESIAN_POINT('Ctrl Pts',(6.78844385144841,-4.26994887684661,15.346443289757));
#63445=CARTESIAN_POINT('Ctrl Pts',(6.79015615021608,-4.2722635108003,15.3441795471346));
#63446=CARTESIAN_POINT('Ctrl Pts',(6.79174708784231,-4.27443533134104,15.3420617997071));
#63447=CARTESIAN_POINT('Ctrl Pts',(6.79306778194254,-4.27624925256168,15.3402958895932));
#63448=CARTESIAN_POINT('Ctrl Pts',(6.8107996753019,-4.30060330823675,15.3165864402844));
#63449=CARTESIAN_POINT('Ctrl Pts',(6.82812764703875,-4.3266456655919,15.2918342165974));
#63450=CARTESIAN_POINT('Ctrl Pts',(6.84476100521714,-4.35446256236332,15.2660735832892));
#63451=CARTESIAN_POINT('Ctrl Pts',(6.84876408758397,-4.36115714127947,15.2598738769011));
#63452=CARTESIAN_POINT('Ctrl Pts',(6.85272673262482,-4.3679544288046,15.2536158504336));
#63453=CARTESIAN_POINT('Ctrl Pts',(6.85664448175611,-4.37485548642977,15.2473001551339));
#63454=CARTESIAN_POINT('Ctrl Pts',(6.87220142998755,-4.40225882253399,15.2222212280432));
#63455=CARTESIAN_POINT('Ctrl Pts',(6.88705311840915,-4.43130038235405,15.1962313701704));
#63456=CARTESIAN_POINT('Ctrl Pts',(6.90092818336887,-4.46200529431339,15.1693865861704));
#63457=CARTESIAN_POINT('Ctrl Pts',(6.91385297148164,-4.49060728516875,15.1443803504418));
#63458=CARTESIAN_POINT('Ctrl Pts',(6.92593042278619,-4.52065243222546,15.1186323058424));
#63459=CARTESIAN_POINT('Ctrl Pts',(6.93691038409135,-4.55214103784724,15.0922053172018));
#63460=CARTESIAN_POINT('Ctrl Pts',(6.94301470875026,-4.56964717165131,15.0775131963522));
#63461=CARTESIAN_POINT('Ctrl Pts',(6.94877927141611,-4.58759914596029,15.0626115450918));
#63462=CARTESIAN_POINT('Ctrl Pts',(6.95415625565575,-4.60599427316238,15.0475137604011));
#63463=CARTESIAN_POINT('Ctrl Pts',(6.96384063454289,-4.63912536924945,15.0203214420337));
#63464=CARTESIAN_POINT('Ctrl Pts',(6.97226953626585,-4.67369588112642,14.9924914495598));
#63465=CARTESIAN_POINT('Ctrl Pts',(6.9791776980466,-4.70964222664831,14.96412246903));
#63466=CARTESIAN_POINT('Ctrl Pts',(6.98573847263594,-4.74378095671348,14.9371800648866));
#63467=CARTESIAN_POINT('Ctrl Pts',(6.99092794841612,-4.77916047790126,14.9097514970841));
#63468=CARTESIAN_POINT('Ctrl Pts',(6.99448542380503,-4.81570149995584,14.8819428905447));
#63469=CARTESIAN_POINT('Ctrl Pts',(6.99588982850059,-4.83012700606452,14.8709647295368));
#63470=CARTESIAN_POINT('Ctrl Pts',(6.99703948106122,-4.84473325899142,14.8599275875814));
#63471=CARTESIAN_POINT('Ctrl Pts',(6.99791659494413,-4.85951430546009,14.8488390072659));
#63472=CARTESIAN_POINT('Ctrl Pts',(6.99928002608722,-4.88249072787875,14.8316023450382));
#63473=CARTESIAN_POINT('Ctrl Pts',(6.99998508666163,-4.90588992273367,14.8142411383093));
#63474=CARTESIAN_POINT('Ctrl Pts',(6.99997879767476,-4.9296673590521,14.7967908137217));
#63475=CARTESIAN_POINT('Ctrl Pts',(6.99990231887239,-4.95610622131399,14.6847031539405));
#63476=CARTESIAN_POINT('Ctrl Pts',(6.99990231887239,-4.91841584418849,15.0109950436589));
#63477=CARTESIAN_POINT('Ctrl Pts',(6.99990231887239,-4.85614473463976,15.898877282419));
#63478=CARTESIAN_POINT('Ctrl Pts',(6.99990231887239,-4.92998658103204,17.3517289669861));
#63479=CARTESIAN_POINT('Ctrl Pts',(6.99990231887239,-5.27368488295105,19.005709054627));
#63480=CARTESIAN_POINT('Ctrl Pts',(6.99990231887239,-5.86659897824408,20.5902694345695));
#63481=CARTESIAN_POINT('Ctrl Pts',(6.99990231887239,-6.69608062393941,22.0651427870248));
#63482=CARTESIAN_POINT('Ctrl Pts',(6.99990231887239,-7.73956505901654,23.3944794780462));
#63483=CARTESIAN_POINT('Ctrl Pts',(6.99990231887239,-8.69529347682775,24.2870566144972));
#63484=CARTESIAN_POINT('Ctrl Pts',(6.99990231887239,-9.28610929960213,24.7366528371348));
#63485=CARTESIAN_POINT('Ctrl Pts',(6.99990231887239,-9.4330769651433,24.8428619308663));
#63486=CARTESIAN_POINT('Ctrl Pts',(7.00659605346157,-4.4803994227663,14.6297385385056));
#63487=CARTESIAN_POINT('Ctrl Pts',(7.00659605346157,-4.44105701581783,14.9703190744433));
#63488=CARTESIAN_POINT('Ctrl Pts',(7.00659605346157,-4.37608979545098,15.8968441454591));
#63489=CARTESIAN_POINT('Ctrl Pts',(7.00659605346157,-4.45313232990638,17.4128498125714));
#63490=CARTESIAN_POINT('Ctrl Pts',(7.00659605346157,-4.8118677809658,19.1393645192062));
#63491=CARTESIAN_POINT('Ctrl Pts',(7.00659605346157,-5.43067059711262,20.792955990879));
#63492=CARTESIAN_POINT('Ctrl Pts',(7.00659605346157,-6.29622676552029,22.3320796939897));
#63493=CARTESIAN_POINT('Ctrl Pts',(7.00659605346157,-7.38549375785552,23.7196853446899));
#63494=CARTESIAN_POINT('Ctrl Pts',(7.00659605346157,-8.38271691158709,24.6510011090022));
#63495=CARTESIAN_POINT('Ctrl Pts',(7.00659605346157,-8.99921657562843,25.1201522854231));
#63496=CARTESIAN_POINT('Ctrl Pts',(7.00659605346157,-9.15258727145085,25.2309895948636));
#63497=CARTESIAN_POINT('Ctrl Pts',(6.71662481110376,-4.10164945528999,14.5859766112628));
#63498=CARTESIAN_POINT('Ctrl Pts',(6.71662481110376,-4.06099172923174,14.9379335334627));
#63499=CARTESIAN_POINT('Ctrl Pts',(6.71662481110376,-3.99387790955452,15.8952253950789));
#63500=CARTESIAN_POINT('Ctrl Pts',(6.71662481110376,-4.07346877946317,17.4615132295016));
#63501=CARTESIAN_POINT('Ctrl Pts',(6.71662481110376,-4.4441765625702,19.2457788126714));
#63502=CARTESIAN_POINT('Ctrl Pts',(6.71662481110376,-5.08359155456183,20.9543317098043));
#63503=CARTESIAN_POINT('Ctrl Pts',(6.71662481110376,-5.97786966754659,22.5446104905642));
#63504=CARTESIAN_POINT('Ctrl Pts',(6.71662481110376,-7.10358798268114,23.9786089333139));
#63505=CARTESIAN_POINT('Ctrl Pts',(6.71662481110376,-8.13384856604163,24.9407677591288));
#63506=CARTESIAN_POINT('Ctrl Pts',(6.71662481110376,-8.77079728415514,25.4254882697159));
#63507=CARTESIAN_POINT('Ctrl Pts',(6.71662481110376,-8.9292659678921,25.5400104887542));
#63508=CARTESIAN_POINT('Ctrl Pts',(6.2531283899648,-3.98117651752108,14.5720568003314));
#63509=CARTESIAN_POINT('Ctrl Pts',(6.2531283899648,-3.94010041424707,14.9276323279248));
#63510=CARTESIAN_POINT('Ctrl Pts',(6.2531283899648,-3.87230380342307,15.8947105023297));
#63511=CARTESIAN_POINT('Ctrl Pts',(6.2531283899648,-3.95270524886919,17.4769921081946));
#63512=CARTESIAN_POINT('Ctrl Pts',(6.2531283899648,-4.3272211960331,19.2796271127503));
#63513=CARTESIAN_POINT('Ctrl Pts',(6.2531283899648,-4.97319251697744,21.0056621615854));
#63514=CARTESIAN_POINT('Ctrl Pts',(6.2531283899648,-5.8766065173295,22.6122123694565));
#63515=CARTESIAN_POINT('Ctrl Pts',(6.2531283899648,-7.01391928347156,24.060967449636));
#63516=CARTESIAN_POINT('Ctrl Pts',(6.2531283899648,-8.05468842536693,25.0329368485149));
#63517=CARTESIAN_POINT('Ctrl Pts',(6.2531283899648,-8.69814158659636,25.5226096590011));
#63518=CARTESIAN_POINT('Ctrl Pts',(6.2531283899648,-8.85823184032323,25.6383039755253));
#63519=CARTESIAN_POINT('Ctrl Pts',(6.99999999975185,-4.9296673620658,14.796790812935));
#63520=CARTESIAN_POINT('Ctrl Pts',(6.99999999975348,-4.91224345485887,14.9628120759864));
#63521=CARTESIAN_POINT('Ctrl Pts',(6.99999999939381,-4.89864382295723,15.1287094595423));
#63522=CARTESIAN_POINT('Ctrl Pts',(6.99999999871008,-4.88880665235693,15.2945618318709));
#63523=CARTESIAN_POINT('Ctrl Pts',(6.99999999819781,-4.8814362670729,15.4188247865357));
#63524=CARTESIAN_POINT('Ctrl Pts',(6.99999999754847,-4.87617905224362,15.5430627452601));
#63525=CARTESIAN_POINT('Ctrl Pts',(6.99999999746782,-4.87302807566252,15.6673106186318));
#63526=CARTESIAN_POINT('Ctrl Pts',(6.99999999735979,-4.86880791455303,15.8337180893462));
#63527=CARTESIAN_POINT('Ctrl Pts',(6.9999999991915,-4.86836396390667,16.0001436878221));
#63528=CARTESIAN_POINT('Ctrl Pts',(6.99999999987961,-4.87172632728565,16.1667041269997));
#63529=CARTESIAN_POINT('Ctrl Pts',(6.99999999995425,-4.87209105600973,16.1847715901549));
#63530=CARTESIAN_POINT('Ctrl Pts',(7.00000000000036,-4.87250062239559,16.2028406354215));
#63531=CARTESIAN_POINT('Ctrl Pts',(7.00000000000036,-4.87295510160001,16.2209114079065));
#63532=CARTESIAN_POINT('Ctrl Pts',(7.00000000000036,-4.87820855291204,16.4297964844935));
#63533=CARTESIAN_POINT('Ctrl Pts',(6.99999999546741,-4.88938134704181,16.6388913171613));
#63534=CARTESIAN_POINT('Ctrl Pts',(6.99999999503646,-4.90651884891385,16.8476332056095));
#63535=CARTESIAN_POINT('Ctrl Pts',(6.99999999469247,-4.92019849279632,17.0142569480107));
#63536=CARTESIAN_POINT('Ctrl Pts',(6.99999999635954,-4.93767767490601,17.1806555717337));
#63537=CARTESIAN_POINT('Ctrl Pts',(6.99999999805387,-4.95895561846968,17.3465427176031));
#63538=CARTESIAN_POINT('Ctrl Pts',(6.99999999906433,-4.97164527214146,17.4454738207608));
#63539=CARTESIAN_POINT('Ctrl Pts',(7.00000000000036,-4.98568560133477,17.5442230216286));
#63540=CARTESIAN_POINT('Ctrl Pts',(7.00000000000036,-5.00106284847129,17.642730538889));
#63541=CARTESIAN_POINT('Ctrl Pts',(7.00000000000036,-5.04223781721342,17.9064997238446));
#63542=CARTESIAN_POINT('Ctrl Pts',(6.99999999769855,-5.09308746630109,18.1685325852661));
#63543=CARTESIAN_POINT('Ctrl Pts',(6.99999999858985,-5.15338945476548,18.4283220865757));
#63544=CARTESIAN_POINT('Ctrl Pts',(6.99999999924453,-5.19768253375072,18.6191429399849));
#63545=CARTESIAN_POINT('Ctrl Pts',(6.99999999995143,-5.24707642416826,18.8087537576797));
#63546=CARTESIAN_POINT('Ctrl Pts',(6.999999999996,-5.30150085813403,18.9969550513234));
#63547=CARTESIAN_POINT('Ctrl Pts',(6.99999999999901,-5.30518090424346,19.0096807590248));
#63548=CARTESIAN_POINT('Ctrl Pts',(7.00000000000036,-5.30888395639083,19.0224000221251));
#63549=CARTESIAN_POINT('Ctrl Pts',(7.00000000000036,-5.31260999009508,19.0351127794273));
#63550=CARTESIAN_POINT('Ctrl Pts',(7.00000000000036,-5.41493715266357,19.3842401589443));
#63551=CARTESIAN_POINT('Ctrl Pts',(6.99999999999506,-5.53457243760421,19.7284577210467));
#63552=CARTESIAN_POINT('Ctrl Pts',(6.99999999997255,-5.67103026820396,20.0659276985029));
#63553=CARTESIAN_POINT('Ctrl Pts',(6.99999999996562,-5.71306956633135,20.1698938903218));
#63554=CARTESIAN_POINT('Ctrl Pts',(7.00000000000035,-5.75670516944874,20.2732194901111));
#63555=CARTESIAN_POINT('Ctrl Pts',(7.00000000000035,-5.80192197421819,20.3758503481523));
#63556=CARTESIAN_POINT('Ctrl Pts',(7.00000000000035,-5.83171073986062,20.4434634091251));
#63557=CARTESIAN_POINT('Ctrl Pts',(6.99999999997079,-5.86218350081567,20.510776266759));
#63558=CARTESIAN_POINT('Ctrl Pts',(6.9999999999295,-5.89333513423436,20.5777738225602));
#63559=CARTESIAN_POINT('Ctrl Pts',(6.99999999970464,-6.06295587913339,20.942575730976));
#63560=CARTESIAN_POINT('Ctrl Pts',(7.00000000000036,-6.25270756111132,21.2980264726989));
#63561=CARTESIAN_POINT('Ctrl Pts',(7.00000000000036,-6.46120307607831,21.6419501662451));
#63562=CARTESIAN_POINT('Ctrl Pts',(7.00000000000036,-6.54468519845901,21.7796580679176));
#63563=CARTESIAN_POINT('Ctrl Pts',(6.99999999962042,-6.63117389391976,21.9155174566697));
#63564=CARTESIAN_POINT('Ctrl Pts',(6.99999999912255,-6.72060835796162,22.0494162477555));
#63565=CARTESIAN_POINT('Ctrl Pts',(6.99999999824675,-6.87793233894469,22.2849573346076));
#63566=CARTESIAN_POINT('Ctrl Pts',(6.9999999988619,-7.04437018592607,22.5144339817016));
#63567=CARTESIAN_POINT('Ctrl Pts',(6.99999999981869,-7.21957967785347,22.7372465183685));
#63568=CARTESIAN_POINT('Ctrl Pts',(6.99999999992587,-7.23920763462172,22.7622072370432));
#63569=CARTESIAN_POINT('Ctrl Pts',(7.00000000000036,-7.25894570336743,22.7870842781222));
#63570=CARTESIAN_POINT('Ctrl Pts',(7.00000000000036,-7.27879342491422,22.811876764014));
#63571=CARTESIAN_POINT('Ctrl Pts',(7.00000000000036,-7.41703735932601,22.9845621166103));
#63572=CARTESIAN_POINT('Ctrl Pts',(6.99999999634334,-7.56056958524369,23.1531795030631));
#63573=CARTESIAN_POINT('Ctrl Pts',(6.99999999541996,-7.70901246660694,23.3172462117123));
#63574=CARTESIAN_POINT('Ctrl Pts',(6.99999999531015,-7.72666492377434,23.3367566154476));
#63575=CARTESIAN_POINT('Ctrl Pts',(6.99999999523504,-7.74438678100536,23.3562027086881));
#63576=CARTESIAN_POINT('Ctrl Pts',(6.99999999519958,-7.76217736879295,23.3755837147586));
#63577=CARTESIAN_POINT('Ctrl Pts',(6.99999999489101,-7.91698551942648,23.5442311896495));
#63578=CARTESIAN_POINT('Ctrl Pts',(7.00000000000036,-8.07700088558281,23.7079464463786));
#63579=CARTESIAN_POINT('Ctrl Pts',(7.00000000000036,-8.24167851282883,23.8663282373223));
#63580=CARTESIAN_POINT('Ctrl Pts',(7.00000000000036,-8.36437153139225,23.9843305448691));
#63581=CARTESIAN_POINT('Ctrl Pts',(6.99999999741532,-8.48968648772239,24.0993265809265));
#63582=CARTESIAN_POINT('Ctrl Pts',(6.99999999745853,-8.61766942749797,24.2114123910189));
#63583=CARTESIAN_POINT('Ctrl Pts',(6.99999999749976,-8.73980227281244,24.3183747637381));
#63584=CARTESIAN_POINT('Ctrl Pts',(6.99999999865195,-8.86436525968121,24.4226868685668));
#63585=CARTESIAN_POINT('Ctrl Pts',(6.99999999924104,-8.99142942748623,24.5244006129468));
#63586=CARTESIAN_POINT('Ctrl Pts',(6.9999999997591,-9.10317157848991,24.6138492181672));
#63587=CARTESIAN_POINT('Ctrl Pts',(6.99999999990898,-9.2168486419286,24.7012880171126));
#63588=CARTESIAN_POINT('Ctrl Pts',(6.99999999989432,-9.33251047983013,24.7867157006585));
#63589=CARTESIAN_POINT('Ctrl Pts',(6.26386081957825,-3.90572621560986,15.814440855933));
#63590=CARTESIAN_POINT('Ctrl Pts',(6.26460716030619,-3.90306652820293,16.0736422380589));
#63591=CARTESIAN_POINT('Ctrl Pts',(6.26531569223296,-3.90881658977334,16.3306845724835));
#63592=CARTESIAN_POINT('Ctrl Pts',(6.2659863977903,-3.92256349692468,16.5850748047761));
#63593=CARTESIAN_POINT('Ctrl Pts',(6.26666475020584,-3.93646713551864,16.8423653947753));
#63594=CARTESIAN_POINT('Ctrl Pts',(6.26730440882618,-3.95855099096231,17.096943119821));
#63595=CARTESIAN_POINT('Ctrl Pts',(6.2679053588221,-3.98839441038359,17.3483506398906));
#63596=CARTESIAN_POINT('Ctrl Pts',(6.26800177816493,-3.99318263387662,17.3886876862903));
#63597=CARTESIAN_POINT('Ctrl Pts',(6.26809720105533,-3.99817062217637,17.4289432315441));
#63598=CARTESIAN_POINT('Ctrl Pts',(6.26819162743929,-4.00335665371818,17.4691155096931));
#63599=CARTESIAN_POINT('Ctrl Pts',(6.26876871870475,-4.0350513282325,17.7146302679753));
#63600=CARTESIAN_POINT('Ctrl Pts',(6.26930858925204,-4.07414146028354,17.9570309131006));
#63601=CARTESIAN_POINT('Ctrl Pts',(6.26981122824073,-4.12011022476256,18.1959089254361));
#63602=CARTESIAN_POINT('Ctrl Pts',(6.27017913019625,-4.15375663645253,18.3707534755957));
#63603=CARTESIAN_POINT('Ctrl Pts',(6.27052708587458,-4.19108861036826,18.5437118696551));
#63604=CARTESIAN_POINT('Ctrl Pts',(6.27085509181305,-4.23191018794964,18.7146402529524));
#63605=CARTESIAN_POINT('Ctrl Pts',(6.27121137657533,-4.27625117193226,18.9003051183254));
#63606=CARTESIAN_POINT('Ctrl Pts',(6.27154412268532,-4.32470931376187,19.08357463927));
#63607=CARTESIAN_POINT('Ctrl Pts',(6.27185332606288,-4.37704085982857,19.2642821899259));
#63608=CARTESIAN_POINT('Ctrl Pts',(6.27227096752176,-4.44772515641576,19.5083641455751));
#63609=CARTESIAN_POINT('Ctrl Pts',(6.27264565767329,-4.52547485758646,19.7477703759114));
#63610=CARTESIAN_POINT('Ctrl Pts',(6.27297738858458,-4.60968094217816,19.9821807438504));
#63611=CARTESIAN_POINT('Ctrl Pts',(6.27330911949587,-4.69388702676985,20.2165911117894));
#63612=CARTESIAN_POINT('Ctrl Pts',(6.27359789118611,-4.78454955978446,20.4460058025126));
#63613=CARTESIAN_POINT('Ctrl Pts',(6.27384369786499,-4.8810873310656,20.6701561528923));
#63614=CARTESIAN_POINT('Ctrl Pts',(6.27395596416794,-4.92517864187066,20.7725314473961));
#63615=CARTESIAN_POINT('Ctrl Pts',(6.27405926809239,-4.97049589580692,20.8738092985562));
#63616=CARTESIAN_POINT('Ctrl Pts',(6.27415361626388,-5.01698560251817,20.9739675362492));
#63617=CARTESIAN_POINT('Ctrl Pts',(6.27415652037485,-5.0184165922798,20.9770504856335));
#63618=CARTESIAN_POINT('Ctrl Pts',(6.27415941593985,-5.01984869290736,20.9801323742789));
#63619=CARTESIAN_POINT('Ctrl Pts',(6.27416230296468,-5.02128190286476,20.9832132015813));
#63620=CARTESIAN_POINT('Ctrl Pts',(6.27420631248003,-5.04312961089931,21.0301770222397));
#63621=CARTESIAN_POINT('Ctrl Pts',(6.27424833746245,-5.06523509446001,21.076894204489));
#63622=CARTESIAN_POINT('Ctrl Pts',(6.2742883985241,-5.0875921193759,21.1233630648912));
#63623=CARTESIAN_POINT('Ctrl Pts',(6.27431785022144,-5.10402833709297,21.1575255847035));
#63624=CARTESIAN_POINT('Ctrl Pts',(6.27434670120188,-5.12089353968899,21.192152832586));
#63625=CARTESIAN_POINT('Ctrl Pts',(6.27437398730189,-5.1375803959525,21.2260036828553));
#63626=CARTESIAN_POINT('Ctrl Pts',(6.27438625132226,-5.145080476395,21.2412182982423));
#63627=CARTESIAN_POINT('Ctrl Pts',(6.27439819921371,-5.15254388406323,21.256276383525));
#63628=CARTESIAN_POINT('Ctrl Pts',(6.27440974343164,-5.15991241649642,21.2710667690669));
#63629=CARTESIAN_POINT('Ctrl Pts',(6.27456064753034,-5.25623264816907,21.4644042314235));
#63630=CARTESIAN_POINT('Ctrl Pts',(6.27467736557741,-5.35907886487503,21.6577055885389));
#63631=CARTESIAN_POINT('Ctrl Pts',(6.2747598958331,-5.46870158665621,21.8504720742369));
#63632=CARTESIAN_POINT('Ctrl Pts',(6.27484107259586,-5.5765265001261,22.0400771971764));
#63633=CARTESIAN_POINT('Ctrl Pts',(6.27488917373459,-5.69090753982229,22.2291648994148));
#63634=CARTESIAN_POINT('Ctrl Pts',(6.27490419856597,-5.81206786878456,22.4172123727217));
#63635=CARTESIAN_POINT('Ctrl Pts',(6.27490863259839,-5.84782393232077,22.4727077436981));
#63636=CARTESIAN_POINT('Ctrl Pts',(6.27491018595364,-5.88417031203136,22.5281121924229));
#63637=CARTESIAN_POINT('Ctrl Pts',(6.27490885862982,-5.92111247084116,22.583411450356));
#63638=CARTESIAN_POINT('Ctrl Pts',(6.27490450996821,-6.04214469049153,22.7645863504783));
#63639=CARTESIAN_POINT('Ctrl Pts',(6.27486924032986,-6.16957355860617,22.9446356521944));
#63640=CARTESIAN_POINT('Ctrl Pts',(6.2748030501825,-6.30354337953915,23.1230248298937));
#63641=CARTESIAN_POINT('Ctrl Pts',(6.27475277160487,-6.40530795191046,23.2585307091866));
#63642=CARTESIAN_POINT('Ctrl Pts',(6.27468465176775,-6.51084628860725,23.3930777864523));
#63643=CARTESIAN_POINT('Ctrl Pts',(6.27459869119746,-6.62021326700212,23.5264134452897));
#63644=CARTESIAN_POINT('Ctrl Pts',(6.27448994699812,-6.75856768297465,23.6950893790818));
#63645=CARTESIAN_POINT('Ctrl Pts',(6.27435265036365,-6.90304997541691,23.8618280950501));
#63646=CARTESIAN_POINT('Ctrl Pts',(6.2741868037742,-7.05375344156325,24.0260801484426));
#63647=CARTESIAN_POINT('Ctrl Pts',(6.27401315425445,-7.21154736790509,24.1980601106643));
#63648=CARTESIAN_POINT('Ctrl Pts',(6.27380820507056,-7.37616248254101,24.3673132447826));
#63649=CARTESIAN_POINT('Ctrl Pts',(6.27357196000059,-7.54763091708786,24.5332701712914));
#63650=CARTESIAN_POINT('Ctrl Pts',(6.27333930797839,-7.71649149075496,24.6967030613646));
#63651=CARTESIAN_POINT('Ctrl Pts',(6.27307630478399,-7.89199856689717,24.8569392626461));
#63652=CARTESIAN_POINT('Ctrl Pts',(6.27278295501666,-8.0741504976575,25.0133963364823));
#63653=CARTESIAN_POINT('Ctrl Pts',(6.27261682411597,-8.17730743756334,25.1020016721282));
#63654=CARTESIAN_POINT('Ctrl Pts',(6.27244096040682,-8.2825949371111,25.1893942510749));
#63655=CARTESIAN_POINT('Ctrl Pts',(6.27225536487834,-8.39000786644608,25.2754626135137));
#63656=CARTESIAN_POINT('Ctrl Pts',(6.27204648957659,-8.51089390399926,25.3723267746377));
#63657=CARTESIAN_POINT('Ctrl Pts',(6.27182528795732,-8.63447217814325,25.467513907671));
#63658=CARTESIAN_POINT('Ctrl Pts',(6.27159176161367,-8.76072156035792,25.5608443099372));
#63659=CARTESIAN_POINT('Ctrl Pts',(-6.390310997314,-3.94960676120434,15.4604112548065));
#63660=CARTESIAN_POINT('Ctrl Pts',(-4.260207331542,-3.32899290723404,16.2184975538162));
#63661=CARTESIAN_POINT('Ctrl Pts',(0.0001535201380647,-2.70682847609605,
16.976602560809));
#63662=CARTESIAN_POINT('Ctrl Pts',(4.260514371819,-3.32903774766832,16.2184429159229));
#63663=CARTESIAN_POINT('Ctrl Pts',(6.390771557728,-3.949740952065,15.4602473392485));
#63664=CARTESIAN_POINT('Ctrl Pts',(-6.390310997314,-3.91824203061707,16.2404119010483));
#63665=CARTESIAN_POINT('Ctrl Pts',(-4.260207331542,-3.34435482128984,16.9591696862112));
#63666=CARTESIAN_POINT('Ctrl Pts',(0.0001535201380647,-2.7685203922099,
17.6779350698092));
#63667=CARTESIAN_POINT('Ctrl Pts',(4.260514371819,-3.34439632263995,16.9591178835817));
#63668=CARTESIAN_POINT('Ctrl Pts',(6.390771557728,-3.9183661181109,16.2402564892191));
#63669=CARTESIAN_POINT('Ctrl Pts',(-6.390310997314,-4.02653939109499,18.1258674862954));
#63670=CARTESIAN_POINT('Ctrl Pts',(-4.260207331542,-3.53814955008341,18.7395147188676));
#63671=CARTESIAN_POINT('Ctrl Pts',(0.0001535201380647,-3.05107310998534,
19.3531400775061));
#63672=CARTESIAN_POINT('Ctrl Pts',(4.260514371819,-3.53818465449488,18.7394704938521));
#63673=CARTESIAN_POINT('Ctrl Pts',(6.390771557728,-4.02664499212973,18.1257348017601));
#63674=CARTESIAN_POINT('Ctrl Pts',(-6.390310997314,-4.89945800151002,21.0044951210507));
#63675=CARTESIAN_POINT('Ctrl Pts',(-4.260207331542,-4.44478850539311,21.4424839510742));
#63676=CARTESIAN_POINT('Ctrl Pts',(0.0001535201380647,-3.98943347064956,
21.8807678511962));
#63677=CARTESIAN_POINT('Ctrl Pts',(4.260514371819,-4.44482132359356,21.4424523632204));
#63678=CARTESIAN_POINT('Ctrl Pts',(6.390771557728,-4.89955631142349,21.0044004178757));
#63679=CARTESIAN_POINT('Ctrl Pts',(-6.390310997314,-6.63374323540806,23.7052269015879));
#63680=CARTESIAN_POINT('Ctrl Pts',(-4.260207331542,-6.0952579924294,23.9981305004778));
#63681=CARTESIAN_POINT('Ctrl Pts',(0.0001535201380647,-5.55782051180541,
24.2900535316613));
#63682=CARTESIAN_POINT('Ctrl Pts',(4.260514371819,-6.09529672644794,23.9981094610928));
#63683=CARTESIAN_POINT('Ctrl Pts',(6.390771557728,-6.63385966821385,23.7051635691471));
#63684=CARTESIAN_POINT('Ctrl Pts',(-6.390310997314,-8.18394441798506,25.1149801838822));
#63685=CARTESIAN_POINT('Ctrl Pts',(-4.260207331542,-7.53598553401078,25.3660543259899));
#63686=CARTESIAN_POINT('Ctrl Pts',(0.0001535201380647,-6.88615455534451,
25.6190325570298));
#63687=CARTESIAN_POINT('Ctrl Pts',(4.260514371819,-7.536032368418,25.366036093427));
#63688=CARTESIAN_POINT('Ctrl Pts',(6.390771557728,-8.18408452146462,25.1149258959381));
#63689=CARTESIAN_POINT('Ctrl Pts',(-6.390310997314,-8.98425336235418,25.6807325212854));
#63690=CARTESIAN_POINT('Ctrl Pts',(-4.260207331542,-8.27686663367918,25.9287944450768));
#63691=CARTESIAN_POINT('Ctrl Pts',(0.0001535201380647,-7.56887097380373,
26.1774616570061));
#63692=CARTESIAN_POINT('Ctrl Pts',(4.260514371819,-8.2769176601128,25.9287765232156));
#63693=CARTESIAN_POINT('Ctrl Pts',(6.390771557728,-8.9844063154964,25.680678884635));
#63694=CARTESIAN_POINT('Ctrl Pts',(-6.26386060032414,-3.90573753027274,
15.8144217558848));
#63695=CARTESIAN_POINT('Ctrl Pts',(-5.97426230930331,-3.82545376840559,
15.9107534531458));
#63696=CARTESIAN_POINT('Ctrl Pts',(-5.68272415002883,-3.75014409027891,
15.9997900251984));
#63697=CARTESIAN_POINT('Ctrl Pts',(-5.38973713287711,-3.68009451384404,
16.0816096133529));
#63698=CARTESIAN_POINT('Ctrl Pts',(-5.1148963508353,-3.61438347805748,16.1583616818006));
#63699=CARTESIAN_POINT('Ctrl Pts',(-4.8387806239847,-3.55330174463071,16.2287627175083));
#63700=CARTESIAN_POINT('Ctrl Pts',(-4.56179526395762,-3.49706393515746,
16.2929147389837));
#63701=CARTESIAN_POINT('Ctrl Pts',(-4.30450523531574,-3.44482497347112,
16.3525051644172));
#63702=CARTESIAN_POINT('Ctrl Pts',(-4.04646484891085,-3.39676582845628,
16.4067035756603));
#63703=CARTESIAN_POINT('Ctrl Pts',(-3.78799895819672,-3.35303372379852,
16.4556278903896));
#63704=CARTESIAN_POINT('Ctrl Pts',(-3.57232101449432,-3.31654128612985,
16.4964529894721));
#63705=CARTESIAN_POINT('Ctrl Pts',(-3.35634678627636,-3.28306154818238,
16.5336061380409));
#63706=CARTESIAN_POINT('Ctrl Pts',(-3.14026502702693,-3.25266330082624,
16.5671782502199));
#63707=CARTESIAN_POINT('Ctrl Pts',(-2.90080112829706,-3.21897566864598,
16.6043831901413));
#63708=CARTESIAN_POINT('Ctrl Pts',(-2.66120552935244,-3.18907472968854,
16.6372138404118));
#63709=CARTESIAN_POINT('Ctrl Pts',(-2.42172500293894,-3.16301823790052,
16.6656906330402));
#63710=CARTESIAN_POINT('Ctrl Pts',(-2.18568576270281,-3.13733617256948,
16.6937582199836));
#63711=CARTESIAN_POINT('Ctrl Pts',(-1.94975831162179,-3.11538890068632,
16.7175961664648));
#63712=CARTESIAN_POINT('Ctrl Pts',(-1.71417893635696,-3.09719944592268,
16.737263052464));
#63713=CARTESIAN_POINT('Ctrl Pts',(-1.4801385381641,-3.0791288180037,16.7568014599553));
#63714=CARTESIAN_POINT('Ctrl Pts',(-1.24644168286964,-3.06476712988494,
16.7722230853077));
#63715=CARTESIAN_POINT('Ctrl Pts',(-1.01332005652778,-3.05410406159889,
16.7836246209729));
#63716=CARTESIAN_POINT('Ctrl Pts',(-0.781833519416523,-3.04351578289111,
16.7949461875317));
#63717=CARTESIAN_POINT('Ctrl Pts',(-0.5509141703719,-3.03657445544106,16.8023038449724));
#63718=CARTESIAN_POINT('Ctrl Pts',(-0.32078885450044,-3.03323674555433,
16.8058315010754));
#63719=CARTESIAN_POINT('Ctrl Pts',(-0.213870712629672,-3.03168601769182,
16.8074704795349));
#63720=CARTESIAN_POINT('Ctrl Pts',(-0.107123971484708,-3.03091269623866,
16.8082832675462));
#63721=CARTESIAN_POINT('Ctrl Pts',(-0.000571381538524201,-3.03090994562974,
16.8082862144943));
#63722=CARTESIAN_POINT('Ctrl Pts',(-0.000380921640730136,-3.0309099407131,
16.8082862197619));
#63723=CARTESIAN_POINT('Ctrl Pts',(-0.000190461127502138,-3.03090993825803,
16.8082862224426));
#63724=CARTESIAN_POINT('Ctrl Pts',(1.03384559906101E-12,-3.03090993826458,
16.8082862225363));
#63725=CARTESIAN_POINT('Ctrl Pts',(0.230288294953843,-3.0309099461773,16.8082863358534));
#63726=CARTESIAN_POINT('Ctrl Pts',(0.461476135630093,-3.03451153042456,
16.8045011076514));
#63727=CARTESIAN_POINT('Ctrl Pts',(0.693339238579527,-3.04177406743476,
16.7967768846798));
#63728=CARTESIAN_POINT('Ctrl Pts',(0.927160087319404,-3.04909792597943,
16.788987441909));
#63729=CARTESIAN_POINT('Ctrl Pts',(1.1616676496846,-3.06014480501952,16.7771922026878));
#63730=CARTESIAN_POINT('Ctrl Pts',(1.39663191288004,-3.07494113876898,16.7612740817315));
#63731=CARTESIAN_POINT('Ctrl Pts',(1.6331435537806,-3.08983491506843,16.7452511305974));
#63732=CARTESIAN_POINT('Ctrl Pts',(1.87011793060501,-3.10852764050927,16.7250508490044));
#63733=CARTESIAN_POINT('Ctrl Pts',(2.10732045625743,-3.13101204586718,16.7005944302589));
#63734=CARTESIAN_POINT('Ctrl Pts',(2.34747479622559,-3.15377625342971,16.6758336690247));
#63735=CARTESIAN_POINT('Ctrl Pts',(2.58786299864806,-3.18042705182343,16.6467102007614));
#63736=CARTESIAN_POINT('Ctrl Pts',(2.82824160919085,-3.21092262617489,16.613183394872));
#63737=CARTESIAN_POINT('Ctrl Pts',(2.93189543141303,-3.22407264328853,16.5987262783694));
#63738=CARTESIAN_POINT('Ctrl Pts',(3.03554747009574,-3.23793714373867,16.5834509066644));
#63739=CARTESIAN_POINT('Ctrl Pts',(3.13917820496035,-3.25251088491731,16.5673563184501));
#63740=CARTESIAN_POINT('Ctrl Pts',(3.40197375645711,-3.28946820607705,16.5265423051997));
#63741=CARTESIAN_POINT('Ctrl Pts',(3.66462147904948,-3.33098599837418,16.4804289673528));
#63742=CARTESIAN_POINT('Ctrl Pts',(3.92678119996645,-3.37693833074301,16.4288554486851));
#63743=CARTESIAN_POINT('Ctrl Pts',(4.19748597231201,-3.42438847155465,16.3756008999651));
#63744=CARTESIAN_POINT('Ctrl Pts',(4.4676704118551,-3.47656651974571,16.3165247605884));
#63745=CARTESIAN_POINT('Ctrl Pts',(4.73695998620211,-3.53329768778599,16.251498714715));
#63746=CARTESIAN_POINT('Ctrl Pts',(5.03194795561124,-3.59544273035955,16.1802672113141));
#63747=CARTESIAN_POINT('Ctrl Pts',(5.32586211575626,-3.66305099399998,16.1018960658767));
#63748=CARTESIAN_POINT('Ctrl Pts',(5.61821015094397,-3.73585595945423,16.0162717568522));
#63749=CARTESIAN_POINT('Ctrl Pts',(5.83434844010851,-3.78968201190525,15.9529681274928));
#63750=CARTESIAN_POINT('Ctrl Pts',(6.04963069831582,-3.84634765920576,15.8857012380644));
#63751=CARTESIAN_POINT('Ctrl Pts',(6.26385797816486,-3.90573660195549,15.8144409703668));
#63752=CARTESIAN_POINT('Ctrl Pts',(-6.38351709471616,-3.93920782693273,
15.7749258978406));
#63753=CARTESIAN_POINT('Ctrl Pts',(-6.08740745253563,-3.85548476926818,
15.881473813723));
#63754=CARTESIAN_POINT('Ctrl Pts',(-5.13142578697123,-3.60387668806693,
16.1968376701999));
#63755=CARTESIAN_POINT('Ctrl Pts',(-3.40211712930966,-3.25762303527195,
16.6110525573658));
#63756=CARTESIAN_POINT('Ctrl Pts',(-1.16426938927718,-3.02328203047528,
16.878951814368));
#63757=CARTESIAN_POINT('Ctrl Pts',(1.16113505781623,-3.02310888355152,16.8791462423432));
#63758=CARTESIAN_POINT('Ctrl Pts',(3.39945869805431,-3.25719731223483,16.6115486323221));
#63759=CARTESIAN_POINT('Ctrl Pts',(5.12988614343298,-3.6034988213486,16.1973036504942));
#63760=CARTESIAN_POINT('Ctrl Pts',(6.08676115286924,-3.85530247941335,15.8817056622505));
#63761=CARTESIAN_POINT('Ctrl Pts',(6.38348326401547,-3.93919827240965,15.7749380472911));
#63762=CARTESIAN_POINT('Ctrl Pts',(-6.17631081322735,-3.89089882940664,
15.1504194794343));
#63763=CARTESIAN_POINT('Ctrl Pts',(-5.88965655823781,-3.81103185421913,
15.2535318539487));
#63764=CARTESIAN_POINT('Ctrl Pts',(-4.96426339598262,-3.57096639928173,
15.5587423966376));
#63765=CARTESIAN_POINT('Ctrl Pts',(-3.29074409978021,-3.24047405664135,
15.95962814198));
#63766=CARTESIAN_POINT('Ctrl Pts',(-1.1260028682163,-3.01678341201172,16.218861585521));
#63767=CARTESIAN_POINT('Ctrl Pts',(1.12297142654902,-3.0166181415462,16.219049702787));
#63768=CARTESIAN_POINT('Ctrl Pts',(3.28817192979132,-3.24006767592172,15.9601082192533));
#63769=CARTESIAN_POINT('Ctrl Pts',(4.96277311007818,-3.5706058011467,15.5591933938224));
#63770=CARTESIAN_POINT('Ctrl Pts',(5.88903089909969,-3.81085796060267,15.2537562258459));
#63771=CARTESIAN_POINT('Ctrl Pts',(6.17627806349228,-3.89088971520562,15.1504312367114));
#63772=CARTESIAN_POINT('Ctrl Pts',(-6.17621381887775,-3.37750417917966,
14.7398362123642));
#63773=CARTESIAN_POINT('Ctrl Pts',(-5.89023958152254,-3.29860736714451,
14.841735137595));
#63774=CARTESIAN_POINT('Ctrl Pts',(-4.96677349652124,-3.06133287700747,
15.1434924061647));
#63775=CARTESIAN_POINT('Ctrl Pts',(-3.29476494977961,-2.73403327557292,
15.5405123166288));
#63776=CARTESIAN_POINT('Ctrl Pts',(-1.12803856271859,-2.51194808909339,
15.7978000261188));
#63777=CARTESIAN_POINT('Ctrl Pts',(1.12500219242395,-2.51178381698562,15.7979869150338));
#63778=CARTESIAN_POINT('Ctrl Pts',(3.29219295119216,-2.73363027885014,15.5409883200213));
#63779=CARTESIAN_POINT('Ctrl Pts',(4.96528590892401,-3.06097626156985,15.1439385253728));
#63780=CARTESIAN_POINT('Ctrl Pts',(5.8896153942606,-3.29843557903911,14.8419568740436));
#63781=CARTESIAN_POINT('Ctrl Pts',(6.17618114388549,-3.37749517511435,14.7398478327077));
#63782=CARTESIAN_POINT('Ctrl Pts',(-6.37985701943049,-2.76049912597563,
14.8225434715735));
#63783=CARTESIAN_POINT('Ctrl Pts',(-6.08546444017595,-2.67906593471349,
14.9262503141624));
#63784=CARTESIAN_POINT('Ctrl Pts',(-5.1344116261327,-2.43405279620404,15.2335227068454));
#63785=CARTESIAN_POINT('Ctrl Pts',(-3.40949469842141,-2.09538588962233,
15.6386468844809));
#63786=CARTESIAN_POINT('Ctrl Pts',(-1.16830514728113,-1.86490505714411,
15.9019381804586));
#63787=CARTESIAN_POINT('Ctrl Pts',(1.16516121475652,-1.86473433147697,15.9021296854872));
#63788=CARTESIAN_POINT('Ctrl Pts',(3.40683809148816,-2.09496825154861,15.6391333471311));
#63789=CARTESIAN_POINT('Ctrl Pts',(5.13287899229569,-2.43368435366994,15.2339772467715));
#63790=CARTESIAN_POINT('Ctrl Pts',(6.08482185993278,-2.67888861493498,14.9264759920189));
#63791=CARTESIAN_POINT('Ctrl Pts',(6.37982337814739,-2.76048983145035,14.822555300347));
#63792=CARTESIAN_POINT('Ctrl Pts',(-6.24994586082225,-2.76546765008493,
14.8593861744158));
#63793=CARTESIAN_POINT('Ctrl Pts',(-5.99627373449832,-2.69661205562347,
14.946811432374));
#63794=CARTESIAN_POINT('Ctrl Pts',(-5.7377440125489,-2.63061153982227,15.0295063433286));
#63795=CARTESIAN_POINT('Ctrl Pts',(-5.4744339766703,-2.56798096496872,15.1071490882542));
#63796=CARTESIAN_POINT('Ctrl Pts',(-5.27195631093415,-2.51981989675213,
15.1668540732975));
#63797=CARTESIAN_POINT('Ctrl Pts',(-5.06665225396755,-2.47365226106918,
15.2235711883174));
#63798=CARTESIAN_POINT('Ctrl Pts',(-4.85859706661085,-2.42973038675524,
15.2771463537608));
#63799=CARTESIAN_POINT('Ctrl Pts',(-4.61928783915712,-2.37921057062411,
15.338769577944));
#63800=CARTESIAN_POINT('Ctrl Pts',(-4.37632859149279,-2.33164851275368,
15.396241002441));
#63801=CARTESIAN_POINT('Ctrl Pts',(-4.12983623086809,-2.28736457460126,
15.4493265339033));
#63802=CARTESIAN_POINT('Ctrl Pts',(-4.00659005055573,-2.26522260552506,
15.4758692996345));
#63803=CARTESIAN_POINT('Ctrl Pts',(-3.88246099670014,-2.2438995742547,15.5013154231866));
#63804=CARTESIAN_POINT('Ctrl Pts',(-3.75746623583399,-2.22343165156168,
15.5256346174406));
#63805=CARTESIAN_POINT('Ctrl Pts',(-3.69496885540091,-2.21319769021516,
15.5377942145676));
#63806=CARTESIAN_POINT('Ctrl Pts',(-3.63225504686568,-2.20317750452444,
15.5496720675799));
#63807=CARTESIAN_POINT('Ctrl Pts',(-3.56932715761033,-2.19337530198695,
15.5612643283527));
#63808=CARTESIAN_POINT('Ctrl Pts',(-3.53786321298266,-2.18847420071821,
15.5670604587391));
#63809=CARTESIAN_POINT('Ctrl Pts',(-3.5063457481126,-2.18362759514885,15.5727851903465));
#63810=CARTESIAN_POINT('Ctrl Pts',(-3.4747750621384,-2.17883600094445,15.5784380382115));
#63811=CARTESIAN_POINT('Ctrl Pts',(-3.46643034044414,-2.17756949314224,
15.5799321914349));
#63812=CARTESIAN_POINT('Ctrl Pts',(-3.45808190106549,-2.17630682803461,
15.5814213225294));
#63813=CARTESIAN_POINT('Ctrl Pts',(-3.44972974845269,-2.17504801628272,
15.582905422515));
#63814=CARTESIAN_POINT('Ctrl Pts',(-3.44228250133664,-2.17392558921229,
15.5842287291942));
#63815=CARTESIAN_POINT('Ctrl Pts',(-3.43483230201171,-2.17280622575502,
15.5855480358875));
#63816=CARTESIAN_POINT('Ctrl Pts',(-3.42737915554867,-2.17168993150639,
15.5868633367423));
#63817=CARTESIAN_POINT('Ctrl Pts',(-3.41156724030373,-2.16932170351904,
15.5896537589808));
#63818=CARTESIAN_POINT('Ctrl Pts',(-3.39713125426695,-2.16717258148387,
15.592184569876));
#63819=CARTESIAN_POINT('Ctrl Pts',(-3.37990364855089,-2.16462676050287,
15.5951804590587));
#63820=CARTESIAN_POINT('Ctrl Pts',(-3.08243670618948,-2.12066838372666,
15.6469101079446));
#63821=CARTESIAN_POINT('Ctrl Pts',(-2.78280714443239,-2.08213371852645,
15.6918061299537));
#63822=CARTESIAN_POINT('Ctrl Pts',(-2.48135671024121,-2.04930088083302,
15.7298141593332));
#63823=CARTESIAN_POINT('Ctrl Pts',(-2.18489990185431,-2.01701192991811,
15.7671925731781));
#63824=CARTESIAN_POINT('Ctrl Pts',(-1.88668153319448,-1.99023730879995,
15.7979092668204));
#63825=CARTESIAN_POINT('Ctrl Pts',(-1.58702423552026,-1.96927461093504,
15.821874900134));
#63826=CARTESIAN_POINT('Ctrl Pts',(-1.44871564458144,-1.9595991542501,15.8329363793648));
#63827=CARTESIAN_POINT('Ctrl Pts',(-1.31010052600959,-1.95116231486475,
15.8425591270519));
#63828=CARTESIAN_POINT('Ctrl Pts',(-1.17121088137433,-1.94399593480486,
15.8507316176886));
#63829=CARTESIAN_POINT('Ctrl Pts',(-0.870280897974668,-1.92846865314091,
15.8684388231329));
#63830=CARTESIAN_POINT('Ctrl Pts',(-0.568061182732521,-1.9189035036577,
15.8793402084787));
#63831=CARTESIAN_POINT('Ctrl Pts',(-0.264946396586357,-1.91537688572319,
15.8833583473097));
#63832=CARTESIAN_POINT('Ctrl Pts',(-0.176893607935623,-1.91435242714238,
15.8845255893758));
#63833=CARTESIAN_POINT('Ctrl Pts',(-0.0887653799340636,-1.91383774912774,
15.8851117379332));
#63834=CARTESIAN_POINT('Ctrl Pts',(-0.000571644969191336,-1.9138352439744,
15.8851143000971));
#63835=CARTESIAN_POINT('Ctrl Pts',(0.298411593004284,-1.91382675132062,
15.885122986021));
#63836=CARTESIAN_POINT('Ctrl Pts',(0.596636753996419,-1.91967815635201,
15.8784305185147));
#63837=CARTESIAN_POINT('Ctrl Pts',(0.893741083173373,-1.93132463844706,
15.8651185988725));
#63838=CARTESIAN_POINT('Ctrl Pts',(0.985253235876338,-1.93491191248944,
15.861018347535));
#63839=CARTESIAN_POINT('Ctrl Pts',(1.0766591370822,-1.93904921940413,15.8562898183046));
#63840=CARTESIAN_POINT('Ctrl Pts',(1.16794837273084,-1.94373530482249,15.8509346664032));
#63841=CARTESIAN_POINT('Ctrl Pts',(1.3473991887541,-1.95294692595509,15.840407835153));
#63842=CARTESIAN_POINT('Ctrl Pts',(1.5263991835423,-1.9642787774411,15.8274599788759));
#63843=CARTESIAN_POINT('Ctrl Pts',(1.70488263911043,-1.9776671612215,15.8121140552086));
#63844=CARTESIAN_POINT('Ctrl Pts',(1.98691438642767,-1.99882289949046,15.7878650980584));
#63845=CARTESIAN_POINT('Ctrl Pts',(2.26764243136529,-2.02514654777305,15.7576264894017));
#63846=CARTESIAN_POINT('Ctrl Pts',(2.54678456470886,-2.05638855538998,15.7214699774126));
#63847=CARTESIAN_POINT('Ctrl Pts',(2.68635563138065,-2.07200955919844,15.7033917214181));
#63848=CARTESIAN_POINT('Ctrl Pts',(2.82553043280264,-2.08885858665511,15.6838337769631));
#63849=CARTESIAN_POINT('Ctrl Pts',(2.96427493797265,-2.10689523241144,15.6628038899662));
#63850=CARTESIAN_POINT('Ctrl Pts',(3.03364719055766,-2.1159135552896,15.6522889464677));
#63851=CARTESIAN_POINT('Ctrl Pts',(3.10291186552976,-2.125228779693,15.6414059949692));
#63852=CARTESIAN_POINT('Ctrl Pts',(3.17206480176733,-2.13483519380386,15.6301559451082));
#63853=CARTESIAN_POINT('Ctrl Pts',(3.20664126988611,-2.13963840085929,15.6245309201777));
#63854=CARTESIAN_POINT('Ctrl Pts',(3.24118980305764,-2.14451440514934,15.6188141193533));
#63855=CARTESIAN_POINT('Ctrl Pts',(3.2757098827992,-2.14946247489551,15.6130056505027));
#63856=CARTESIAN_POINT('Ctrl Pts',(3.29296992266997,-2.1519365097686,15.6101014160774));
#63857=CARTESIAN_POINT('Ctrl Pts',(3.31022284916438,-2.15442856099336,15.6071742645679));
#63858=CARTESIAN_POINT('Ctrl Pts',(3.32746859777775,-2.15693853479366,15.6042242092418));
#63859=CARTESIAN_POINT('Ctrl Pts',(3.34471434639113,-2.15944850859396,15.6012741539158));
#63860=CARTESIAN_POINT('Ctrl Pts',(3.36334195791706,-2.1621816194904,15.5980596952111));
#63861=CARTESIAN_POINT('Ctrl Pts',(3.37918424551883,-2.16452212943542,15.5953053448536));
#63862=CARTESIAN_POINT('Ctrl Pts',(3.40180447282053,-2.16786399951689,15.5913725775209));
#63863=CARTESIAN_POINT('Ctrl Pts',(3.42439771599313,-2.17123483076243,15.587402831826));
#63864=CARTESIAN_POINT('Ctrl Pts',(3.44696382211482,-2.17463439951978,15.5833962810123));
#63865=CARTESIAN_POINT('Ctrl Pts',(3.72166647695343,-2.2160181702915,15.5346235712079));
#63866=CARTESIAN_POINT('Ctrl Pts',(3.99234601765621,-2.26165697685362,15.4803988058823));
#63867=CARTESIAN_POINT('Ctrl Pts',(4.25883451373603,-2.31107032049297,15.4210479140662));
#63868=CARTESIAN_POINT('Ctrl Pts',(4.53188464578493,-2.36170034844608,15.3602356497996));
#63869=CARTESIAN_POINT('Ctrl Pts',(4.80053488116735,-2.4162931606847,15.2940417166047));
#63870=CARTESIAN_POINT('Ctrl Pts',(5.06462595783161,-2.47437565815115,15.2227911584299));
#63871=CARTESIAN_POINT('Ctrl Pts',(5.20181840798739,-2.50454888565751,15.1857772661983));
#63872=CARTESIAN_POINT('Ctrl Pts',(5.33778082244635,-2.53566457398629,15.1473983324778));
#63873=CARTESIAN_POINT('Ctrl Pts',(5.47249295507274,-2.56766076945225,15.1076973074869));
#63874=CARTESIAN_POINT('Ctrl Pts',(5.73647117932479,-2.63035964220599,15.0299002607491));
#63875=CARTESIAN_POINT('Ctrl Pts',(5.99564777821735,-2.69643720778191,14.9470280121331));
#63876=CARTESIAN_POINT('Ctrl Pts',(6.24994450567097,-2.76546231685323,14.859387545079));
#63877=CARTESIAN_POINT('Ctrl Pts',(7.0000012587911,8.04447766145535,12.5220647156823));
#63878=CARTESIAN_POINT('Ctrl Pts',(7.00000125879157,10.7706828754762,10.7706844567013));
#63879=CARTESIAN_POINT('Ctrl Pts',(7.00000125879419,12.5220635346855,8.04447949979687));
#63880=CARTESIAN_POINT('Ctrl Pts',(4.44295390839243E-7,9.2830316114314,
14.4500025344128));
#63881=CARTESIAN_POINT('Ctrl Pts',(4.44295937338156E-7,12.4289722487314,
12.4289740734016));
#63882=CARTESIAN_POINT('Ctrl Pts',(4.44298966301522E-7,14.4500011715914,
9.28303373280449));
#63883=CARTESIAN_POINT('Ctrl Pts',(-7.00000045620705,8.04447780346309,12.5220649367283));
#63884=CARTESIAN_POINT('Ctrl Pts',(-7.00000045620657,10.7706830656127,10.7706846468282));
#63885=CARTESIAN_POINT('Ctrl Pts',(-7.00000045620395,12.5220637557412,8.04447964179496));
#63886=CARTESIAN_POINT('Origin',(7.,0.,0.));
#63887=CARTESIAN_POINT('Origin',(-7.,0.,0.));
#63888=CARTESIAN_POINT('Ctrl Pts',(7.00000187330025,14.5427410982365,3.16613343860038));
#63889=CARTESIAN_POINT('Ctrl Pts',(7.00000187328746,15.2320474980471,-1.12398530161775E-6));
#63890=CARTESIAN_POINT('Ctrl Pts',(7.00000187329306,14.5427406309767,-3.16613558484275));
#63891=CARTESIAN_POINT('Ctrl Pts',(-6.61390457865313E-8,16.781789433929,
3.65360177478736));
#63892=CARTESIAN_POINT('Ctrl Pts',(-6.61538026439186E-8,17.5772237182236,
-1.29702851949525E-6));
#63893=CARTESIAN_POINT('Ctrl Pts',(-6.61473378705373E-8,16.7817888947284,
-3.65360425145376));
#63894=CARTESIAN_POINT('Ctrl Pts',(-7.00000199277579,14.5427410600111,3.16613343033478));
#63895=CARTESIAN_POINT('Ctrl Pts',(-7.00000199278858,15.2320474580187,-1.12396941171523E-6));
#63896=CARTESIAN_POINT('Ctrl Pts',(-7.00000199278298,14.5427405927513,-3.16613557654537));
#63897=CARTESIAN_POINT('Origin',(7.,0.,0.));
#63898=CARTESIAN_POINT('Origin',(-7.,0.,0.));
#63899=CARTESIAN_POINT('Ctrl Pts',(7.00000121187377,12.5220644953863,-8.04447803276786));
#63900=CARTESIAN_POINT('Ctrl Pts',(7.00000121181499,10.7706831479978,-10.7706847672647));
#63901=CARTESIAN_POINT('Ctrl Pts',(7.00000121183722,8.04447615020803,-12.5220657048102));
#63902=CARTESIAN_POINT('Ctrl Pts',(2.20648454367741E-7,14.4500023126704,
-9.28303206059653));
#63903=CARTESIAN_POINT('Ctrl Pts',(2.20580622652342E-7,12.4289725910948,
-12.4289744596026));
#63904=CARTESIAN_POINT('Ctrl Pts',(2.20606280418553E-7,9.28302988825824,
-14.4500037082345));
#63905=CARTESIAN_POINT('Ctrl Pts',(-7.00000081329343,12.52206460531,-8.04447810308367));
#63906=CARTESIAN_POINT('Ctrl Pts',(-7.00000081335221,10.7706832424739,-10.7706848616264));
#63907=CARTESIAN_POINT('Ctrl Pts',(-7.00000081332997,8.04447622063808,-12.5220658146196));
#63908=CARTESIAN_POINT('Origin',(7.,0.,0.));
#63909=CARTESIAN_POINT('Origin',(-7.,0.,0.));
#63910=CARTESIAN_POINT('Ctrl Pts',(7.00000130830393,3.16613101538807,-14.5427418150896));
#63911=CARTESIAN_POINT('Ctrl Pts',(7.00000130833239,3.0400473190149E-7,
-15.2320468148857));
#63912=CARTESIAN_POINT('Ctrl Pts',(7.00000130832594,-3.16613043489078,-14.5427419414591));
#63913=CARTESIAN_POINT('Ctrl Pts',(2.16205911596409E-9,3.65359888466782,
-16.7817898306923));
#63914=CARTESIAN_POINT('Ctrl Pts',(2.19489398097225E-9,3.50781807877837E-7,
-17.5772224790036));
#63915=CARTESIAN_POINT('Ctrl Pts',(2.18745987262781E-9,-3.65359821485225,
-16.7817899765181));
#63916=CARTESIAN_POINT('Ctrl Pts',(-7.00000130439666,3.16613101553883,-14.54274181636));
#63917=CARTESIAN_POINT('Ctrl Pts',(-7.0000013043682,3.03956066118533E-7,
-15.2320468161995));
#63918=CARTESIAN_POINT('Ctrl Pts',(-7.00000130437465,-3.16613043513888,
-14.5427419427295));
#63919=CARTESIAN_POINT('Origin',(7.,0.,0.));
#63920=CARTESIAN_POINT('Origin',(-7.,0.,0.));
#63921=CARTESIAN_POINT('Ctrl Pts',(7.00000187325864,-8.04449920362268,-12.52205063737));
#63922=CARTESIAN_POINT('Ctrl Pts',(7.00000187329277,-10.7706925366761,-10.7706713519787));
#63923=CARTESIAN_POINT('Ctrl Pts',(7.00000187328255,-12.5220664599442,-8.04447457416177));
#63924=CARTESIAN_POINT('Ctrl Pts',(3.27183161877263E-7,-9.28305673692403,
-14.4499867034266));
#63925=CARTESIAN_POINT('Ctrl Pts',(3.27222544072347E-7,-12.4289837543079,
-12.4289593079015));
#63926=CARTESIAN_POINT('Ctrl Pts',(3.27210751979541E-7,-14.4500049621397,
-9.283028315387));
#63927=CARTESIAN_POINT('Ctrl Pts',(-7.00000128222652,-8.04449930831836,
-12.5220508000662));
#63928=CARTESIAN_POINT('Ctrl Pts',(-7.00000128219239,-10.7706926767314,
-10.770671491959));
#63929=CARTESIAN_POINT('Ctrl Pts',(-7.00000128220261,-12.5220666227154,
-8.04447467878238));
#63930=CARTESIAN_POINT('Origin',(7.,0.,0.));
#63931=CARTESIAN_POINT('Origin',(-7.,0.,0.));
#63932=CARTESIAN_POINT('Ctrl Pts',(7.00000077642591,-14.5427415801911,-3.16613291281688));
#63933=CARTESIAN_POINT('Ctrl Pts',(7.00000077642943,-15.2320476743123,8.76418954263501E-7));
#63934=CARTESIAN_POINT('Ctrl Pts',(7.00000077642958,-14.5427412158444,3.16613458633202));
#63935=CARTESIAN_POINT('Ctrl Pts',(-5.53471878720152E-8,-16.7817891933195,
-3.65360099454467));
#63936=CARTESIAN_POINT('Ctrl Pts',(-5.53431341970486E-8,-17.5772230870879,
1.01135997016723E-6));
#63937=CARTESIAN_POINT('Ctrl Pts',(-5.53429606034401E-8,-16.7817887728767,
3.65360292572906));
#63938=CARTESIAN_POINT('Ctrl Pts',(-7.0000008764059,-14.5427415482134,-3.16613290583942));
#63939=CARTESIAN_POINT('Ctrl Pts',(-7.00000087640238,-15.2320476408173,
8.76427051435137E-7));
#63940=CARTESIAN_POINT('Ctrl Pts',(-7.00000087640223,-14.5427411838667,
3.16613457937076));
#63941=CARTESIAN_POINT('Origin',(7.,0.,0.));
#63942=CARTESIAN_POINT('Origin',(-7.,0.,0.));
#63943=CARTESIAN_POINT('Ctrl Pts',(7.00000122676011,-12.5220654507218,8.0444765366914));
#63944=CARTESIAN_POINT('Ctrl Pts',(7.00000122674705,-10.770694459262,10.7706678660607));
#63945=CARTESIAN_POINT('Ctrl Pts',(7.00000122675059,-8.04450745410184,12.522045588584));
#63946=CARTESIAN_POINT('Ctrl Pts',(-4.2404238558542E-7,-14.4500036018478,
9.28303045429202));
#63947=CARTESIAN_POINT('Ctrl Pts',(-4.24057452036573E-7,-12.4289858045474,
12.4289551169526));
#63948=CARTESIAN_POINT('Ctrl Pts',(-4.24053364237652E-7,-9.28306613186535,
14.4499806816531));
#63949=CARTESIAN_POINT('Ctrl Pts',(-7.00000199275941,-12.5220652397833,
8.04447640111238));
#63950=CARTESIAN_POINT('Ctrl Pts',(-7.00000199277246,-10.7706942778114,
10.7706676845808));
#63951=CARTESIAN_POINT('Ctrl Pts',(-7.00000199276892,-8.04450731855204,
12.5220453776161));
#63952=CARTESIAN_POINT('Origin',(7.,0.,0.));
#63953=CARTESIAN_POINT('Origin',(-7.,0.,0.));
#63954=CARTESIAN_POINT('Ctrl Pts',(7.00000059287425,-3.16610548810897,14.5427476123492));
#63955=CARTESIAN_POINT('Ctrl Pts',(7.00000059287546,1.45624626939507E-5,
15.2320444588135));
#63956=CARTESIAN_POINT('Ctrl Pts',(7.00000059287604,3.16613329503596,14.5427415584669));
#63957=CARTESIAN_POINT('Ctrl Pts',(-6.39446721752374E-8,-3.65356931914349,
16.7817960242083));
#63958=CARTESIAN_POINT('Ctrl Pts',(-6.39432701116918E-8,1.68045488070068E-5,
17.5772192403596));
#63959=CARTESIAN_POINT('Ctrl Pts',(-6.39426012170821E-8,3.65360140731941,
16.7817890382507));
#63960=CARTESIAN_POINT('Ctrl Pts',(-7.00000070838506,-3.16610548005986,
14.5427475754022));
#63961=CARTESIAN_POINT('Ctrl Pts',(-7.00000070838384,1.45624666247567E-5,
15.232044420115));
#63962=CARTESIAN_POINT('Ctrl Pts',(-7.00000070838326,3.16613328699471,14.5427415215199));
#63963=CARTESIAN_POINT('Origin',(7.,0.,0.));
#63964=CARTESIAN_POINT('Origin',(-7.,0.,0.));
#63965=CARTESIAN_POINT('Origin',(-8.3,0.,0.));
#63966=CARTESIAN_POINT('',(-8.3,-16.1678918187026,-6.69696006698037));
#63967=CARTESIAN_POINT('Origin',(-8.3,-18.0156508836972,-7.46232693177812));
#63968=CARTESIAN_POINT('Origin',(-7.,-18.0156508836972,-7.46232693177812));
#63969=CARTESIAN_POINT('',(-7.,-16.1678918187026,-6.69696006698037));
#63970=CARTESIAN_POINT('Origin',(-7.,-18.0156508836972,-7.46232693177812));
#63971=CARTESIAN_POINT('',(-7.,-16.1678918187026,-6.69696006698036));
#63972=CARTESIAN_POINT('Origin',(-8.3,0.,0.));
#63973=CARTESIAN_POINT('',(-8.3,6.69696006698037,-16.1678918187026));
#63974=CARTESIAN_POINT('Origin',(-8.3,7.46232693177812,-18.0156508836972));
#63975=CARTESIAN_POINT('Origin',(-7.,7.46232693177812,-18.0156508836972));
#63976=CARTESIAN_POINT('',(-7.,6.69696006698037,-16.1678918187026));
#63977=CARTESIAN_POINT('Origin',(-7.,7.46232693177812,-18.0156508836972));
#63978=CARTESIAN_POINT('',(-7.,6.69696006698036,-16.1678918187026));
#63979=CARTESIAN_POINT('Origin',(-8.3,0.,0.));
#63980=CARTESIAN_POINT('',(-8.3,16.1678918187026,6.69696006698037));
#63981=CARTESIAN_POINT('Origin',(-8.3,18.0156508836972,7.46232693177812));
#63982=CARTESIAN_POINT('Origin',(-7.,18.0156508836972,7.46232693177812));
#63983=CARTESIAN_POINT('',(-7.,16.1678918187026,6.69696006698037));
#63984=CARTESIAN_POINT('Origin',(-7.,18.0156508836972,7.46232693177812));
#63985=CARTESIAN_POINT('',(-7.,16.1678918187026,6.69696006698036));
#63986=CARTESIAN_POINT('Origin',(-7.,0.,0.));
#63987=CARTESIAN_POINT('',(-7.,-5.16622633738485,12.4723736887134));
#63988=CARTESIAN_POINT('Origin',(-7.,0.,0.));
#63989=CARTESIAN_POINT('Origin',(-7.7,0.,0.));
#63990=CARTESIAN_POINT('',(7.,-5.16622633738485,12.4723736887134));
#63991=CARTESIAN_POINT('Origin',(7.,0.,0.));
#63992=CARTESIAN_POINT('',(-7.7,-5.16622633738485,12.4723736887134));
#63993=CARTESIAN_POINT('Origin',(8.3,0.,0.));
#63994=CARTESIAN_POINT('',(8.3,-6.69696006579904,-16.1678918191954));
#63995=CARTESIAN_POINT('Origin',(8.3,-7.46232693046164,-18.015650884246));
#63996=CARTESIAN_POINT('Origin',(8.3,-7.46232693046164,-18.015650884246));
#63997=CARTESIAN_POINT('',(7.,-6.69696006579904,-16.1678918191954));
#63998=CARTESIAN_POINT('',(8.3,-6.69696006579904,-16.1678918191954));
#63999=CARTESIAN_POINT('Origin',(7.,-7.46232693046164,-18.015650884246));
#64000=CARTESIAN_POINT('Origin',(8.3,0.,0.));
#64001=CARTESIAN_POINT('',(8.3,16.1678918191954,-6.69696006579904));
#64002=CARTESIAN_POINT('Origin',(8.3,18.015650884246,-7.46232693046164));
#64003=CARTESIAN_POINT('Origin',(8.3,18.015650884246,-7.46232693046164));
#64004=CARTESIAN_POINT('',(7.,16.1678918191954,-6.69696006579904));
#64005=CARTESIAN_POINT('',(8.3,16.1678918191954,-6.69696006579904));
#64006=CARTESIAN_POINT('Origin',(7.,18.015650884246,-7.46232693046164));
#64007=CARTESIAN_POINT('Origin',(8.3,0.,0.));
#64008=CARTESIAN_POINT('',(8.3,6.69696006579904,16.1678918191954));
#64009=CARTESIAN_POINT('Origin',(8.3,7.46232693046164,18.015650884246));
#64010=CARTESIAN_POINT('Origin',(8.3,7.46232693046164,18.015650884246));
#64011=CARTESIAN_POINT('',(7.,6.69696006579904,16.1678918191954));
#64012=CARTESIAN_POINT('',(8.3,6.69696006579904,16.1678918191954));
#64013=CARTESIAN_POINT('Origin',(7.,7.46232693046164,18.015650884246));
#64014=CARTESIAN_POINT('Origin',(7.,0.,0.));
#64015=CARTESIAN_POINT('',(0.,0.,0.));
#64016=CARTESIAN_POINT('Origin',(29.,-23.8,0.));
#64017=CARTESIAN_POINT('',(31.5,-23.8,-3.06161699786838E-16));
#64018=CARTESIAN_POINT('Origin',(29.,-23.8,0.));
#64019=CARTESIAN_POINT('',(29.,-23.8,-1.3856406461));
#64020=CARTESIAN_POINT('',(27.8,-23.8,-0.692820323));
#64021=CARTESIAN_POINT('',(28.3999999999746,-23.8,-1.03923048453533));
#64022=CARTESIAN_POINT('',(27.8,-23.8,0.692820323));
#64023=CARTESIAN_POINT('',(27.8,-23.8,0.17320508075));
#64024=CARTESIAN_POINT('',(29.,-23.8,1.3856406461));
#64025=CARTESIAN_POINT('',(28.3999999999746,-23.8,1.03923048453533));
#64026=CARTESIAN_POINT('',(30.2,-23.8,0.692820323));
#64027=CARTESIAN_POINT('',(29.6000000000254,-23.8,1.03923048453533));
#64028=CARTESIAN_POINT('',(30.2,-23.8,-0.692820323));
#64029=CARTESIAN_POINT('',(30.2,-23.8,0.));
#64030=CARTESIAN_POINT('',(29.6000000000254,-23.8,-1.03923048453533));
#64031=CARTESIAN_POINT('Origin',(29.,-7.8,0.));
#64032=CARTESIAN_POINT('',(31.5,-7.8,-3.06161699786838E-16));
#64033=CARTESIAN_POINT('Origin',(29.,-7.8,0.));
#64034=CARTESIAN_POINT('Origin',(29.,-15.8,0.));
#64035=CARTESIAN_POINT('',(31.5,-15.8,3.06161699786838E-16));
#64036=CARTESIAN_POINT('Origin',(29.,-21.3,3.11198878113149E-17));
#64037=CARTESIAN_POINT('',(30.2,-21.3,-0.692820323));
#64038=CARTESIAN_POINT('',(29.,-21.3,-1.3856406461));
#64039=CARTESIAN_POINT('',(30.2,-21.3,-0.692820323));
#64040=CARTESIAN_POINT('',(30.2,-21.3,0.692820323));
#64041=CARTESIAN_POINT('',(30.2,-21.3,0.692820323));
#64042=CARTESIAN_POINT('',(29.,-21.3,1.3856406461));
#64043=CARTESIAN_POINT('',(29.,-21.3,1.3856406461));
#64044=CARTESIAN_POINT('',(27.8,-21.3,0.692820323));
#64045=CARTESIAN_POINT('',(27.8,-21.3,0.692820323));
#64046=CARTESIAN_POINT('',(27.8,-21.3,-0.692820323));
#64047=CARTESIAN_POINT('',(27.8,-21.3,-0.692820323));
#64048=CARTESIAN_POINT('',(29.,-21.3,-1.3856406461));
#64049=CARTESIAN_POINT('Origin',(29.6,-21.3,-1.03923048455));
#64050=CARTESIAN_POINT('',(30.2,-21.3,-0.692820323));
#64051=CARTESIAN_POINT('',(29.,-21.3,-1.3856406461));
#64052=CARTESIAN_POINT('Origin',(30.2,-21.3,0.));
#64053=CARTESIAN_POINT('',(30.2,-21.3,0.692820323));
#64054=CARTESIAN_POINT('Origin',(29.6,-21.3,1.03923048455));
#64055=CARTESIAN_POINT('',(29.,-21.3,1.3856406461));
#64056=CARTESIAN_POINT('Origin',(28.4,-21.3,1.03923048455));
#64057=CARTESIAN_POINT('',(27.8,-21.3,0.692820323));
#64058=CARTESIAN_POINT('Origin',(27.8,-21.3,0.3464101615));
#64059=CARTESIAN_POINT('',(27.8,-21.3,-0.692820323));
#64060=CARTESIAN_POINT('Origin',(28.4,-21.3,-1.03923048455));
#64061=CARTESIAN_POINT('',(0.,0.,0.));
#64062=CARTESIAN_POINT('Origin',(26.5,12.,20.));
#64063=CARTESIAN_POINT('',(19.,12.,20.));
#64064=CARTESIAN_POINT('Origin',(24.,12.,20.));
#64065=CARTESIAN_POINT('',(21.,12.,20.));
#64066=CARTESIAN_POINT('Origin',(24.,12.,20.));
#64067=CARTESIAN_POINT('Origin',(24.,14.7,20.));
#64068=CARTESIAN_POINT('',(19.,17.4,20.));
#64069=CARTESIAN_POINT('',(19.,14.7,20.));
#64070=CARTESIAN_POINT('Origin',(24.,17.4,20.));
#64071=CARTESIAN_POINT('Origin',(24.,17.3999999999,20.));
#64072=CARTESIAN_POINT('',(19.6,17.9999999999,20.));
#64073=CARTESIAN_POINT('Origin',(19.6000000001,17.3999999999,20.));
#64074=CARTESIAN_POINT('Origin',(24.,17.9999999999,20.));
#64075=CARTESIAN_POINT('Origin',(26.2,17.99999999995,20.));
#64076=CARTESIAN_POINT('',(21.5,18.,21.443375673));
#64077=CARTESIAN_POINT('',(21.5,18.,18.556624327));
#64078=CARTESIAN_POINT('',(21.5,18.,20.));
#64079=CARTESIAN_POINT('',(24.,18.,17.1132486541));
#64080=CARTESIAN_POINT('',(23.5750000000476,18.,17.3586225184655));
#64081=CARTESIAN_POINT('',(26.5,18.,18.556624327));
#64082=CARTESIAN_POINT('',(26.0749999999947,18.,18.3112504626039));
#64083=CARTESIAN_POINT('',(26.5,18.,21.443375673));
#64084=CARTESIAN_POINT('',(26.5,18.,19.63915608175));
#64085=CARTESIAN_POINT('',(24.,18.,22.8867513459));
#64086=CARTESIAN_POINT('',(26.0749999999947,18.,21.6887495373961));
#64087=CARTESIAN_POINT('',(23.5750000000476,18.,22.6413774815345));
#64088=CARTESIAN_POINT('Origin',(24.,15.,20.));
#64089=CARTESIAN_POINT('',(21.5,15.,18.556624327));
#64090=CARTESIAN_POINT('',(21.5,15.,21.443375673));
#64091=CARTESIAN_POINT('',(21.5,15.,21.443375673));
#64092=CARTESIAN_POINT('',(24.,15.,22.8867513459));
#64093=CARTESIAN_POINT('',(24.,15.,22.8867513459));
#64094=CARTESIAN_POINT('',(26.5,15.,21.443375673));
#64095=CARTESIAN_POINT('',(26.5,15.,21.443375673));
#64096=CARTESIAN_POINT('',(26.5,15.,18.556624327));
#64097=CARTESIAN_POINT('',(26.5,15.,20.));
#64098=CARTESIAN_POINT('',(24.,15.,17.1132486541));
#64099=CARTESIAN_POINT('',(24.,15.,17.1132486541));
#64100=CARTESIAN_POINT('',(21.5,15.,18.556624327));
#64101=CARTESIAN_POINT('Origin',(22.75,18.,17.83493649055));
#64102=CARTESIAN_POINT('',(24.,18.,17.1132486541));
#64103=CARTESIAN_POINT('',(21.5,18.,18.556624327));
#64104=CARTESIAN_POINT('Origin',(25.25,18.,17.83493649055));
#64105=CARTESIAN_POINT('',(26.5,18.,18.556624327));
#64106=CARTESIAN_POINT('Origin',(26.5,18.,19.2783121635));
#64107=CARTESIAN_POINT('',(26.5,18.,21.443375673));
#64108=CARTESIAN_POINT('Origin',(25.25,18.,22.16506350945));
#64109=CARTESIAN_POINT('',(24.,18.,22.8867513459));
#64110=CARTESIAN_POINT('Origin',(22.75,18.,22.16506350945));
#64111=CARTESIAN_POINT('',(21.5,18.,21.443375673));
#64112=CARTESIAN_POINT('Origin',(21.5,18.,20.));
#64113=CARTESIAN_POINT('Origin',(25.193275,-8.,20.));
#64114=CARTESIAN_POINT('',(21.61345,-8.,20.));
#64115=CARTESIAN_POINT('Origin',(24.,-8.,20.));
#64116=CARTESIAN_POINT('Origin',(24.,-7.693275,20.));
#64117=CARTESIAN_POINT('',(21.,-7.38655,20.));
#64118=CARTESIAN_POINT('Origin',(24.,-7.38655,20.));
#64119=CARTESIAN_POINT('',(21.306725,-7.693275,20.));
#64120=CARTESIAN_POINT('Origin',(24.,2.306725,20.));
#64121=CARTESIAN_POINT('',(21.,2.306725,20.));
#64122=CARTESIAN_POINT('',(0.,0.,0.));
#64123=CARTESIAN_POINT('Origin',(26.5,-12.,-20.));
#64124=CARTESIAN_POINT('',(19.,-12.,-20.));
#64125=CARTESIAN_POINT('Origin',(24.,-12.,-20.));
#64126=CARTESIAN_POINT('',(21.,-12.,-20.));
#64127=CARTESIAN_POINT('Origin',(24.,-12.,-20.));
#64128=CARTESIAN_POINT('Origin',(24.,-14.7,-20.));
#64129=CARTESIAN_POINT('',(19.,-17.4,-20.));
#64130=CARTESIAN_POINT('',(19.,-14.7,-20.));
#64131=CARTESIAN_POINT('Origin',(24.,-17.4,-20.));
#64132=CARTESIAN_POINT('Origin',(24.,-17.3999999999,-20.));
#64133=CARTESIAN_POINT('',(19.6,-17.9999999999,-20.));
#64134=CARTESIAN_POINT('Origin',(19.6000000001,-17.3999999999,-20.));
#64135=CARTESIAN_POINT('Origin',(24.,-17.9999999999,-20.));
#64136=CARTESIAN_POINT('Origin',(26.2,-17.99999999995,-20.));
#64137=CARTESIAN_POINT('',(21.5,-18.,-21.443375673));
#64138=CARTESIAN_POINT('',(21.5,-18.,-18.556624327));
#64139=CARTESIAN_POINT('',(21.5,-18.,-20.));
#64140=CARTESIAN_POINT('',(24.,-18.,-17.1132486541));
#64141=CARTESIAN_POINT('',(23.5750000000476,-18.,-17.3586225184655));
#64142=CARTESIAN_POINT('',(26.5,-18.,-18.556624327));
#64143=CARTESIAN_POINT('',(26.0749999999947,-18.,-18.3112504626039));
#64144=CARTESIAN_POINT('',(26.5,-18.,-21.443375673));
#64145=CARTESIAN_POINT('',(26.5,-18.,-19.63915608175));
#64146=CARTESIAN_POINT('',(24.,-18.,-22.8867513459));
#64147=CARTESIAN_POINT('',(26.0749999999947,-18.,-21.6887495373961));
#64148=CARTESIAN_POINT('',(23.5750000000476,-18.,-22.6413774815345));
#64149=CARTESIAN_POINT('Origin',(24.,-15.,-20.));
#64150=CARTESIAN_POINT('',(21.5,-15.,-18.556624327));
#64151=CARTESIAN_POINT('',(21.5,-15.,-21.443375673));
#64152=CARTESIAN_POINT('',(21.5,-15.,-21.443375673));
#64153=CARTESIAN_POINT('',(24.,-15.,-22.8867513459));
#64154=CARTESIAN_POINT('',(24.,-15.,-22.8867513459));
#64155=CARTESIAN_POINT('',(26.5,-15.,-21.443375673));
#64156=CARTESIAN_POINT('',(26.5,-15.,-21.443375673));
#64157=CARTESIAN_POINT('',(26.5,-15.,-18.556624327));
#64158=CARTESIAN_POINT('',(26.5,-15.,-20.));
#64159=CARTESIAN_POINT('',(24.,-15.,-17.1132486541));
#64160=CARTESIAN_POINT('',(24.,-15.,-17.1132486541));
#64161=CARTESIAN_POINT('',(21.5,-15.,-18.556624327));
#64162=CARTESIAN_POINT('Origin',(22.75,-18.,-17.83493649055));
#64163=CARTESIAN_POINT('',(24.,-18.,-17.1132486541));
#64164=CARTESIAN_POINT('',(21.5,-18.,-18.556624327));
#64165=CARTESIAN_POINT('Origin',(25.25,-18.,-17.83493649055));
#64166=CARTESIAN_POINT('',(26.5,-18.,-18.556624327));
#64167=CARTESIAN_POINT('Origin',(26.5,-18.,-19.2783121635));
#64168=CARTESIAN_POINT('',(26.5,-18.,-21.443375673));
#64169=CARTESIAN_POINT('Origin',(25.25,-18.,-22.16506350945));
#64170=CARTESIAN_POINT('',(24.,-18.,-22.8867513459));
#64171=CARTESIAN_POINT('Origin',(22.75,-18.,-22.16506350945));
#64172=CARTESIAN_POINT('',(21.5,-18.,-21.443375673));
#64173=CARTESIAN_POINT('Origin',(21.5,-18.,-20.));
#64174=CARTESIAN_POINT('Origin',(25.193275,8.,-20.));
#64175=CARTESIAN_POINT('',(21.61345,8.,-20.));
#64176=CARTESIAN_POINT('Origin',(24.,8.,-20.));
#64177=CARTESIAN_POINT('Origin',(24.,7.693275,-20.));
#64178=CARTESIAN_POINT('',(21.,7.38655,-20.));
#64179=CARTESIAN_POINT('Origin',(24.,7.38655,-20.));
#64180=CARTESIAN_POINT('',(21.306725,7.693275,-20.));
#64181=CARTESIAN_POINT('Origin',(24.,-2.306725,-20.));
#64182=CARTESIAN_POINT('',(21.,-2.306725,-20.));
#64183=CARTESIAN_POINT('',(0.,0.,0.));
#64184=CARTESIAN_POINT('Origin',(39.,-9.19238815542512,9.19238815542512));
#64185=CARTESIAN_POINT('',(39.,0.1,-5.99916660878826));
#64186=CARTESIAN_POINT('',(39.,0.1,-25.9998076915965));
#64187=CARTESIAN_POINT('',(39.,0.1,4.59619407771256));
#64188=CARTESIAN_POINT('',(39.,0.1,25.9998076915965));
#64189=CARTESIAN_POINT('Origin',(39.,0.,0.));
#64190=CARTESIAN_POINT('',(39.,0.1,5.99916660878826));
#64191=CARTESIAN_POINT('',(39.,0.1,4.59619407771256));
#64192=CARTESIAN_POINT('Origin',(39.,0.,0.));
#64193=CARTESIAN_POINT('Origin',(38.25,0.,0.));
#64194=CARTESIAN_POINT('',(37.5,0.1,-27.4998181812171));
#64195=CARTESIAN_POINT('',(37.5,0.1,27.4998181812171));
#64196=CARTESIAN_POINT('Origin',(37.5,0.,0.));
#64197=CARTESIAN_POINT('',(38.25,0.1,26.7498129364068));
#64198=CARTESIAN_POINT('',(38.25,0.1,-26.7498129364068));
#64199=CARTESIAN_POINT('Origin',(-7.,-9.72271824131503,9.72271824131503));
#64200=CARTESIAN_POINT('',(-7.,10.0876161703348,14.3));
#64201=CARTESIAN_POINT('',(-7.,12.8747815515449,24.3));
#64202=CARTESIAN_POINT('Origin',(-7.,0.,22.5));
#64203=CARTESIAN_POINT('',(-7.,24.3,12.8747815515449));
#64204=CARTESIAN_POINT('Origin',(-7.,0.,0.));
#64205=CARTESIAN_POINT('',(-7.,14.3,10.0876161703348));
#64206=CARTESIAN_POINT('Origin',(-7.,22.5,0.));
#64207=CARTESIAN_POINT('Origin',(-7.,0.,0.));
#64208=CARTESIAN_POINT('Origin',(-7.,-9.72271824131503,9.72271824131503));
#64209=CARTESIAN_POINT('',(-7.,14.3,-10.0876161703348));
#64210=CARTESIAN_POINT('',(-7.,24.3,-12.8747815515449));
#64211=CARTESIAN_POINT('Origin',(-7.,22.5,0.));
#64212=CARTESIAN_POINT('',(-7.,12.8747815515449,-24.3));
#64213=CARTESIAN_POINT('Origin',(-7.,0.,0.));
#64214=CARTESIAN_POINT('',(-7.,10.0876161703348,-14.3));
#64215=CARTESIAN_POINT('Origin',(-7.,0.,-22.5));
#64216=CARTESIAN_POINT('Origin',(-7.,0.,0.));
#64217=CARTESIAN_POINT('Origin',(1.,0.,0.));
#64218=CARTESIAN_POINT('',(9.,10.0876161703348,-14.3));
#64219=CARTESIAN_POINT('',(9.,14.3,-10.0876161703348));
#64220=CARTESIAN_POINT('Origin',(9.,0.,0.));
#64221=CARTESIAN_POINT('',(1.,14.3,-10.0876161703348));
#64222=CARTESIAN_POINT('',(1.,10.0876161703348,-14.3));
#64223=CARTESIAN_POINT('Origin',(1.,0.,0.));
#64224=CARTESIAN_POINT('',(9.,10.0876161703348,14.3));
#64225=CARTESIAN_POINT('',(1.,10.0876161703348,14.3));
#64226=CARTESIAN_POINT('',(9.,14.3,10.0876161703348));
#64227=CARTESIAN_POINT('',(1.,14.3,10.0876161703348));
#64228=CARTESIAN_POINT('Origin',(9.,0.,0.));
#64229=CARTESIAN_POINT('Origin',(1.,0.,-22.5));
#64230=CARTESIAN_POINT('',(9.,12.8747815515449,-24.3));
#64231=CARTESIAN_POINT('',(1.,12.8747815515449,-24.3));
#64232=CARTESIAN_POINT('Origin',(9.,0.,-22.5));
#64233=CARTESIAN_POINT('Origin',(1.,22.5,0.));
#64234=CARTESIAN_POINT('',(9.,24.3,12.8747815515449));
#64235=CARTESIAN_POINT('',(1.,24.3,12.8747815515449));
#64236=CARTESIAN_POINT('Origin',(9.,22.5,0.));
#64237=CARTESIAN_POINT('Origin',(1.,22.5,0.));
#64238=CARTESIAN_POINT('',(9.,24.3,-12.8747815515449));
#64239=CARTESIAN_POINT('Origin',(9.,22.5,0.));
#64240=CARTESIAN_POINT('',(1.,24.3,-12.8747815515449));
#64241=CARTESIAN_POINT('Origin',(1.,0.,22.5));
#64242=CARTESIAN_POINT('',(9.,12.8747815515449,24.3));
#64243=CARTESIAN_POINT('Origin',(9.,0.,22.5));
#64244=CARTESIAN_POINT('',(1.,12.8747815515449,24.3));
#64245=CARTESIAN_POINT('Origin',(15.25,0.,0.));
#64246=CARTESIAN_POINT('Origin',(9.,0.,0.));
#64247=CARTESIAN_POINT('',(9.,0.1,27.4998181812171));
#64248=CARTESIAN_POINT('Origin',(9.,0.,0.));
#64249=CARTESIAN_POINT('',(15.25,0.1,27.4998181812171));
#64250=CARTESIAN_POINT('',(9.,0.1,-27.4998181812171));
#64251=CARTESIAN_POINT('',(15.25,0.1,-27.4998181812171));
#64252=CARTESIAN_POINT('Origin',(9.,0.,0.));
#64253=CARTESIAN_POINT('',(26.4377160017529,19.4454364826301,-19.4454364826301));
#64254=CARTESIAN_POINT('',(21.5,18.8745860881769,-20.));
#64255=CARTESIAN_POINT('Ctrl Pts',(26.4377160017535,19.4454364826275,-19.4454364826326));
#64256=CARTESIAN_POINT('Ctrl Pts',(26.4059901055805,19.5848952143129,-19.3059777509472));
#64257=CARTESIAN_POINT('Ctrl Pts',(26.3612673723032,19.7227284607851,-19.1650944052198));
#64258=CARTESIAN_POINT('Ctrl Pts',(26.1640017219762,20.169832853608,-18.6985071174812));
#64259=CARTESIAN_POINT('Ctrl Pts',(25.945163052824,20.4554595320486,-18.383121240662));
#64260=CARTESIAN_POINT('Ctrl Pts',(25.4583216143465,20.8332972173375,-17.9521176633326));
#64261=CARTESIAN_POINT('Ctrl Pts',(25.2031277311749,20.9737985255456,-17.7868382119765));
#64262=CARTESIAN_POINT('Ctrl Pts',(24.6276828245849,21.1637417254346,-17.5604063991252));
#64263=CARTESIAN_POINT('Ctrl Pts',(24.3071450917694,21.2132034355965,-17.5));
#64264=CARTESIAN_POINT('Ctrl Pts',(23.6928549082306,21.2132034355965,-17.5));
#64265=CARTESIAN_POINT('Ctrl Pts',(23.3723171754151,21.1637417254346,-17.5604063991252));
#64266=CARTESIAN_POINT('Ctrl Pts',(22.7968722688252,20.9737985255456,-17.7868382119765));
#64267=CARTESIAN_POINT('Ctrl Pts',(22.5416783856535,20.8332972173375,-17.9521176633326));
#64268=CARTESIAN_POINT('Ctrl Pts',(22.0548369471761,20.4554595320486,-18.383121240662));
#64269=CARTESIAN_POINT('Ctrl Pts',(21.8359982780239,20.169832853608,-18.6985071174812));
#64270=CARTESIAN_POINT('Ctrl Pts',(21.5586819382302,19.5412928441449,-19.3544362091167));
#64271=CARTESIAN_POINT('Ctrl Pts',(21.5,19.1981343317555,-19.6946580411449));
#64272=CARTESIAN_POINT('Ctrl Pts',(21.5,18.8745860881769,-20.));
#64273=CARTESIAN_POINT('Ctrl Pts',(21.5,18.8745860881769,-20.));
#64274=CARTESIAN_POINT('Ctrl Pts',(21.5,18.5112642482312,-20.3428774672885));
#64275=CARTESIAN_POINT('Ctrl Pts',(21.5732810359517,18.1082220917789,-20.7028459652353));
#64276=CARTESIAN_POINT('Ctrl Pts',(21.8751326101794,17.3199088998874,-21.3667099444405));
#64277=CARTESIAN_POINT('Ctrl Pts',(22.1019786827811,16.9344413423488,-21.6711549104462));
#64278=CARTESIAN_POINT('Ctrl Pts',(22.5800189982876,16.4058021284168,-22.0718427713117));
#64279=CARTESIAN_POINT('Ctrl Pts',(22.8176675360957,16.2001944002355,-22.222452745926));
#64280=CARTESIAN_POINT('Ctrl Pts',(23.2304377099712,15.976589433265,-22.3831860081774));
#64281=CARTESIAN_POINT('Ctrl Pts',(23.3774232617092,15.9159206638649,-22.4262333390977));
#64282=CARTESIAN_POINT('Ctrl Pts',(23.6826872283767,15.8333169759962,-22.4846329655715));
#64283=CARTESIAN_POINT('Ctrl Pts',(23.8409645128471,15.8113883008419,-22.5));
#64284=CARTESIAN_POINT('Ctrl Pts',(24.,15.8113883008419,-22.5));
#64285=CARTESIAN_POINT('Ctrl Pts',(24.1590354871529,15.8113883008419,-22.5));
#64286=CARTESIAN_POINT('Ctrl Pts',(24.3173127716233,15.8333169759962,-22.4846329655715));
#64287=CARTESIAN_POINT('Ctrl Pts',(24.6225767382908,15.9159206638649,-22.4262333390977));
#64288=CARTESIAN_POINT('Ctrl Pts',(24.7695622900288,15.976589433265,-22.3831860081774));
#64289=CARTESIAN_POINT('Ctrl Pts',(25.1823324639043,16.2001944002355,-22.222452745926));
#64290=CARTESIAN_POINT('Ctrl Pts',(25.4199810017124,16.4058021284168,-22.0718427713117));
#64291=CARTESIAN_POINT('Ctrl Pts',(25.8980213172189,16.9344413423488,-21.6711549104462));
#64292=CARTESIAN_POINT('Ctrl Pts',(26.1248673898206,17.3199088998874,-21.3667099444405));
#64293=CARTESIAN_POINT('Ctrl Pts',(26.4267189640483,18.1082220917789,-20.7028459652353));
#64294=CARTESIAN_POINT('Ctrl Pts',(26.5,18.5112642482312,-20.3428774672885));
#64295=CARTESIAN_POINT('Ctrl Pts',(26.5,19.0613782547939,-19.8237187585295));
#64296=CARTESIAN_POINT('Ctrl Pts',(26.4810497169031,19.2549528183989,-19.6359201468613));
#64297=CARTESIAN_POINT('Ctrl Pts',(26.4377160017535,19.4454364826275,-19.4454364826326));
#64298=CARTESIAN_POINT('',(26.7834228088254,12.,24.7436860633173));
#64299=CARTESIAN_POINT('',(21.2165771911746,12.,24.7436860633173));
#64300=CARTESIAN_POINT('',(24.,12.,24.7436860633173));
#64301=CARTESIAN_POINT('Ctrl Pts',(21.2165771911746,12.,24.7436860633173));
#64302=CARTESIAN_POINT('Ctrl Pts',(20.9800185926029,12.2862102160665,24.6048820636218));
#64303=CARTESIAN_POINT('Ctrl Pts',(20.764413790233,12.5833300005747,24.4543921279647));
#64304=CARTESIAN_POINT('Ctrl Pts',(19.9481928010976,13.811462707463,23.8038074123085));
#64305=CARTESIAN_POINT('Ctrl Pts',(19.4277281498764,14.8735636803617,23.1658933876871));
#64306=CARTESIAN_POINT('Ctrl Pts',(18.7008421968431,16.9568964437325,21.6874432584144));
#64307=CARTESIAN_POINT('Ctrl Pts',(18.5,17.9789117753936,20.8452740961799));
#64308=CARTESIAN_POINT('Ctrl Pts',(18.5,19.5518661056715,19.3608310001999));
#64309=CARTESIAN_POINT('Ctrl Pts',(18.6175304465914,20.2511953036901,18.6288115221753));
#64310=CARTESIAN_POINT('Ctrl Pts',(19.2063453548323,21.4825503875294,17.1942881563934));
#64311=CARTESIAN_POINT('Ctrl Pts',(19.680056660858,22.0156394470847,16.4936948503358));
#64312=CARTESIAN_POINT('Ctrl Pts',(20.7520277927281,22.707492236193,15.5200247473001));
#64313=CARTESIAN_POINT('Ctrl Pts',(21.3285452412578,22.9573233129958,15.1427702692175));
#64314=CARTESIAN_POINT('Ctrl Pts',(22.6156966073876,23.2860541564014,14.6322199108483));
#64315=CARTESIAN_POINT('Ctrl Pts',(23.3263251783664,23.3666428910959,14.5));
#64316=CARTESIAN_POINT('Ctrl Pts',(24.6736748216336,23.3666428910959,14.5));
#64317=CARTESIAN_POINT('Ctrl Pts',(25.3843033926124,23.2860541564014,14.6322199108483));
#64318=CARTESIAN_POINT('Ctrl Pts',(26.6714547587422,22.9573233129958,15.1427702692175));
#64319=CARTESIAN_POINT('Ctrl Pts',(27.2479722072719,22.707492236193,15.5200247473001));
#64320=CARTESIAN_POINT('Ctrl Pts',(28.319943339142,22.0156394470847,16.4936948503358));
#64321=CARTESIAN_POINT('Ctrl Pts',(28.7936546451677,21.4825503875294,17.1942881563934));
#64322=CARTESIAN_POINT('Ctrl Pts',(29.3824695534086,20.2511953036901,18.6288115221753));
#64323=CARTESIAN_POINT('Ctrl Pts',(29.5,19.5518661056715,19.3608310001999));
#64324=CARTESIAN_POINT('Ctrl Pts',(29.5,17.9789117753936,20.8452740961799));
#64325=CARTESIAN_POINT('Ctrl Pts',(29.2991578031569,16.9568964437325,21.6874432584144));
#64326=CARTESIAN_POINT('Ctrl Pts',(28.5722718501237,14.8735636803618,23.1658933876871));
#64327=CARTESIAN_POINT('Ctrl Pts',(28.0518071989025,13.811462707463,23.8038074123085));
#64328=CARTESIAN_POINT('Ctrl Pts',(27.235586209767,12.5833300005747,24.4543921279647));
#64329=CARTESIAN_POINT('Ctrl Pts',(27.0199814073971,12.2862102160665,24.6048820636218));
#64330=CARTESIAN_POINT('Ctrl Pts',(26.7834228088254,12.,24.7436860633173));
#64331=CARTESIAN_POINT('Origin',(24.,0.,0.));
#64332=CARTESIAN_POINT('',(9.,0.1,5.99916660878826));
#64333=CARTESIAN_POINT('',(24.,0.1,5.99916660878826));
#64334=CARTESIAN_POINT('',(9.,0.1,-5.99916660878826));
#64335=CARTESIAN_POINT('Origin',(9.,0.,0.));
#64336=CARTESIAN_POINT('',(24.,0.1,-5.99916660878826));
#64337=CARTESIAN_POINT('Origin',(9.,0.,-22.5));
#64338=CARTESIAN_POINT('',(9.,0.1,-11.25));
#64339=CARTESIAN_POINT('',(9.,0.1,-11.25));
#64340=CARTESIAN_POINT('Origin',(24.,12.25,-20.));
#64341=CARTESIAN_POINT('',(21.5,0.1,-20.));
#64342=CARTESIAN_POINT('',(21.5,12.25,-20.));
#64343=CARTESIAN_POINT('Origin',(24.,0.1,-20.));
#64344=CARTESIAN_POINT('Origin',(28.4,12.,20.));
#64345=CARTESIAN_POINT('Origin',(24.,12.,20.));
#64346=CARTESIAN_POINT('',(20.7,12.,20.));
#64347=CARTESIAN_POINT('Origin',(24.,12.,20.));
#64348=CARTESIAN_POINT('Origin',(24.,7.5,20.));
#64349=CARTESIAN_POINT('',(20.7,3.,20.));
#64350=CARTESIAN_POINT('Origin',(24.,3.,20.));
#64351=CARTESIAN_POINT('',(20.7,7.5,20.));
#64352=CARTESIAN_POINT('Origin',(26.9,3.,20.));
#64353=CARTESIAN_POINT('',(21.5,3.,20.));
#64354=CARTESIAN_POINT('Origin',(24.,3.,20.));
#64355=CARTESIAN_POINT('Origin',(24.,-12.25,20.));
#64356=CARTESIAN_POINT('',(21.5,0.1,20.));
#64357=CARTESIAN_POINT('Origin',(24.,0.1,20.));
#64358=CARTESIAN_POINT('',(21.5,-12.25,20.));
#64359=CARTESIAN_POINT('Origin',(16.,0.1,0.));
#64360=CARTESIAN_POINT('Origin',(16.,0.1,0.));
#64361=CARTESIAN_POINT('Origin',(24.,19.75,20.));
#64362=CARTESIAN_POINT('Origin',(24.,-19.75,-20.));
#64363=CARTESIAN_POINT('',(26.7834228088254,-12.,-24.7436860633173));
#64364=CARTESIAN_POINT('',(21.2165771911746,-12.,-24.7436860633173));
#64365=CARTESIAN_POINT('Origin',(24.,-12.,-20.));
#64366=CARTESIAN_POINT('Ctrl Pts',(26.7834228088254,-12.,-24.7436860633173));
#64367=CARTESIAN_POINT('Ctrl Pts',(27.019981407397,-12.2862102160664,-24.6048820636218));
#64368=CARTESIAN_POINT('Ctrl Pts',(27.235586209767,-12.5833300005747,-24.4543921279647));
#64369=CARTESIAN_POINT('Ctrl Pts',(28.0518071989025,-13.811462707463,-23.8038074123085));
#64370=CARTESIAN_POINT('Ctrl Pts',(28.5722718501237,-14.8735636803618,-23.1658933876871));
#64371=CARTESIAN_POINT('Ctrl Pts',(29.2991578031569,-16.9568964437325,-21.6874432584144));
#64372=CARTESIAN_POINT('Ctrl Pts',(29.5,-17.9789117753936,-20.8452740961799));
#64373=CARTESIAN_POINT('Ctrl Pts',(29.5,-19.5518661056715,-19.3608310001999));
#64374=CARTESIAN_POINT('Ctrl Pts',(29.3824695534086,-20.2511953036901,-18.6288115221753));
#64375=CARTESIAN_POINT('Ctrl Pts',(28.7936546451677,-21.4825503875294,-17.1942881563934));
#64376=CARTESIAN_POINT('Ctrl Pts',(28.319943339142,-22.0156394470847,-16.4936948503358));
#64377=CARTESIAN_POINT('Ctrl Pts',(27.2479722072719,-22.707492236193,-15.5200247473001));
#64378=CARTESIAN_POINT('Ctrl Pts',(26.6714547587422,-22.9573233129958,-15.1427702692175));
#64379=CARTESIAN_POINT('Ctrl Pts',(25.3843033926124,-23.2860541564014,-14.6322199108483));
#64380=CARTESIAN_POINT('Ctrl Pts',(24.6736748216336,-23.3666428910959,-14.5));
#64381=CARTESIAN_POINT('Ctrl Pts',(23.3263251783664,-23.3666428910959,-14.5));
#64382=CARTESIAN_POINT('Ctrl Pts',(22.6156966073876,-23.2860541564014,-14.6322199108483));
#64383=CARTESIAN_POINT('Ctrl Pts',(21.3285452412578,-22.9573233129958,-15.1427702692175));
#64384=CARTESIAN_POINT('Ctrl Pts',(20.7520277927281,-22.707492236193,-15.5200247473001));
#64385=CARTESIAN_POINT('Ctrl Pts',(19.680056660858,-22.0156394470847,-16.4936948503358));
#64386=CARTESIAN_POINT('Ctrl Pts',(19.2063453548323,-21.4825503875294,-17.1942881563934));
#64387=CARTESIAN_POINT('Ctrl Pts',(18.6175304465914,-20.2511953036901,-18.6288115221753));
#64388=CARTESIAN_POINT('Ctrl Pts',(18.5,-19.5518661056715,-19.3608310001999));
#64389=CARTESIAN_POINT('Ctrl Pts',(18.5,-17.9789117753936,-20.8452740961799));
#64390=CARTESIAN_POINT('Ctrl Pts',(18.7008421968431,-16.9568964437325,-21.6874432584144));
#64391=CARTESIAN_POINT('Ctrl Pts',(19.4277281498764,-14.8735636803617,-23.1658933876871));
#64392=CARTESIAN_POINT('Ctrl Pts',(19.9481928010976,-13.811462707463,-23.8038074123085));
#64393=CARTESIAN_POINT('Ctrl Pts',(20.764413790233,-12.5833300005747,-24.4543921279647));
#64394=CARTESIAN_POINT('Ctrl Pts',(20.980018592603,-12.2862102160665,-24.6048820636218));
#64395=CARTESIAN_POINT('Ctrl Pts',(21.2165771911746,-12.,-24.7436860633173));
#64396=CARTESIAN_POINT('Origin',(16.,-0.1,0.));
#64397=CARTESIAN_POINT('',(39.,-0.1,25.9998076915965));
#64398=CARTESIAN_POINT('',(37.5,-0.1,27.4998181812171));
#64399=CARTESIAN_POINT('',(38.25,-0.1,26.7498129364068));
#64400=CARTESIAN_POINT('',(39.,-0.1,5.99916660878826));
#64401=CARTESIAN_POINT('',(39.,-0.1,4.59619407771256));
#64402=CARTESIAN_POINT('',(9.,-0.1,5.99916660878826));
#64403=CARTESIAN_POINT('',(24.,-0.1,5.99916660878826));
#64404=CARTESIAN_POINT('',(9.,-0.1,27.4998181812171));
#64405=CARTESIAN_POINT('',(9.,-0.1,-11.25));
#64406=CARTESIAN_POINT('',(15.25,-0.1,27.4998181812171));
#64407=CARTESIAN_POINT('',(21.5,-0.1,20.));
#64408=CARTESIAN_POINT('Origin',(24.,-0.1,20.));
#64409=CARTESIAN_POINT('Origin',(24.,-12.25,20.));
#64410=CARTESIAN_POINT('',(24.,-15.8113883008419,22.5));
#64411=CARTESIAN_POINT('',(21.5,-18.8745860881769,20.));
#64412=CARTESIAN_POINT('Ctrl Pts',(21.5,-18.8745860881769,20.));
#64413=CARTESIAN_POINT('Ctrl Pts',(21.5,-19.1981343317555,19.6946580411449));
#64414=CARTESIAN_POINT('Ctrl Pts',(21.5586819382302,-19.5412928441449,19.3544362091167));
#64415=CARTESIAN_POINT('Ctrl Pts',(21.8359982780239,-20.169832853608,18.6985071174812));
#64416=CARTESIAN_POINT('Ctrl Pts',(22.054836947176,-20.4554595320486,18.383121240662));
#64417=CARTESIAN_POINT('Ctrl Pts',(22.5416783856535,-20.8332972173375,17.9521176633326));
#64418=CARTESIAN_POINT('Ctrl Pts',(22.7968722688251,-20.9737985255456,17.7868382119765));
#64419=CARTESIAN_POINT('Ctrl Pts',(23.3723171754151,-21.1637417254346,17.5604063991252));
#64420=CARTESIAN_POINT('Ctrl Pts',(23.6928549082306,-21.2132034355965,17.5));
#64421=CARTESIAN_POINT('Ctrl Pts',(24.3071450917694,-21.2132034355965,17.5));
#64422=CARTESIAN_POINT('Ctrl Pts',(24.627682824585,-21.1637417254346,17.5604063991252));
#64423=CARTESIAN_POINT('Ctrl Pts',(25.2031277311749,-20.9737985255456,17.7868382119765));
#64424=CARTESIAN_POINT('Ctrl Pts',(25.4583216143465,-20.8332972173375,17.9521176633326));
#64425=CARTESIAN_POINT('Ctrl Pts',(25.945163052824,-20.4554595320486,18.383121240662));
#64426=CARTESIAN_POINT('Ctrl Pts',(26.1640017219762,-20.169832853608,18.6985071174812));
#64427=CARTESIAN_POINT('Ctrl Pts',(26.4413180617698,-19.5412928441449,19.3544362091167));
#64428=CARTESIAN_POINT('Ctrl Pts',(26.5,-19.1981343317555,19.6946580411449));
#64429=CARTESIAN_POINT('Ctrl Pts',(26.5,-18.5112642482312,20.3428774672885));
#64430=CARTESIAN_POINT('Ctrl Pts',(26.4267189640483,-18.1082220917789,20.7028459652353));
#64431=CARTESIAN_POINT('Ctrl Pts',(26.1248673898206,-17.3199088998874,21.3667099444405));
#64432=CARTESIAN_POINT('Ctrl Pts',(25.8980213172189,-16.9344413423488,21.6711549104462));
#64433=CARTESIAN_POINT('Ctrl Pts',(25.4199810017124,-16.4058021284168,22.0718427713117));
#64434=CARTESIAN_POINT('Ctrl Pts',(25.1823324639043,-16.2001944002355,22.222452745926));
#64435=CARTESIAN_POINT('Ctrl Pts',(24.7695622900288,-15.976589433265,22.3831860081774));
#64436=CARTESIAN_POINT('Ctrl Pts',(24.6225767382908,-15.9159206638649,22.4262333390977));
#64437=CARTESIAN_POINT('Ctrl Pts',(24.3173127716233,-15.8333169759962,22.4846329655715));
#64438=CARTESIAN_POINT('Ctrl Pts',(24.1590354871529,-15.8113883008419,22.5));
#64439=CARTESIAN_POINT('Ctrl Pts',(24.,-15.8113883008419,22.5));
#64440=CARTESIAN_POINT('Ctrl Pts',(24.,-15.8113883008419,22.5));
#64441=CARTESIAN_POINT('Ctrl Pts',(23.8409645128471,-15.8113883008419,22.5));
#64442=CARTESIAN_POINT('Ctrl Pts',(23.6826872283767,-15.8333169759962,22.4846329655715));
#64443=CARTESIAN_POINT('Ctrl Pts',(23.3774232617092,-15.9159206638649,22.4262333390977));
#64444=CARTESIAN_POINT('Ctrl Pts',(23.2304377099712,-15.976589433265,22.3831860081774));
#64445=CARTESIAN_POINT('Ctrl Pts',(22.8176675360957,-16.2001944002355,22.222452745926));
#64446=CARTESIAN_POINT('Ctrl Pts',(22.5800189982876,-16.4058021284168,22.0718427713117));
#64447=CARTESIAN_POINT('Ctrl Pts',(22.1019786827811,-16.9344413423488,21.6711549104462));
#64448=CARTESIAN_POINT('Ctrl Pts',(21.8751326101794,-17.3199088998874,21.3667099444405));
#64449=CARTESIAN_POINT('Ctrl Pts',(21.5732810359517,-18.1082220917789,20.7028459652353));
#64450=CARTESIAN_POINT('Ctrl Pts',(21.5,-18.5112642482312,20.3428774672885));
#64451=CARTESIAN_POINT('Ctrl Pts',(21.5,-18.8745860881769,20.));
#64452=CARTESIAN_POINT('',(21.5,-12.25,20.));
#64453=CARTESIAN_POINT('Origin',(24.,12.25,-20.));
#64454=CARTESIAN_POINT('',(21.5,-0.1,-20.));
#64455=CARTESIAN_POINT('Origin',(24.,-0.1,-20.));
#64456=CARTESIAN_POINT('',(21.5,-3.,-20.));
#64457=CARTESIAN_POINT('',(21.5,12.25,-20.));
#64458=CARTESIAN_POINT('Origin',(24.,-3.,-20.));
#64459=CARTESIAN_POINT('Origin',(26.9,-3.,-20.));
#64460=CARTESIAN_POINT('',(20.7,-3.,-20.));
#64461=CARTESIAN_POINT('Origin',(24.,-3.,-20.));
#64462=CARTESIAN_POINT('Origin',(24.,-7.5,-20.));
#64463=CARTESIAN_POINT('',(20.7,-12.,-20.));
#64464=CARTESIAN_POINT('',(20.7,-7.5,-20.));
#64465=CARTESIAN_POINT('Origin',(24.,-12.,-20.));
#64466=CARTESIAN_POINT('Origin',(28.4,-12.,-20.));
#64467=CARTESIAN_POINT('',(24.,-12.,-24.7436860633173));
#64468=CARTESIAN_POINT('Origin',(16.,-0.1,0.));
#64469=CARTESIAN_POINT('',(37.5,-0.1,-27.4998181812171));
#64470=CARTESIAN_POINT('',(39.,-0.1,-25.9998076915965));
#64471=CARTESIAN_POINT('',(38.25,-0.1,-26.7498129364068));
#64472=CARTESIAN_POINT('',(9.,-0.1,-27.4998181812171));
#64473=CARTESIAN_POINT('',(15.25,-0.1,-27.4998181812171));
#64474=CARTESIAN_POINT('',(9.,-0.1,-5.99916660878826));
#64475=CARTESIAN_POINT('',(9.,-0.1,-11.25));
#64476=CARTESIAN_POINT('',(39.,-0.1,-5.99916660878826));
#64477=CARTESIAN_POINT('',(24.,-0.1,-5.99916660878826));
#64478=CARTESIAN_POINT('',(39.,-0.1,4.59619407771256));
#64479=CARTESIAN_POINT('Origin',(39.,-9.19238815542512,9.19238815542512));
#64480=CARTESIAN_POINT('',(39.,-5.65685424949238,-2.));
#64481=CARTESIAN_POINT('Origin',(39.,0.,0.));
#64482=CARTESIAN_POINT('',(39.,-7.8,-2.));
#64483=CARTESIAN_POINT('',(39.,-6.54619407771256,-2.));
#64484=CARTESIAN_POINT('',(39.,-7.8,2.));
#64485=CARTESIAN_POINT('',(39.,-7.8,4.59619407771256));
#64486=CARTESIAN_POINT('',(39.,-5.65685424949238,2.));
#64487=CARTESIAN_POINT('',(39.,-6.54619407771256,2.));
#64488=CARTESIAN_POINT('Origin',(39.,0.,0.));
#64489=CARTESIAN_POINT('Origin',(39.,0.,0.));
#64490=CARTESIAN_POINT('Origin',(38.25,0.,0.));
#64491=CARTESIAN_POINT('Origin',(37.5,0.,0.));
#64492=CARTESIAN_POINT('Origin',(9.,0.,-22.5));
#64493=CARTESIAN_POINT('',(9.,-12.8747815515449,-24.3));
#64494=CARTESIAN_POINT('Origin',(9.,0.,0.));
#64495=CARTESIAN_POINT('',(9.,-10.0876161703348,-14.3));
#64496=CARTESIAN_POINT('Origin',(9.,0.,-22.5));
#64497=CARTESIAN_POINT('',(9.,-14.3,-10.0876161703348));
#64498=CARTESIAN_POINT('Origin',(9.,0.,0.));
#64499=CARTESIAN_POINT('',(9.,-24.3,-12.8747815515449));
#64500=CARTESIAN_POINT('Origin',(9.,-22.5,0.));
#64501=CARTESIAN_POINT('',(9.,-24.3,12.8747815515449));
#64502=CARTESIAN_POINT('Origin',(9.,0.,0.));
#64503=CARTESIAN_POINT('',(9.,-14.3,10.0876161703348));
#64504=CARTESIAN_POINT('Origin',(9.,-22.5,0.));
#64505=CARTESIAN_POINT('',(9.,-10.0876161703348,14.3));
#64506=CARTESIAN_POINT('Origin',(9.,0.,0.));
#64507=CARTESIAN_POINT('',(9.,-12.8747815515449,24.3));
#64508=CARTESIAN_POINT('Origin',(9.,0.,22.5));
#64509=CARTESIAN_POINT('Origin',(9.,0.,0.));
#64510=CARTESIAN_POINT('',(9.,-5.65685424949238,2.));
#64511=CARTESIAN_POINT('Origin',(9.,0.,0.));
#64512=CARTESIAN_POINT('',(9.,-7.8,2.));
#64513=CARTESIAN_POINT('',(9.,-1.95,2.));
#64514=CARTESIAN_POINT('',(9.,-7.8,-2.));
#64515=CARTESIAN_POINT('',(9.,-7.8,-11.25));
#64516=CARTESIAN_POINT('',(9.,-5.65685424949238,-2.));
#64517=CARTESIAN_POINT('',(9.,-1.95,-2.));
#64518=CARTESIAN_POINT('Origin',(9.,0.,0.));
#64519=CARTESIAN_POINT('Origin',(24.,0.,0.));
#64520=CARTESIAN_POINT('',(29.6403124237433,-5.65685424949238,2.));
#64521=CARTESIAN_POINT('',(24.,-5.65685424949238,2.));
#64522=CARTESIAN_POINT('',(28.3596875762567,-5.65685424949238,2.));
#64523=CARTESIAN_POINT('Ctrl Pts',(28.3596875762567,-5.65685424949239,1.99999999999999));
#64524=CARTESIAN_POINT('Ctrl Pts',(28.5698259640486,-5.63306819907035,2.06727711020427));
#64525=CARTESIAN_POINT('Ctrl Pts',(28.7900272337845,-5.62049819855856,2.1));
#64526=CARTESIAN_POINT('Ctrl Pts',(29.2099727662155,-5.62049819855856,2.1));
#64527=CARTESIAN_POINT('Ctrl Pts',(29.4301740359514,-5.63306819907034,2.06727711020428));
#64528=CARTESIAN_POINT('Ctrl Pts',(29.6403124237433,-5.65685424949239,2.));
#64529=CARTESIAN_POINT('',(24.,-5.65685424949238,2.));
#64530=CARTESIAN_POINT('Origin',(24.,0.,0.));
#64531=CARTESIAN_POINT('',(28.3596875762567,-5.65685424949238,-2.));
#64532=CARTESIAN_POINT('',(24.,-5.65685424949238,-2.));
#64533=CARTESIAN_POINT('',(29.6403124237433,-5.65685424949238,-2.));
#64534=CARTESIAN_POINT('Ctrl Pts',(29.6403124237433,-5.65685424949239,-2.));
#64535=CARTESIAN_POINT('Ctrl Pts',(29.4301740359514,-5.63306819907035,-2.06727711020427));
#64536=CARTESIAN_POINT('Ctrl Pts',(29.2099727662155,-5.62049819855856,-2.1));
#64537=CARTESIAN_POINT('Ctrl Pts',(29.,-5.62049819855856,-2.1));
#64538=CARTESIAN_POINT('Ctrl Pts',(28.7900272337845,-5.62049819855856,-2.1));
#64539=CARTESIAN_POINT('Ctrl Pts',(28.5698259640486,-5.63306819907035,-2.06727711020427));
#64540=CARTESIAN_POINT('Ctrl Pts',(28.3596875762567,-5.65685424949239,-2.));
#64541=CARTESIAN_POINT('',(24.,-5.65685424949238,-2.));
#64542=CARTESIAN_POINT('Origin',(15.25,0.,0.));
#64543=CARTESIAN_POINT('',(3.7202200813,-19.2325444488655,19.6560228434547));
#64544=CARTESIAN_POINT('',(4.3435534146,-19.2325444488655,19.6560228434547));
#64545=CARTESIAN_POINT('',(4.03188674795,-19.2325444488655,19.6560228434547));
#64546=CARTESIAN_POINT('',(4.3435534146,-18.6475617704547,20.2118391052639));
#64547=CARTESIAN_POINT('Ctrl Pts',(4.3435534146,-19.2325444488655,19.6560228434547));
#64548=CARTESIAN_POINT('Ctrl Pts',(4.39419602744118,-19.2325444488655,19.6560228434547));
#64549=CARTESIAN_POINT('Ctrl Pts',(4.44821405117923,-19.2253141398743,19.6631055485021));
#64550=CARTESIAN_POINT('Ctrl Pts',(4.54758440972013,-19.1958605065015,19.6918603235793));
#64551=CARTESIAN_POINT('Ctrl Pts',(4.59293670765284,-19.1736315324598,19.7135267334984));
#64552=CARTESIAN_POINT('Ctrl Pts',(4.66456223528332,-19.1222183158652,19.7634017741075));
#64553=CARTESIAN_POINT('Ctrl Pts',(4.69560557365306,-19.0896044189134,19.7949355413725));
#64554=CARTESIAN_POINT('Ctrl Pts',(4.7367677324877,-19.0179321794404,19.8638044084183));
#64555=CARTESIAN_POINT('Ctrl Pts',(4.7468867479,-18.9788683526504,19.9011336839378));
#64556=CARTESIAN_POINT('Ctrl Pts',(4.7468867479,-18.9054144267782,19.9709256846039));
#64557=CARTESIAN_POINT('Ctrl Pts',(4.73676246101481,-18.8661272497408,20.0080412374082));
#64558=CARTESIAN_POINT('Ctrl Pts',(4.69559144465381,-18.7936626617373,20.0761230151159));
#64559=CARTESIAN_POINT('Ctrl Pts',(4.66454479714166,-18.7604907000729,20.1070950894545));
#64560=CARTESIAN_POINT('Ctrl Pts',(4.59292152712871,-18.7080352594837,20.1559097961516));
#64561=CARTESIAN_POINT('Ctrl Pts',(4.54757596140155,-18.6852506642774,20.1770124569941));
#64562=CARTESIAN_POINT('Ctrl Pts',(4.44821406584017,-18.6550109864893,20.2049743669883));
#64563=CARTESIAN_POINT('Ctrl Pts',(4.39419749547155,-18.6475617704547,20.2118391052639));
#64564=CARTESIAN_POINT('Ctrl Pts',(4.3435534146,-18.6475617704547,20.2118391052639));
#64565=CARTESIAN_POINT('',(3.7202200813,-18.6475617704547,20.2118391052639));
#64566=CARTESIAN_POINT('',(4.03188674795,-18.6475617704547,20.2118391052639));
#64567=CARTESIAN_POINT('Origin',(3.7202200813,0.,0.));
#64568=CARTESIAN_POINT('Origin',(29.,-13.75,0.));
#64569=CARTESIAN_POINT('',(29.6403124237433,-7.8,2.));
#64570=CARTESIAN_POINT('',(31.1,-7.8,2.57175827820944E-16));
#64571=CARTESIAN_POINT('Origin',(29.,-7.8,0.));
#64572=CARTESIAN_POINT('',(31.1,-27.5,2.57175827820944E-16));
#64573=CARTESIAN_POINT('',(31.1,-13.75,2.57175827820944E-16));
#64574=CARTESIAN_POINT('',(26.9,-27.5,0.));
#64575=CARTESIAN_POINT('Ctrl Pts',(26.9,-27.5,-4.16333634234434E-16));
#64576=CARTESIAN_POINT('Ctrl Pts',(26.9,-27.5,0.263790724669232));
#64577=CARTESIAN_POINT('Ctrl Pts',(26.9527396524836,-27.4958150675353,0.5450944837367));
#64578=CARTESIAN_POINT('Ctrl Pts',(27.167084371912,-27.4806868728543,1.06246092692353));
#64579=CARTESIAN_POINT('Ctrl Pts',(27.3286837627136,-27.4699591842076,1.29853224369707));
#64580=CARTESIAN_POINT('Ctrl Pts',(27.7014679712018,-27.4498004540462,1.67131645218531));
#64581=CARTESIAN_POINT('Ctrl Pts',(27.9375391926626,-27.4390590848186,1.83291567693009));
#64582=CARTESIAN_POINT('Ctrl Pts',(28.4549053217882,-27.423899590768,2.04726026764777));
#64583=CARTESIAN_POINT('Ctrl Pts',(28.7362089711958,-27.4197009465822,2.1));
#64584=CARTESIAN_POINT('Ctrl Pts',(29.2637910288042,-27.4197009465822,2.1));
#64585=CARTESIAN_POINT('Ctrl Pts',(29.5450946782118,-27.423899590768,2.04726026764777));
#64586=CARTESIAN_POINT('Ctrl Pts',(30.0624608073374,-27.4390590848186,1.8329156769301));
#64587=CARTESIAN_POINT('Ctrl Pts',(30.2985320287982,-27.4498004540462,1.67131645218531));
#64588=CARTESIAN_POINT('Ctrl Pts',(30.6713162372864,-27.4699591842076,1.29853224369707));
#64589=CARTESIAN_POINT('Ctrl Pts',(30.832915628088,-27.4806868728543,1.06246092692352));
#64590=CARTESIAN_POINT('Ctrl Pts',(31.0472603475164,-27.4958150675353,0.545094483736699));
#64591=CARTESIAN_POINT('Ctrl Pts',(31.1,-27.5,0.263790724669232));
#64592=CARTESIAN_POINT('Ctrl Pts',(31.1,-27.5,-4.85722573273506E-16));
#64593=CARTESIAN_POINT('',(29.,-27.4197009465822,-2.1));
#64594=CARTESIAN_POINT('Ctrl Pts',(29.,-27.4197009465822,-2.1));
#64595=CARTESIAN_POINT('Ctrl Pts',(28.9409243313237,-27.4197009465822,-2.1));
#64596=CARTESIAN_POINT('Ctrl Pts',(28.8823185718112,-27.41989199691,-2.09751141842624));
#64597=CARTESIAN_POINT('Ctrl Pts',(28.8241875421993,-27.4202649703079,-2.09262753008797));
#64598=CARTESIAN_POINT('Ctrl Pts',(28.7651735223191,-27.4206436090429,-2.08766945717214));
#64599=CARTESIAN_POINT('Ctrl Pts',(28.7066479007282,-27.4212097395195,-2.08024281822867));
#64600=CARTESIAN_POINT('Ctrl Pts',(28.6486082408746,-27.4219538122106,-2.07039219270619));
#64601=CARTESIAN_POINT('Ctrl Pts',(28.5905518712427,-27.4226980991222,-2.06053873116144));
#64602=CARTESIAN_POINT('Ctrl Pts',(28.532980875708,-27.4236204307232,-2.04825974278311));
#64603=CARTESIAN_POINT('Ctrl Pts',(28.4758984634574,-27.424711249236,-2.03354802731425));
#64604=CARTESIAN_POINT('Ctrl Pts',(28.4194214360888,-27.4257904991236,-2.01899233626311));
#64605=CARTESIAN_POINT('Ctrl Pts',(28.3634218905768,-27.4270346811134,-2.00205494714711));
#64606=CARTESIAN_POINT('Ctrl Pts',(28.3079207704063,-27.4284345383079,-1.98268160327497));
#64607=CARTESIAN_POINT('Ctrl Pts',(28.2704559711509,-27.4293794808355,-1.96960405750932));
#64608=CARTESIAN_POINT('Ctrl Pts',(28.2332186617402,-27.4303953587217,-1.95541555925643));
#64609=CARTESIAN_POINT('Ctrl Pts',(28.1962227045941,-27.4314793246848,-1.94008815763357));
#64610=CARTESIAN_POINT('Ctrl Pts',(28.1419909448439,-27.4330682924051,-1.91761997390408));
#64611=CARTESIAN_POINT('Ctrl Pts',(28.0891325285996,-27.434776870226,-1.89306111287472));
#64612=CARTESIAN_POINT('Ctrl Pts',(28.0376128725783,-27.4365837911004,-1.8664969908824));
#64613=CARTESIAN_POINT('Ctrl Pts',(27.9853278197182,-27.4384175563217,-1.83953822155411));
#64614=CARTESIAN_POINT('Ctrl Pts',(27.9344207893789,-27.4403526083505,-1.81051389260381));
#64615=CARTESIAN_POINT('Ctrl Pts',(27.8848692034387,-27.4423667181325,-1.77946152151725));
#64616=CARTESIAN_POINT('Ctrl Pts',(27.8353096468437,-27.4443811518955,-1.74840415547999));
#64617=CARTESIAN_POINT('Ctrl Pts',(27.787105233271,-27.4464746688476,-1.71531763408417));
#64618=CARTESIAN_POINT('Ctrl Pts',(27.7402584733154,-27.448625029206,-1.6801938239222));
#64619=CARTESIAN_POINT('Ctrl Pts',(27.6939156420422,-27.4507522582258,-1.6454478391508));
#64620=CARTESIAN_POINT('Ctrl Pts',(27.6489008015155,-27.452935114305,-1.60870758824503));
#64621=CARTESIAN_POINT('Ctrl Pts',(27.6052508774519,-27.4551520676655,-1.56992830573606));
#64622=CARTESIAN_POINT('Ctrl Pts',(27.5745062828372,-27.4567135671138,-1.54261432190297));
#64623=CARTESIAN_POINT('Ctrl Pts',(27.5444395290512,-27.4582919822752,-1.51428798453775));
#64624=CARTESIAN_POINT('Ctrl Pts',(27.515076404205,-27.4598797900746,-1.48492488518827));
#64625=CARTESIAN_POINT('Ctrl Pts',(27.4739307804,-27.4621047352306,-1.44377929711088));
#64626=CARTESIAN_POINT('Ctrl Pts',(27.4348258111026,-27.464310388427,-1.40126006169301));
#64627=CARTESIAN_POINT('Ctrl Pts',(27.3976932514178,-27.4664763150051,-1.35742885023417));
#64628=CARTESIAN_POINT('Ctrl Pts',(27.3600131664037,-27.4686741785051,-1.31295134079059));
#64629=CARTESIAN_POINT('Ctrl Pts',(27.324363452127,-27.4708311351993,-1.26712232282476));
#64630=CARTESIAN_POINT('Ctrl Pts',(27.2907051879064,-27.472925833098,-1.21996362460113));
#64631=CARTESIAN_POINT('Ctrl Pts',(27.2570404827003,-27.4750209318468,-1.17279590189273));
#64632=CARTESIAN_POINT('Ctrl Pts',(27.2253674916476,-27.4770537479697,-1.12429729314642));
#64633=CARTESIAN_POINT('Ctrl Pts',(27.1956878552808,-27.4790029172168,-1.07445692534351));
#64634=CARTESIAN_POINT('Ctrl Pts',(27.1663254278886,-27.4809312542013,-1.02514923967236));
#64635=CARTESIAN_POINT('Ctrl Pts',(27.1389136304772,-27.4827777227514,-0.974527572618045));
#64636=CARTESIAN_POINT('Ctrl Pts',(27.1134998926964,-27.4845216363304,-0.922560212204816));
#64637=CARTESIAN_POINT('Ctrl Pts',(27.0945077136406,-27.4858248967652,-0.883723996039469));
#64638=CARTESIAN_POINT('Ctrl Pts',(27.0766323337252,-27.4870708816564,-0.84413572170515));
#64639=CARTESIAN_POINT('Ctrl Pts',(27.0599121975429,-27.4882509571134,-0.803778152699582));
#64640=CARTESIAN_POINT('Ctrl Pts',(27.0375591557555,-27.4898285923499,-0.749824380039959));
#64641=CARTESIAN_POINT('Ctrl Pts',(27.0176337763087,-27.4912611977169,-0.695376406081773));
#64642=CARTESIAN_POINT('Ctrl Pts',(27.0000496507938,-27.4925402285157,-0.640467486067715));
#64643=CARTESIAN_POINT('Ctrl Pts',(26.9822027462824,-27.4938383732835,-0.584738001454926));
#64644=CARTESIAN_POINT('Ctrl Pts',(26.9667672171644,-27.4949783191173,-0.52853293039682));
#64645=CARTESIAN_POINT('Ctrl Pts',(26.9536989008167,-27.4959511324866,-0.47185994901157));
#64646=CARTESIAN_POINT('Ctrl Pts',(26.9406270335015,-27.496924210192,-0.415171568250305));
#64647=CARTESIAN_POINT('Ctrl Pts',(26.9299234702452,-27.4977300645931,-0.358014183201836));
#64648=CARTESIAN_POINT('Ctrl Pts',(26.9215940204666,-27.4983597548748,-0.30038073213773));
#64649=CARTESIAN_POINT('Ctrl Pts',(26.9133527431796,-27.4989827794868,-0.243357367588823));
#64650=CARTESIAN_POINT('Ctrl Pts',(26.9074355517769,-27.4994333498565,-0.185867132809557));
#64651=CARTESIAN_POINT('Ctrl Pts',(26.9038985506734,-27.4997028061065,-0.127901188933921));
#64652=CARTESIAN_POINT('Ctrl Pts',(26.9013126263583,-27.4998998073085,-0.0855219135745074));
#64653=CARTESIAN_POINT('Ctrl Pts',(26.9,-27.5,-0.0428882664061002));
#64654=CARTESIAN_POINT('Ctrl Pts',(26.9,-27.5,0.));
#64655=CARTESIAN_POINT('Ctrl Pts',(31.1,-27.5,-3.46944695195361E-16));
#64656=CARTESIAN_POINT('Ctrl Pts',(31.1,-27.5,-0.263790724669233));
#64657=CARTESIAN_POINT('Ctrl Pts',(31.0472603475164,-27.4958150675353,-0.545094483736701));
#64658=CARTESIAN_POINT('Ctrl Pts',(30.832915628088,-27.4806868728543,-1.06246092692353));
#64659=CARTESIAN_POINT('Ctrl Pts',(30.6713162372864,-27.4699591842076,-1.29853224369707));
#64660=CARTESIAN_POINT('Ctrl Pts',(30.2985320287982,-27.4498004540462,-1.67131645218531));
#64661=CARTESIAN_POINT('Ctrl Pts',(30.0624608073374,-27.4390590848186,-1.8329156769301));
#64662=CARTESIAN_POINT('Ctrl Pts',(29.5450946782118,-27.423899590768,-2.04726026764777));
#64663=CARTESIAN_POINT('Ctrl Pts',(29.2637910288042,-27.4197009465822,-2.1));
#64664=CARTESIAN_POINT('Ctrl Pts',(29.,-27.4197009465822,-2.1));
#64665=CARTESIAN_POINT('',(29.6403124237433,-7.8,-2.));
#64666=CARTESIAN_POINT('Origin',(29.,-7.8,0.));
#64667=CARTESIAN_POINT('',(29.6403124237433,-6.72842712474619,-2.));
#64668=CARTESIAN_POINT('',(28.3596875762567,-7.8,-2.));
#64669=CARTESIAN_POINT('',(28.3596875762567,-6.72842712474619,-2.));
#64670=CARTESIAN_POINT('',(28.3596875762567,-7.8,2.));
#64671=CARTESIAN_POINT('Origin',(29.,-7.8,0.));
#64672=CARTESIAN_POINT('',(28.3596875762567,-6.72842712474619,2.));
#64673=CARTESIAN_POINT('',(29.6403124237433,-6.72842712474619,2.));
#64674=CARTESIAN_POINT('Origin',(24.,-3.9,-2.));
#64675=CARTESIAN_POINT('',(24.,-7.8,-2.));
#64676=CARTESIAN_POINT('Origin',(24.,-3.9,-2.));
#64677=CARTESIAN_POINT('',(24.,-7.8,-2.));
#64678=CARTESIAN_POINT('Origin',(24.,-7.8,0.));
#64679=CARTESIAN_POINT('',(24.,-7.8,2.));
#64680=CARTESIAN_POINT('Origin',(24.,-7.8,0.));
#64681=CARTESIAN_POINT('',(24.,-7.8,2.));
#64682=CARTESIAN_POINT('Origin',(24.,-3.9,2.));
#64683=CARTESIAN_POINT('Origin',(24.,-3.9,2.));
#64684=CARTESIAN_POINT('Origin',(1.,0.,22.5));
#64685=CARTESIAN_POINT('',(-7.,-12.8747815515449,24.3));
#64686=CARTESIAN_POINT('',(-7.,-10.0876161703348,14.3));
#64687=CARTESIAN_POINT('Origin',(-7.,0.,22.5));
#64688=CARTESIAN_POINT('',(1.,-12.8747815515449,24.3));
#64689=CARTESIAN_POINT('',(1.,-10.0876161703348,14.3));
#64690=CARTESIAN_POINT('Origin',(1.,-22.5,0.));
#64691=CARTESIAN_POINT('',(-7.,-24.3,-12.8747815515449));
#64692=CARTESIAN_POINT('',(-7.,-14.3,-10.0876161703348));
#64693=CARTESIAN_POINT('Origin',(-7.,-22.5,0.));
#64694=CARTESIAN_POINT('',(1.,-24.3,-12.8747815515449));
#64695=CARTESIAN_POINT('',(1.,-14.3,-10.0876161703348));
#64696=CARTESIAN_POINT('Origin',(1.,0.,-22.5));
#64697=CARTESIAN_POINT('',(-7.,-12.8747815515449,-24.3));
#64698=CARTESIAN_POINT('',(1.,-12.8747815515449,-24.3));
#64699=CARTESIAN_POINT('',(-7.,-10.0876161703348,-14.3));
#64700=CARTESIAN_POINT('Origin',(-7.,0.,-22.5));
#64701=CARTESIAN_POINT('',(1.,-10.0876161703348,-14.3));
#64702=CARTESIAN_POINT('Origin',(1.,0.,0.));
#64703=CARTESIAN_POINT('',(-7.,-14.3,10.0876161703348));
#64704=CARTESIAN_POINT('Origin',(-7.,0.,0.));
#64705=CARTESIAN_POINT('',(1.,-14.3,10.0876161703348));
#64706=CARTESIAN_POINT('Origin',(1.,0.,0.));
#64707=CARTESIAN_POINT('Origin',(-7.,0.,0.));
#64708=CARTESIAN_POINT('Origin',(1.,-22.5,0.));
#64709=CARTESIAN_POINT('',(-7.,-24.3,12.8747815515449));
#64710=CARTESIAN_POINT('',(1.,-24.3,12.8747815515449));
#64711=CARTESIAN_POINT('Origin',(-7.,-22.5,0.));
#64712=CARTESIAN_POINT('Origin',(-7.,-9.72271824131503,9.72271824131503));
#64713=CARTESIAN_POINT('Origin',(-7.,0.,0.));
#64714=CARTESIAN_POINT('Origin',(-7.,-9.72271824131503,9.72271824131503));
#64715=CARTESIAN_POINT('Origin',(-7.,0.,0.));
#64716=CARTESIAN_POINT('Origin',(15.25,0.,0.));
#64717=CARTESIAN_POINT('',(4.3435534146,-17.874107980537,20.8989536556285));
#64718=CARTESIAN_POINT('',(5.18767834635794,-19.7673317665207,19.118122157584));
#64719=CARTESIAN_POINT('Ctrl Pts',(5.18767834635793,-19.7673317665207,19.118122157584));
#64720=CARTESIAN_POINT('Ctrl Pts',(5.24965809277247,-19.7360217070282,19.1504954382083));
#64721=CARTESIAN_POINT('Ctrl Pts',(5.30712124170086,-19.7015935906934,19.1859300894978));
#64722=CARTESIAN_POINT('Ctrl Pts',(5.48660165044913,-19.5761078943939,19.3143019932782));
#64723=CARTESIAN_POINT('Ctrl Pts',(5.59711475871681,-19.4625384572688,19.4291249072538));
#64724=CARTESIAN_POINT('Ctrl Pts',(5.74364605565176,-19.2109564252457,19.6779178545318));
#64725=CARTESIAN_POINT('Ctrl Pts',(5.7796645257,-19.0728726925368,19.8118157765002));
#64726=CARTESIAN_POINT('Ctrl Pts',(5.7796645257,-18.8112850369902,20.060362407785));
#64727=CARTESIAN_POINT('Ctrl Pts',(5.74357914128895,-18.6703688818376,20.1915501172113));
#64728=CARTESIAN_POINT('Ctrl Pts',(5.59693543031386,-18.408739121605,20.4303620690589));
#64729=CARTESIAN_POINT('Ctrl Pts',(5.4863803371174,-18.2880926642702,20.5380618497645));
#64730=CARTESIAN_POINT('Ctrl Pts',(5.2314028462211,-18.0965825390734,20.7070034351683));
#64731=CARTESIAN_POINT('Ctrl Pts',(5.06999631183931,-18.0129189000428,20.779560855588));
#64732=CARTESIAN_POINT('Ctrl Pts',(4.71625542419336,-17.90164394286,20.8755009713159));
#64733=CARTESIAN_POINT('Ctrl Pts',(4.52391635613999,-17.874107980537,20.8989536556285));
#64734=CARTESIAN_POINT('Ctrl Pts',(4.3435534146,-17.874107980537,20.8989536556285));
#64735=CARTESIAN_POINT('',(5.7631397208,-20.8989536556285,17.874107980537));
#64736=CARTESIAN_POINT('Origin',(5.03051074633478,2.27365790259165,-2.27404388388516));
#64737=CARTESIAN_POINT('',(4.7295794663,-20.8989536556285,17.874107980537));
#64738=CARTESIAN_POINT('',(5.24635959355,-20.8989536556285,17.874107980537));
#64739=CARTESIAN_POINT('',(4.2292347159,-19.9191739484904,18.9598657487278));
#64740=CARTESIAN_POINT('Origin',(3.9969811813217,2.27238339981618,-2.27289593102036));
#64741=CARTESIAN_POINT('',(3.7202200813,-19.9191739484904,18.9598657487278));
#64742=CARTESIAN_POINT('',(3.9747273986,-19.9191739484904,18.9598657487278));
#64743=CARTESIAN_POINT('',(3.7202200813,-20.8989536556285,17.874107980537));
#64744=CARTESIAN_POINT('Origin',(3.7202200813,0.,0.));
#64745=CARTESIAN_POINT('',(2.7424423035,-20.8989536556285,17.874107980537));
#64746=CARTESIAN_POINT('',(3.2313311924,-20.8989536556285,17.874107980537));
#64747=CARTESIAN_POINT('',(2.7424423035,-17.874107980537,20.8989536556285));
#64748=CARTESIAN_POINT('Origin',(2.7424423035,0.,0.));
#64749=CARTESIAN_POINT('',(3.54299785905,-17.874107980537,20.8989536556285));
#64750=CARTESIAN_POINT('',(1.4888888889,-18.6070663646292,20.2491254453689));
#64751=CARTESIAN_POINT('',(1.4888888889,-20.8989536556285,17.874107980537));
#64752=CARTESIAN_POINT('Origin',(1.4888888889,0.,0.));
#64753=CARTESIAN_POINT('',(0.5111111111,-20.8989536556285,17.874107980537));
#64754=CARTESIAN_POINT('',(1.,-20.8989536556285,17.874107980537));
#64755=CARTESIAN_POINT('',(0.5111111111,-18.6070663646292,20.2491254453689));
#64756=CARTESIAN_POINT('Origin',(0.5111111111,0.,0.));
#64757=CARTESIAN_POINT('',(-0.5277777778,-18.6070663646292,20.2491254453689));
#64758=CARTESIAN_POINT('',(-0.00833333335000042,-18.6070663646292,20.2491254453689));
#64759=CARTESIAN_POINT('',(-0.5277777778,-17.874107980537,20.8989536556285));
#64760=CARTESIAN_POINT('Origin',(-0.527777777800001,0.,0.));
#64761=CARTESIAN_POINT('',(2.5277777778,-17.874107980537,20.8989536556285));
#64762=CARTESIAN_POINT('',(1.,-17.874107980537,20.8989536556285));
#64763=CARTESIAN_POINT('',(2.5277777778,-18.6070663646292,20.2491254453689));
#64764=CARTESIAN_POINT('Origin',(2.5277777778,0.,0.));
#64765=CARTESIAN_POINT('',(2.00833333335,-18.6070663646292,20.2491254453689));
#64766=CARTESIAN_POINT('',(-3.7631397208,-21.2925086575347,17.4034213610087));
#64767=CARTESIAN_POINT('',(-1.8075841652,-21.2925086575347,17.4034213610087));
#64768=CARTESIAN_POINT('',(-2.785361943,-21.2925086575347,17.4034213610086));
#64769=CARTESIAN_POINT('',(1.,-22.2889734574269,16.1075032892786));
#64770=CARTESIAN_POINT('Origin',(-6.57072387330978,-4.43551506634776E-8,
3.4092084710835E-8));
#64771=CARTESIAN_POINT('',(3.8075841652,-21.2925086575347,17.4034213610087));
#64772=CARTESIAN_POINT('Origin',(8.57072389460998,2.73287437124736E-8,-2.01895722362622E-8));
#64773=CARTESIAN_POINT('',(5.7631397208,-21.2925086575347,17.4034213610087));
#64774=CARTESIAN_POINT('',(4.785361943,-21.2925086575347,17.4034213610086));
#64775=CARTESIAN_POINT('',(1.,-22.9416461797837,15.1634715867317));
#64776=CARTESIAN_POINT('Origin',(10.5262794394392,-7.77399478124607E-9,
6.01586114257202E-9));
#64777=CARTESIAN_POINT('Origin',(-8.52627944622453,1.44232226162444E-8,
-1.06424180579268E-8));
#64778=CARTESIAN_POINT('',(-1.9747474276,-19.3023137418562,19.5875134769819));
#64779=CARTESIAN_POINT('',(-0.5561396937,-20.8989536556285,17.874107980537));
#64780=CARTESIAN_POINT('Origin',(-1.85251751839491,0.,0.));
#64781=CARTESIAN_POINT('',(-1.6994942043,-20.8989536556285,17.874107980537));
#64782=CARTESIAN_POINT('',(-1.127816949,-20.8989536556285,17.874107980537));
#64783=CARTESIAN_POINT('',(-2.785361943,-19.6894777136292,19.1982933450997));
#64784=CARTESIAN_POINT('Origin',(-2.99551159274116,7.11916623071864,-7.12000723870792));
#64785=CARTESIAN_POINT('',(-2.785361943,-20.8989536556285,17.874107980537));
#64786=CARTESIAN_POINT('Origin',(-2.785361943,0.,0.));
#64787=CARTESIAN_POINT('',(-3.7631397208,-20.8989536556285,17.874107980537));
#64788=CARTESIAN_POINT('',(-3.2742508319,-20.8989536556285,17.874107980537));
#64789=CARTESIAN_POINT('',(-3.7631397208,-17.874107980537,20.8989536556285));
#64790=CARTESIAN_POINT('Origin',(-3.7631397208,0.,0.));
#64791=CARTESIAN_POINT('',(-2.785361943,-17.874107980537,20.8989536556285));
#64792=CARTESIAN_POINT('',(-3.2742508319,-17.874107980537,20.8989536556285));
#64793=CARTESIAN_POINT('',(-2.785361943,-18.9090114682761,19.9674556539536));
#64794=CARTESIAN_POINT('Origin',(-2.785361943,0.,0.));
#64795=CARTESIAN_POINT('',(-1.8474876449,-17.874107980537,20.8989536556285));
#64796=CARTESIAN_POINT('Origin',(-3.28939526749656,8.80977299836507,-8.80811422836384));
#64797=CARTESIAN_POINT('',(-0.6680745397,-17.874107980537,20.8989536556285));
#64798=CARTESIAN_POINT('',(-1.2577810923,-17.874107980537,20.8989536556285));
#64799=CARTESIAN_POINT('Origin',(-2.11077331185338,0.,0.));
#64800=CARTESIAN_POINT('',(1.,-16.1075032892786,22.2889734574269));
#64801=CARTESIAN_POINT('',(-1.8075841652,-17.4034213610087,21.2925086575347));
#64802=CARTESIAN_POINT('Origin',(-6.5707239016573,3.78664832823006E-8,-5.07550401707135E-8));
#64803=CARTESIAN_POINT('',(-3.7631397208,-17.4034213610087,21.2925086575347));
#64804=CARTESIAN_POINT('',(-2.785361943,-17.4034213610086,21.2925086575347));
#64805=CARTESIAN_POINT('',(1.,-15.1634715867317,22.9416461797837));
#64806=CARTESIAN_POINT('Origin',(-8.52627943980808,-4.20687484847804E-9,
5.66308777649738E-9));
#64807=CARTESIAN_POINT('',(5.7631397208,-17.4034213610087,21.2925086575347));
#64808=CARTESIAN_POINT('Origin',(10.5262794297275,-2.73344635814965E-8,
3.70220565315549E-8));
#64809=CARTESIAN_POINT('',(3.8075841652,-17.4034213610087,21.2925086575347));
#64810=CARTESIAN_POINT('',(4.785361943,-17.4034213610086,21.2925086575347));
#64811=CARTESIAN_POINT('Origin',(8.57072386182903,-7.01216418264039E-8,
8.97514196296356E-8));
#64812=CARTESIAN_POINT('Origin',(1.,0.,0.));
#64813=CARTESIAN_POINT('',(1.4888888889,-20.5443060118528,17.5194603367613));
#64814=CARTESIAN_POINT('',(1.4888888889,-18.2531915575896,19.8952506383293));
#64815=CARTESIAN_POINT('Origin',(1.4888888889,0.,0.));
#64816=CARTESIAN_POINT('',(2.5277777778,-18.2531915575896,19.8952506383293));
#64817=CARTESIAN_POINT('',(2.00833333335,-18.2531915575896,19.8952506383293));
#64818=CARTESIAN_POINT('',(2.5277777778,-17.5194603367613,20.5443060118528));
#64819=CARTESIAN_POINT('Origin',(2.5277777778,0.,0.));
#64820=CARTESIAN_POINT('',(-0.5277777778,-17.5194603367613,20.5443060118528));
#64821=CARTESIAN_POINT('',(1.,-17.5194603367613,20.5443060118528));
#64822=CARTESIAN_POINT('',(-0.5277777778,-18.2531915575896,19.8952506383293));
#64823=CARTESIAN_POINT('Origin',(-0.527777777800001,0.,0.));
#64824=CARTESIAN_POINT('',(0.5111111111,-18.2531915575896,19.8952506383293));
#64825=CARTESIAN_POINT('',(-0.00833333335000086,-18.2531915575896,19.8952506383293));
#64826=CARTESIAN_POINT('',(0.5111111111,-20.5443060118528,17.5194603367613));
#64827=CARTESIAN_POINT('Origin',(0.5111111111,0.,0.));
#64828=CARTESIAN_POINT('',(1.,-20.5443060118528,17.5194603367613));
#64829=CARTESIAN_POINT('Origin',(0.5111111111,-0.345696648587947,-0.345696648587947));
#64830=CARTESIAN_POINT('',(0.5111111111,-1.51242283754575,-1.51242283754575));
#64831=CARTESIAN_POINT('',(0.5111111111,0.821029540369857,0.821029540369857));
#64832=CARTESIAN_POINT('Origin',(1.,-1.51242283754575,-1.51242283754575));
#64833=CARTESIAN_POINT('',(1.4888888889,-1.51242283754575,-1.51242283754575));
#64834=CARTESIAN_POINT('Origin',(-0.00833333334999997,0.821029540369857,
0.821029540369857));
#64835=CARTESIAN_POINT('',(-0.5277777778,0.821029540369857,0.821029540369857));
#64836=CARTESIAN_POINT('Origin',(-0.5277777778,1.1667261889578,1.1667261889578));
#64837=CARTESIAN_POINT('',(-0.5277777778,1.51242283754575,1.51242283754575));
#64838=CARTESIAN_POINT('Origin',(1.,1.51242283754575,1.51242283754575));
#64839=CARTESIAN_POINT('',(2.5277777778,1.51242283754575,1.51242283754575));
#64840=CARTESIAN_POINT('Origin',(2.5277777778,1.1667261889578,1.1667261889578));
#64841=CARTESIAN_POINT('',(2.5277777778,0.821029540369857,0.821029540369857));
#64842=CARTESIAN_POINT('Origin',(2.00833333335,0.821029540369857,0.821029540369857));
#64843=CARTESIAN_POINT('',(1.4888888889,0.821029540369857,0.821029540369857));
#64844=CARTESIAN_POINT('Origin',(1.4888888889,-0.345696648587947,-0.345696648587947));
#64845=CARTESIAN_POINT('Origin',(-2.24242807365,-0.879007510905235,-0.879007510905235));
#64846=CARTESIAN_POINT('',(-1.6994942043,-20.5443060118528,17.5194603367613));
#64847=CARTESIAN_POINT('',(-1.6994942043,-1.51242283754575,-1.51242283754575));
#64848=CARTESIAN_POINT('',(-2.785361943,-19.3358955993241,18.8447112307947));
#64849=CARTESIAN_POINT('Origin',(-2.99587202900024,0.,0.));
#64850=CARTESIAN_POINT('',(-2.785361943,-0.245592184264721,-0.245592184264721));
#64851=CARTESIAN_POINT('Origin',(-1.127816949,-1.51242283754575,-1.51242283754575));
#64852=CARTESIAN_POINT('',(-0.5561396937,-20.5443060118528,17.5194603367613));
#64853=CARTESIAN_POINT('',(-0.5561396937,-1.51242283754575,-1.51242283754575));
#64854=CARTESIAN_POINT('',(-1.127816949,-20.5443060118528,17.5194603367613));
#64855=CARTESIAN_POINT('Origin',(-1.26544356065,-0.684911484991446,-0.684911484991446));
#64856=CARTESIAN_POINT('',(-1.9747474276,-18.9487506681581,19.2339504032838));
#64857=CARTESIAN_POINT('',(-1.9747474276,0.142599867562857,0.142599867562857));
#64858=CARTESIAN_POINT('Origin',(-1.85251751839491,0.,0.));
#64859=CARTESIAN_POINT('Origin',(-1.2577810923,1.51242283754575,1.51242283754575));
#64860=CARTESIAN_POINT('',(-1.8474876449,-17.5194603367613,20.5443060118528));
#64861=CARTESIAN_POINT('',(-1.8474876449,1.51242283754575,1.51242283754575));
#64862=CARTESIAN_POINT('',(-0.6680745397,-17.5194603367613,20.5443060118528));
#64863=CARTESIAN_POINT('',(-1.2577810923,-17.5194603367613,20.5443060118528));
#64864=CARTESIAN_POINT('',(-0.6680745397,1.51242283754575,1.51242283754575));
#64865=CARTESIAN_POINT('Origin',(-2.31642479395,1.02082246519224,1.02082246519224));
#64866=CARTESIAN_POINT('',(-2.785361943,-18.5553246394379,19.6137688251154));
#64867=CARTESIAN_POINT('',(-2.785361943,0.529222092838726,0.529222092838726));
#64868=CARTESIAN_POINT('Origin',(-3.28936566907665,8.64824730080475,-8.6465264730355));
#64869=CARTESIAN_POINT('Origin',(-2.785361943,1.02082246519224,1.02082246519224));
#64870=CARTESIAN_POINT('',(-2.785361943,-17.5194603367613,20.5443060118528));
#64871=CARTESIAN_POINT('',(-2.785361943,1.51242283754575,1.51242283754575));
#64872=CARTESIAN_POINT('Origin',(-2.785361943,0.,0.));
#64873=CARTESIAN_POINT('Origin',(-3.2742508319,1.51242283754575,1.51242283754575));
#64874=CARTESIAN_POINT('',(-3.7631397208,-17.5194603367613,20.5443060118528));
#64875=CARTESIAN_POINT('',(-3.7631397208,1.51242283754575,1.51242283754575));
#64876=CARTESIAN_POINT('',(-3.2742508319,-17.5194603367613,20.5443060118528));
#64877=CARTESIAN_POINT('Origin',(-3.7631397208,0.,0.));
#64878=CARTESIAN_POINT('',(-3.7631397208,-20.5443060118528,17.5194603367613));
#64879=CARTESIAN_POINT('',(-3.7631397208,-1.51242283754575,-1.51242283754575));
#64880=CARTESIAN_POINT('Origin',(-3.7631397208,0.,0.));
#64881=CARTESIAN_POINT('Origin',(-3.2742508319,-1.51242283754575,-1.51242283754575));
#64882=CARTESIAN_POINT('',(-2.785361943,-20.5443060118528,17.5194603367613));
#64883=CARTESIAN_POINT('',(-2.785361943,-1.51242283754575,-1.51242283754575));
#64884=CARTESIAN_POINT('',(-3.2742508319,-20.5443060118528,17.5194603367613));
#64885=CARTESIAN_POINT('Origin',(-2.785361943,-0.879007510905235,-0.879007510905235));
#64886=CARTESIAN_POINT('Origin',(-2.785361943,0.,0.));
#64887=CARTESIAN_POINT('Origin',(-1.32141098365,0.827511352554304,0.827511352554304));
#64888=CARTESIAN_POINT('Origin',(-2.11077331185338,0.,0.));
#64889=CARTESIAN_POINT('Origin',(1.,0.,0.));
#64890=CARTESIAN_POINT('Origin',(1.,0.,0.));
#64891=CARTESIAN_POINT('',(1.,-22.5806629390448,14.8024883459927));
#64892=CARTESIAN_POINT('',(5.7631397208,-20.9371408903466,17.0480535938206));
#64893=CARTESIAN_POINT('Origin',(10.526279445577,1.21171739309034E-8,-8.89615270338595E-9));
#64894=CARTESIAN_POINT('',(3.8075841652,-20.9371408903466,17.0480535938206));
#64895=CARTESIAN_POINT('',(4.785361943,-20.9371408903466,17.0480535938206));
#64896=CARTESIAN_POINT('',(1.,-21.930781703976,15.7493115358277));
#64897=CARTESIAN_POINT('Origin',(8.57072385391719,-1.12072822133769E-7,
8.59802584685099E-8));
#64898=CARTESIAN_POINT('',(-1.8075841652,-20.9371408903466,17.0480535938206));
#64899=CARTESIAN_POINT('Origin',(-6.57072381790309,-2.36861166236224E-7,
1.81346071492783E-7));
#64900=CARTESIAN_POINT('',(-3.7631397208,-20.9371408903466,17.0480535938206));
#64901=CARTESIAN_POINT('',(-2.785361943,-20.9371408903466,17.0480535938206));
#64902=CARTESIAN_POINT('Origin',(-8.52627944430539,8.13953349165786E-9,
-5.95527405167218E-9));
#64903=CARTESIAN_POINT('Origin',(2.4037920826,-2.51763936616857,-2.51763936616857));
#64904=CARTESIAN_POINT('',(1.,-3.09073508407414,-3.09073508407414));
#64905=CARTESIAN_POINT('',(3.8075841652,-1.94454364826301,-1.94454364826301));
#64906=CARTESIAN_POINT('Origin',(-0.4037920826,-2.51763936616857,-2.51763936616857));
#64907=CARTESIAN_POINT('',(-1.8075841652,-1.94454364826301,-1.94454364826301));
#64908=CARTESIAN_POINT('Origin',(4.785361943,-1.94454364826301,-1.94454364826301));
#64909=CARTESIAN_POINT('',(5.7631397208,-1.94454364826301,-1.94454364826301));
#64910=CARTESIAN_POINT('Origin',(3.3815698604,-2.91681547239451,-2.91681547239451));
#64911=CARTESIAN_POINT('',(1.,-3.88908729652601,-3.88908729652601));
#64912=CARTESIAN_POINT('Origin',(-1.3815698604,-2.91681547239451,-2.91681547239451));
#64913=CARTESIAN_POINT('',(-3.7631397208,-1.94454364826301,-1.94454364826301));
#64914=CARTESIAN_POINT('Origin',(-2.785361943,-1.94454364826301,-1.94454364826301));
#64915=CARTESIAN_POINT('Origin',(4.785361943,1.94454364826301,1.94454364826301));
#64916=CARTESIAN_POINT('',(5.7631397208,-17.0480535938206,20.9371408903466));
#64917=CARTESIAN_POINT('',(5.7631397208,1.94454364826301,1.94454364826301));
#64918=CARTESIAN_POINT('',(3.8075841652,-17.0480535938206,20.9371408903466));
#64919=CARTESIAN_POINT('',(4.785361943,-17.0480535938206,20.9371408903466));
#64920=CARTESIAN_POINT('',(3.8075841652,1.94454364826301,1.94454364826301));
#64921=CARTESIAN_POINT('Origin',(3.3815698604,2.91681547239451,2.91681547239451));
#64922=CARTESIAN_POINT('',(1.,-14.8024883459927,22.5806629390448));
#64923=CARTESIAN_POINT('',(1.,3.88908729652601,3.88908729652601));
#64924=CARTESIAN_POINT('Origin',(10.5262794421488,1.26208155037943E-9,-1.68191238714144E-9));
#64925=CARTESIAN_POINT('Origin',(-1.3815698604,2.91681547239451,2.91681547239451));
#64926=CARTESIAN_POINT('',(-3.7631397208,-17.0480535938206,20.9371408903466));
#64927=CARTESIAN_POINT('',(-3.7631397208,1.94454364826301,1.94454364826301));
#64928=CARTESIAN_POINT('Origin',(-8.52627944021436,-3.35364402914706E-9,
4.51061854533918E-9));
#64929=CARTESIAN_POINT('Origin',(-2.785361943,1.94454364826301,1.94454364826301));
#64930=CARTESIAN_POINT('',(-1.8075841652,-17.0480535938206,20.9371408903466));
#64931=CARTESIAN_POINT('',(-1.8075841652,1.94454364826301,1.94454364826301));
#64932=CARTESIAN_POINT('',(-2.785361943,-17.0480535938206,20.9371408903466));
#64933=CARTESIAN_POINT('Origin',(2.4037920826,2.51763936616857,2.51763936616857));
#64934=CARTESIAN_POINT('',(1.,-15.7493115358277,21.930781703976));
#64935=CARTESIAN_POINT('Origin',(8.57072390411113,4.73520644916903E-8,-6.22505558212083E-8));
#64936=CARTESIAN_POINT('',(1.,3.09073508407414,3.09073508407414));
#64937=CARTESIAN_POINT('Origin',(-0.4037920826,2.51763936616857,2.51763936616857));
#64938=CARTESIAN_POINT('Origin',(-6.57072389687678,3.12376124966818E-8,
-4.02133704113794E-8));
#64939=CARTESIAN_POINT('Origin',(1.,0.,0.));
#64940=CARTESIAN_POINT('Origin',(4.4794070911,-0.996038468713527,-0.996038468713527));
#64941=CARTESIAN_POINT('',(4.7295794663,-20.5443060118528,17.5194603367613));
#64942=CARTESIAN_POINT('',(4.7295794663,-1.51242283754575,-1.51242283754575));
#64943=CARTESIAN_POINT('',(4.2292347159,-19.56551095632,18.6062027565574));
#64944=CARTESIAN_POINT('Origin',(3.99698582654048,2.23070863740945,-2.23124034514977));
#64945=CARTESIAN_POINT('',(4.2292347159,-0.479654099881305,-0.479654099881305));
#64946=CARTESIAN_POINT('Origin',(5.24635959355,-1.51242283754575,-1.51242283754575));
#64947=CARTESIAN_POINT('',(5.7631397208,-20.5443060118528,17.5194603367613));
#64948=CARTESIAN_POINT('',(5.7631397208,-1.51242283754575,-1.51242283754575));
#64949=CARTESIAN_POINT('',(5.24635959355,-20.5443060118528,17.5194603367613));
#64950=CARTESIAN_POINT('Origin',(5.47540903359635,-0.918513821002833,-0.918513821002833));
#64951=CARTESIAN_POINT('',(5.18767834635794,-19.4137281924324,18.7645185834957));
#64952=CARTESIAN_POINT('',(5.18767834635794,-0.324604804468337,-0.324604804468337));
#64953=CARTESIAN_POINT('Origin',(5.03051424672319,2.23200783897291,-2.23240826550412));
#64954=CARTESIAN_POINT('Origin',(4.3435534146,0.496938932349593,0.496938932349593));
#64955=CARTESIAN_POINT('',(4.3435534146,-17.5194603367613,20.5443060118528));
#64956=CARTESIAN_POINT('',(4.3435534146,1.51242283754575,1.51242283754575));
#64957=CARTESIAN_POINT('Ctrl Pts',(4.3435534146,-17.5194603367613,20.5443060118528));
#64958=CARTESIAN_POINT('Ctrl Pts',(4.52391792341369,-17.5194603367613,20.5443060118528));
#64959=CARTESIAN_POINT('Ctrl Pts',(4.71625693450842,-17.5470348446854,20.5208909607321));
#64960=CARTESIAN_POINT('Ctrl Pts',(5.06999455179236,-17.6584515309732,20.4250945452161));
#64961=CARTESIAN_POINT('Ctrl Pts',(5.23139805095757,-17.7422168695679,20.3526419083133));
#64962=CARTESIAN_POINT('Ctrl Pts',(5.48637421277749,-17.9339330499853,20.1839135315558));
#64963=CARTESIAN_POINT('Ctrl Pts',(5.59693050287028,-18.0546991682471,20.0763345995508));
#64964=CARTESIAN_POINT('Ctrl Pts',(5.74357733669248,-18.3165417747782,19.8377335001105));
#64965=CARTESIAN_POINT('Ctrl Pts',(5.7796645257,-18.4575499635599,19.7066343295773));
#64966=CARTESIAN_POINT('Ctrl Pts',(5.7796645257,-18.71926054171,19.4582065445153));
#64967=CARTESIAN_POINT('Ctrl Pts',(5.7436467578758,-18.8573825010707,19.3243479332158));
#64968=CARTESIAN_POINT('Ctrl Pts',(5.59711654864042,-19.1089901329801,19.0755810903176));
#64969=CARTESIAN_POINT('Ctrl Pts',(5.48660381528006,-19.2225482493687,18.9607463124921));
#64970=CARTESIAN_POINT('Ctrl Pts',(5.30712307306233,-19.3480080907561,18.8323468119573));
#64971=CARTESIAN_POINT('Ctrl Pts',(5.24965906631464,-19.3824274887551,18.7969022202364));
#64972=CARTESIAN_POINT('Ctrl Pts',(5.18767834635793,-19.4137281924324,18.7645185834957));
#64973=CARTESIAN_POINT('Origin',(3.54299785905,1.51242283754575,1.51242283754575));
#64974=CARTESIAN_POINT('',(2.7424423035,-17.5194603367613,20.5443060118528));
#64975=CARTESIAN_POINT('',(2.7424423035,1.51242283754575,1.51242283754575));
#64976=CARTESIAN_POINT('',(3.54299785905,-17.5194603367613,20.5443060118528));
#64977=CARTESIAN_POINT('Origin',(3.7202200813,0.496938932349593,0.496938932349593));
#64978=CARTESIAN_POINT('',(3.7202200813,-18.2937167290108,19.85799406382));
#64979=CARTESIAN_POINT('',(3.7202200813,0.782138667404597,0.782138667404597));
#64980=CARTESIAN_POINT('',(3.7202200813,-18.8789697081476,19.3024481027368));
#64981=CARTESIAN_POINT('Origin',(3.7202200813,0.,0.));
#64982=CARTESIAN_POINT('',(3.7202200813,0.211739197294589,0.211739197294589));
#64983=CARTESIAN_POINT('Origin',(4.03188674795,0.782138667404597,0.782138667404597));
#64984=CARTESIAN_POINT('',(4.3435534146,-18.2937167290108,19.85799406382));
#64985=CARTESIAN_POINT('',(4.3435534146,0.782138667404597,0.782138667404597));
#64986=CARTESIAN_POINT('',(4.03188674795,-18.2937167290108,19.85799406382));
#64987=CARTESIAN_POINT('Origin',(2.7424423035,0.,0.));
#64988=CARTESIAN_POINT('',(2.7424423035,-20.5443060118528,17.5194603367613));
#64989=CARTESIAN_POINT('',(2.7424423035,-1.51242283754575,-1.51242283754575));
#64990=CARTESIAN_POINT('Origin',(2.7424423035,0.,0.));
#64991=CARTESIAN_POINT('Origin',(3.2313311924,-1.51242283754575,-1.51242283754575));
#64992=CARTESIAN_POINT('',(3.7202200813,-20.5443060118528,17.5194603367613));
#64993=CARTESIAN_POINT('',(3.7202200813,-1.51242283754575,-1.51242283754575));
#64994=CARTESIAN_POINT('',(3.2313311924,-20.5443060118528,17.5194603367613));
#64995=CARTESIAN_POINT('Origin',(3.7202200813,-0.996038468713527,-0.996038468713527));
#64996=CARTESIAN_POINT('',(3.7202200813,-19.56551095632,18.6062027565574));
#64997=CARTESIAN_POINT('',(3.7202200813,-0.479654099881305,-0.479654099881305));
#64998=CARTESIAN_POINT('Origin',(3.7202200813,0.,0.));
#64999=CARTESIAN_POINT('Origin',(3.9747273986,-0.479654099881305,-0.479654099881305));
#65000=CARTESIAN_POINT('',(3.9747273986,-19.56551095632,18.6062027565574));
#65001=CARTESIAN_POINT('Origin',(4.3435534146,0.496938932349593,0.496938932349593));
#65002=CARTESIAN_POINT('',(4.3435534146,-18.8789697081476,19.3024481027368));
#65003=CARTESIAN_POINT('',(4.3435534146,0.211739197294589,0.211739197294589));
#65004=CARTESIAN_POINT('Ctrl Pts',(4.3435534146,-18.2937167290108,19.85799406382));
#65005=CARTESIAN_POINT('Ctrl Pts',(4.39419751981262,-18.2937167290108,19.85799406382));
#65006=CARTESIAN_POINT('Ctrl Pts',(4.44821399727505,-18.3011713769004,19.8511347365578));
#65007=CARTESIAN_POINT('Ctrl Pts',(4.54757547767286,-18.3314319885872,19.8231941256532));
#65008=CARTESIAN_POINT('Ctrl Pts',(4.59292073016298,-18.3542319727212,19.8021072538948));
#65009=CARTESIAN_POINT('Ctrl Pts',(4.66454409879151,-18.40672084645,19.7533266057787));
#65010=CARTESIAN_POINT('Ctrl Pts',(4.69559097470685,-18.4399132778847,19.7223748562545));
#65011=CARTESIAN_POINT('Ctrl Pts',(4.73676234178596,-18.5124187162062,19.6543334901588));
#65012=CARTESIAN_POINT('Ctrl Pts',(4.7468867479,-18.5517261768333,19.617237912228));
#65013=CARTESIAN_POINT('Ctrl Pts',(4.7468867479,-18.625214121851,19.5474797559526));
#65014=CARTESIAN_POINT('Ctrl Pts',(4.73676781048986,-18.6642939918242,19.5101665751395));
#65015=CARTESIAN_POINT('Ctrl Pts',(4.69560563233662,-18.7359923229461,19.441323557758));
#65016=CARTESIAN_POINT('Ctrl Pts',(4.66456218935101,-18.7686163667244,19.4097996565274));
#65017=CARTESIAN_POINT('Ctrl Pts',(4.59293647859085,-18.8200438549336,19.3599388355082));
#65018=CARTESIAN_POINT('Ctrl Pts',(4.54758424200201,-18.8422779900643,19.3382776827266));
#65019=CARTESIAN_POINT('Ctrl Pts',(4.44821398195441,-18.8717380395622,19.3095294338108));
#65020=CARTESIAN_POINT('Ctrl Pts',(4.39419599674402,-18.8789697081476,19.3024481027368));
#65021=CARTESIAN_POINT('Ctrl Pts',(4.3435534146,-18.8789697081476,19.3024481027368));
#65022=CARTESIAN_POINT('Origin',(4.03188674795,0.211739197294589,0.211739197294589));
#65023=CARTESIAN_POINT('',(4.03188674795,-18.8789697081476,19.3024481027368));
#65024=CARTESIAN_POINT('Origin',(1.,0.,0.));
#65025=CARTESIAN_POINT('',(0.,0.,0.));
#65026=CARTESIAN_POINT('Origin',(-29.,17.1826947828386,17.1826947828386));
#65027=CARTESIAN_POINT('',(-31.5,17.1826947828386,17.1826947828386));
#65028=CARTESIAN_POINT('Origin',(-29.,17.1826947828386,17.1826947828386));
#65029=CARTESIAN_POINT('',(-29.,18.1624906800114,16.2028988857214));
#65030=CARTESIAN_POINT('',(-27.8,17.6725927314035,16.6927968343292));
#65031=CARTESIAN_POINT('',(-28.3999999999746,17.9175417056693,16.4478478600079));
#65032=CARTESIAN_POINT('',(-27.8,16.6927968343292,17.6725927314035));
#65033=CARTESIAN_POINT('',(-27.8,17.0602202957321,17.3051692700007));
#65034=CARTESIAN_POINT('',(-29.,16.2028988857213,18.1624906800114));
#65035=CARTESIAN_POINT('',(-28.3999999999746,16.4478478600079,17.9175417056693));
#65036=CARTESIAN_POINT('',(-30.2,16.6927968343292,17.6725927314035));
#65037=CARTESIAN_POINT('',(-29.6000000000254,16.4478478600079,17.9175417056693));
#65038=CARTESIAN_POINT('',(-30.2,17.6725927314035,16.6927968343292));
#65039=CARTESIAN_POINT('',(-30.2,17.1826947828664,17.1826947828664));
#65040=CARTESIAN_POINT('',(-29.6000000000254,17.9175417056693,16.4478478600079));
#65041=CARTESIAN_POINT('Origin',(-29.,8.6974134086,8.6974134086));
#65042=CARTESIAN_POINT('',(-31.5,8.6974134086,8.6974134086));
#65043=CARTESIAN_POINT('Origin',(-29.,8.6974134086,8.6974134086));
#65044=CARTESIAN_POINT('Origin',(-29.,12.9400540957193,12.9400540957193));
#65045=CARTESIAN_POINT('',(-31.5,12.9400540957193,12.9400540957193));
#65046=CARTESIAN_POINT('Origin',(-29.,15.4149278299,15.4149278299));
#65047=CARTESIAN_POINT('',(-30.2,15.9048257784372,14.9250298813628));
#65048=CARTESIAN_POINT('',(-29.,16.394723727045,14.435131932755));
#65049=CARTESIAN_POINT('',(-30.2,15.9048257784372,14.9250298813628));
#65050=CARTESIAN_POINT('',(-30.2,14.9250298813628,15.9048257784372));
#65051=CARTESIAN_POINT('',(-30.2,14.9250298813628,15.9048257784372));
#65052=CARTESIAN_POINT('',(-29.,14.435131932755,16.394723727045));
#65053=CARTESIAN_POINT('',(-29.,14.435131932755,16.394723727045));
#65054=CARTESIAN_POINT('',(-27.8,14.9250298813628,15.9048257784372));
#65055=CARTESIAN_POINT('',(-27.8,14.9250298813628,15.9048257784372));
#65056=CARTESIAN_POINT('',(-27.8,15.9048257784372,14.9250298813628));
#65057=CARTESIAN_POINT('',(-27.8,15.9048257784372,14.9250298813628));
#65058=CARTESIAN_POINT('',(-29.,16.394723727045,14.435131932755));
#65059=CARTESIAN_POINT('Origin',(-29.6,16.1497747527411,14.6800809070589));
#65060=CARTESIAN_POINT('',(-30.2,15.9048257784372,14.9250298813628));
#65061=CARTESIAN_POINT('',(-29.,16.394723727045,14.435131932755));
#65062=CARTESIAN_POINT('Origin',(-30.2,15.4149278299,15.4149278299));
#65063=CARTESIAN_POINT('',(-30.2,14.9250298813628,15.9048257784372));
#65064=CARTESIAN_POINT('Origin',(-29.6,14.6800809070589,16.1497747527411));
#65065=CARTESIAN_POINT('',(-29.,14.435131932755,16.394723727045));
#65066=CARTESIAN_POINT('Origin',(-28.4,14.6800809070589,16.1497747527411));
#65067=CARTESIAN_POINT('',(-27.8,14.9250298813628,15.9048257784372));
#65068=CARTESIAN_POINT('Origin',(-27.8,15.1699788556314,15.6598768041686));
#65069=CARTESIAN_POINT('',(-27.8,15.9048257784372,14.9250298813628));
#65070=CARTESIAN_POINT('Origin',(-28.4,16.1497747527411,14.6800809070589));
#65071=CARTESIAN_POINT('',(0.,0.,0.));
#65072=CARTESIAN_POINT('Origin',(-26.5,-22.6274169980807,5.65685424941929));
#65073=CARTESIAN_POINT('',(-19.,-22.6274169980807,5.65685424941929));
#65074=CARTESIAN_POINT('Origin',(-24.,-22.6274169980807,5.65685424941929));
#65075=CARTESIAN_POINT('',(-21.,-22.6274169980807,5.65685424941928));
#65076=CARTESIAN_POINT('Origin',(-24.,-22.6274169980807,5.65685424941928));
#65077=CARTESIAN_POINT('Origin',(-24.,-24.5366053072844,3.74766594021561));
#65078=CARTESIAN_POINT('',(-19.,-26.4457936164881,1.83847763101193));
#65079=CARTESIAN_POINT('',(-19.,-24.5366053072844,3.74766594021561));
#65080=CARTESIAN_POINT('Origin',(-24.,-26.4457936164881,1.83847763101193));
#65081=CARTESIAN_POINT('Origin',(-24.,-26.4457936164174,1.83847763108264));
#65082=CARTESIAN_POINT('',(-19.6,-26.8700576851293,1.41421356237071));
#65083=CARTESIAN_POINT('Origin',(-19.6000000001,-26.4457936164174,1.83847763108264));
#65084=CARTESIAN_POINT('Origin',(-24.,-26.8700576851293,1.41421356237071));
#65085=CARTESIAN_POINT('Origin',(-26.2,-26.8700576851646,1.41421356233536));
#65086=CARTESIAN_POINT('',(-21.5,-27.890678411278,2.434834288578));
#65087=CARTESIAN_POINT('',(-21.5,-25.849436958922,0.393592836222004));
#65088=CARTESIAN_POINT('',(-21.5,-26.8700576852402,1.41421356225982));
#65089=CARTESIAN_POINT('',(-24.,-24.8288162328147,-0.627027889885282));
#65090=CARTESIAN_POINT('',(-23.5750000000476,-25.0023217562335,-0.453522366466486));
#65091=CARTESIAN_POINT('',(-26.5,-25.849436958922,0.393592836222004));
#65092=CARTESIAN_POINT('',(-26.0749999999947,-25.6759314354816,0.220087312781607));
#65093=CARTESIAN_POINT('',(-26.5,-27.890678411278,2.434834288578));
#65094=CARTESIAN_POINT('',(-26.5,-26.6149025036153,1.15905838079568));
#65095=CARTESIAN_POINT('',(-24.,-28.9112991373853,3.45545501468528));
#65096=CARTESIAN_POINT('',(-26.0749999999947,-28.0641839347184,2.60833981201839));
#65097=CARTESIAN_POINT('',(-23.5750000000476,-28.7377936139665,3.28194949126649));
#65098=CARTESIAN_POINT('Origin',(-24.,-24.7487373415404,3.53553390595964));
#65099=CARTESIAN_POINT('',(-21.5,-23.7281166153624,2.51491317978165));
#65100=CARTESIAN_POINT('',(-21.5,-25.7693580677184,4.55615463213764));
#65101=CARTESIAN_POINT('',(-21.5,-25.7693580677184,4.55615463213764));
#65102=CARTESIAN_POINT('',(-24.,-26.7899787938256,5.57677535824492));
#65103=CARTESIAN_POINT('',(-24.,-26.7899787938256,5.57677535824492));
#65104=CARTESIAN_POINT('',(-26.5,-25.7693580677184,4.55615463213764));
#65105=CARTESIAN_POINT('',(-26.5,-25.7693580677184,4.55615463213764));
#65106=CARTESIAN_POINT('',(-26.5,-23.7281166153624,2.51491317978165));
#65107=CARTESIAN_POINT('',(-26.5,-24.7487373415404,3.53553390595964));
#65108=CARTESIAN_POINT('',(-24.,-22.7074958892551,1.49429245367436));
#65109=CARTESIAN_POINT('',(-24.,-22.7074958892551,1.49429245367436));
#65110=CARTESIAN_POINT('',(-21.5,-23.7281166153624,2.51491317978165));
#65111=CARTESIAN_POINT('Origin',(-22.75,-25.3391265958684,-0.116717526831639));
#65112=CARTESIAN_POINT('',(-24.,-24.8288162328147,-0.627027889885282));
#65113=CARTESIAN_POINT('',(-21.5,-25.849436958922,0.393592836222004));
#65114=CARTESIAN_POINT('Origin',(-25.25,-25.3391265958684,-0.116717526831639));
#65115=CARTESIAN_POINT('',(-26.5,-25.849436958922,0.393592836222004));
#65116=CARTESIAN_POINT('Origin',(-26.5,-26.359747322011,0.903903199311002));
#65117=CARTESIAN_POINT('',(-26.5,-27.890678411278,2.434834288578));
#65118=CARTESIAN_POINT('Origin',(-25.25,-28.4009887743316,2.94514465163164));
#65119=CARTESIAN_POINT('',(-24.,-28.9112991373853,3.45545501468528));
#65120=CARTESIAN_POINT('Origin',(-22.75,-28.4009887743316,2.94514465163164));
#65121=CARTESIAN_POINT('',(-21.5,-27.890678411278,2.434834288578));
#65122=CARTESIAN_POINT('Origin',(-21.5,-26.8700576851,1.4142135624));
#65123=CARTESIAN_POINT('Origin',(-25.193275,-8.48528137426905,19.798989873231));
#65124=CARTESIAN_POINT('',(-21.61345,-8.48528137426905,19.7989898732309));
#65125=CARTESIAN_POINT('Origin',(-24.,-8.48528137426905,19.798989873231));
#65126=CARTESIAN_POINT('Origin',(-24.,-8.70216870172849,19.5821025457715));
#65127=CARTESIAN_POINT('',(-21.,-8.91905602918794,19.3652152183121));
#65128=CARTESIAN_POINT('Origin',(-24.,-8.91905602918794,19.3652152183121));
#65129=CARTESIAN_POINT('',(-21.306725,-8.70216870172849,19.5821025457715));
#65130=CARTESIAN_POINT('Origin',(-24.,-15.773236513594,12.511034733906));
#65131=CARTESIAN_POINT('',(-21.,-15.773236513594,12.511034733906));
#65132=CARTESIAN_POINT('',(0.,0.,0.));
#65133=CARTESIAN_POINT('Origin',(-26.5,22.6274169980807,-5.65685424941929));
#65134=CARTESIAN_POINT('',(-19.,22.6274169980807,-5.65685424941929));
#65135=CARTESIAN_POINT('Origin',(-24.,22.6274169980807,-5.65685424941929));
#65136=CARTESIAN_POINT('',(-21.,22.6274169980807,-5.65685424941928));
#65137=CARTESIAN_POINT('Origin',(-24.,22.6274169980807,-5.65685424941928));
#65138=CARTESIAN_POINT('Origin',(-24.,24.5366053072844,-3.74766594021561));
#65139=CARTESIAN_POINT('',(-19.,26.4457936164881,-1.83847763101193));
#65140=CARTESIAN_POINT('',(-19.,24.5366053072844,-3.74766594021561));
#65141=CARTESIAN_POINT('Origin',(-24.,26.4457936164881,-1.83847763101193));
#65142=CARTESIAN_POINT('Origin',(-24.,26.4457936164174,-1.83847763108264));
#65143=CARTESIAN_POINT('',(-19.6,26.8700576851293,-1.41421356237071));
#65144=CARTESIAN_POINT('Origin',(-19.6000000001,26.4457936164174,-1.83847763108264));
#65145=CARTESIAN_POINT('Origin',(-24.,26.8700576851293,-1.41421356237071));
#65146=CARTESIAN_POINT('Origin',(-26.2,26.8700576851646,-1.41421356233536));
#65147=CARTESIAN_POINT('',(-21.5,27.890678411278,-2.434834288578));
#65148=CARTESIAN_POINT('',(-21.5,25.849436958922,-0.393592836222004));
#65149=CARTESIAN_POINT('',(-21.5,26.8700576852402,-1.41421356225982));
#65150=CARTESIAN_POINT('',(-24.,24.8288162328147,0.627027889885282));
#65151=CARTESIAN_POINT('',(-23.5750000000476,25.0023217562335,0.453522366466486));
#65152=CARTESIAN_POINT('',(-26.5,25.849436958922,-0.393592836222004));
#65153=CARTESIAN_POINT('',(-26.0749999999947,25.6759314354816,-0.220087312781607));
#65154=CARTESIAN_POINT('',(-26.5,27.890678411278,-2.434834288578));
#65155=CARTESIAN_POINT('',(-26.5,26.6149025036153,-1.15905838079568));
#65156=CARTESIAN_POINT('',(-24.,28.9112991373853,-3.45545501468528));
#65157=CARTESIAN_POINT('',(-26.0749999999947,28.0641839347184,-2.60833981201839));
#65158=CARTESIAN_POINT('',(-23.5750000000476,28.7377936139665,-3.28194949126649));
#65159=CARTESIAN_POINT('Origin',(-24.,24.7487373415404,-3.53553390595964));
#65160=CARTESIAN_POINT('',(-21.5,23.7281166153624,-2.51491317978165));
#65161=CARTESIAN_POINT('',(-21.5,25.7693580677184,-4.55615463213764));
#65162=CARTESIAN_POINT('',(-21.5,25.7693580677184,-4.55615463213764));
#65163=CARTESIAN_POINT('',(-24.,26.7899787938256,-5.57677535824492));
#65164=CARTESIAN_POINT('',(-24.,26.7899787938256,-5.57677535824492));
#65165=CARTESIAN_POINT('',(-26.5,25.7693580677184,-4.55615463213764));
#65166=CARTESIAN_POINT('',(-26.5,25.7693580677184,-4.55615463213764));
#65167=CARTESIAN_POINT('',(-26.5,23.7281166153624,-2.51491317978165));
#65168=CARTESIAN_POINT('',(-26.5,24.7487373415404,-3.53553390595964));
#65169=CARTESIAN_POINT('',(-24.,22.7074958892551,-1.49429245367436));
#65170=CARTESIAN_POINT('',(-24.,22.7074958892551,-1.49429245367436));
#65171=CARTESIAN_POINT('',(-21.5,23.7281166153624,-2.51491317978165));
#65172=CARTESIAN_POINT('Origin',(-22.75,25.3391265958684,0.116717526831639));
#65173=CARTESIAN_POINT('',(-24.,24.8288162328147,0.627027889885282));
#65174=CARTESIAN_POINT('',(-21.5,25.849436958922,-0.393592836222004));
#65175=CARTESIAN_POINT('Origin',(-25.25,25.3391265958684,0.116717526831639));
#65176=CARTESIAN_POINT('',(-26.5,25.849436958922,-0.393592836222004));
#65177=CARTESIAN_POINT('Origin',(-26.5,26.359747322011,-0.903903199311002));
#65178=CARTESIAN_POINT('',(-26.5,27.890678411278,-2.434834288578));
#65179=CARTESIAN_POINT('Origin',(-25.25,28.4009887743316,-2.94514465163164));
#65180=CARTESIAN_POINT('',(-24.,28.9112991373853,-3.45545501468528));
#65181=CARTESIAN_POINT('Origin',(-22.75,28.4009887743316,-2.94514465163164));
#65182=CARTESIAN_POINT('',(-21.5,27.890678411278,-2.434834288578));
#65183=CARTESIAN_POINT('Origin',(-21.5,26.8700576851,-1.4142135624));
#65184=CARTESIAN_POINT('Origin',(-25.193275,8.48528137426905,-19.798989873231));
#65185=CARTESIAN_POINT('',(-21.61345,8.48528137426905,-19.7989898732309));
#65186=CARTESIAN_POINT('Origin',(-24.,8.48528137426905,-19.798989873231));
#65187=CARTESIAN_POINT('Origin',(-24.,8.70216870172849,-19.5821025457715));
#65188=CARTESIAN_POINT('',(-21.,8.91905602918794,-19.3652152183121));
#65189=CARTESIAN_POINT('Origin',(-24.,8.91905602918794,-19.3652152183121));
#65190=CARTESIAN_POINT('',(-21.306725,8.70216870172849,-19.5821025457715));
#65191=CARTESIAN_POINT('Origin',(-24.,15.773236513594,-12.511034733906));
#65192=CARTESIAN_POINT('',(-21.,15.773236513594,-12.511034733906));
#65193=CARTESIAN_POINT('',(0.,0.,0.));
#65194=CARTESIAN_POINT('Origin',(-39.,0.,13.));
#65195=CARTESIAN_POINT('',(-39.,6.64643157139886,-6.78785292759886));
#65196=CARTESIAN_POINT('',(-39.,18.3139296501741,-18.4553510063741));
#65197=CARTESIAN_POINT('',(-39.,-3.32071067811503,3.17928932191503));
#65198=CARTESIAN_POINT('',(-39.,-18.4553510063741,18.3139296501741));
#65199=CARTESIAN_POINT('Origin',(-39.,0.,0.));
#65200=CARTESIAN_POINT('',(-39.,-6.78785292759886,6.64643157139886));
#65201=CARTESIAN_POINT('',(-39.,-3.32071067811503,3.17928932191503));
#65202=CARTESIAN_POINT('Origin',(-39.,0.,0.));
#65203=CARTESIAN_POINT('Origin',(-38.25,0.,0.));
#65204=CARTESIAN_POINT('',(-37.5,19.3745972392358,-19.5160185954358));
#65205=CARTESIAN_POINT('',(-37.5,-19.5160185954358,19.3745972392358));
#65206=CARTESIAN_POINT('Origin',(-37.5,0.,0.));
#65207=CARTESIAN_POINT('',(-38.25,-18.985684800905,18.844263444705));
#65208=CARTESIAN_POINT('',(-38.25,18.844263444705,-18.985684800905));
#65209=CARTESIAN_POINT('Origin',(7.,0.,13.75));
#65210=CARTESIAN_POINT('',(7.,-17.244648771018,2.97860517091918));
#65211=CARTESIAN_POINT('',(7.,-26.2865401242261,8.07884944143965));
#65212=CARTESIAN_POINT('Origin',(7.,-15.9099025767,15.9099025767));
#65213=CARTESIAN_POINT('',(7.,-26.2865401242261,-8.07884944143965));
#65214=CARTESIAN_POINT('Origin',(7.,0.,0.));
#65215=CARTESIAN_POINT('',(7.,-17.244648771018,-2.97860517091918));
#65216=CARTESIAN_POINT('Origin',(7.,-15.9099025767,-15.9099025767));
#65217=CARTESIAN_POINT('Origin',(7.,0.,0.));
#65218=CARTESIAN_POINT('Origin',(7.,0.,13.75));
#65219=CARTESIAN_POINT('',(7.,-2.97860517091918,-17.244648771018));
#65220=CARTESIAN_POINT('',(7.,-8.07884944143965,-26.2865401242261));
#65221=CARTESIAN_POINT('Origin',(7.,-15.9099025767,-15.9099025767));
#65222=CARTESIAN_POINT('',(7.,8.07884944143965,-26.2865401242261));
#65223=CARTESIAN_POINT('Origin',(7.,0.,0.));
#65224=CARTESIAN_POINT('',(7.,2.97860517091918,-17.244648771018));
#65225=CARTESIAN_POINT('Origin',(7.,15.9099025767,-15.9099025767));
#65226=CARTESIAN_POINT('Origin',(7.,0.,0.));
#65227=CARTESIAN_POINT('Origin',(-1.,0.,0.));
#65228=CARTESIAN_POINT('',(-9.,2.97860517091918,-17.244648771018));
#65229=CARTESIAN_POINT('',(-9.,-2.97860517091918,-17.244648771018));
#65230=CARTESIAN_POINT('Origin',(-9.,0.,0.));
#65231=CARTESIAN_POINT('',(-1.,-2.97860517091918,-17.244648771018));
#65232=CARTESIAN_POINT('',(-1.,2.97860517091918,-17.244648771018));
#65233=CARTESIAN_POINT('Origin',(-1.,0.,0.));
#65234=CARTESIAN_POINT('',(-9.,-17.244648771018,2.97860517091918));
#65235=CARTESIAN_POINT('',(-1.,-17.244648771018,2.97860517091918));
#65236=CARTESIAN_POINT('',(-9.,-17.244648771018,-2.97860517091918));
#65237=CARTESIAN_POINT('',(-1.,-17.244648771018,-2.97860517091918));
#65238=CARTESIAN_POINT('Origin',(-9.,0.,0.));
#65239=CARTESIAN_POINT('Origin',(-1.,15.9099025767,-15.9099025767));
#65240=CARTESIAN_POINT('',(-9.,8.07884944143965,-26.2865401242261));
#65241=CARTESIAN_POINT('',(-1.,8.07884944143965,-26.2865401242261));
#65242=CARTESIAN_POINT('Origin',(-9.,15.9099025767,-15.9099025767));
#65243=CARTESIAN_POINT('Origin',(-1.,-15.9099025767,-15.9099025767));
#65244=CARTESIAN_POINT('',(-9.,-26.2865401242261,-8.07884944143965));
#65245=CARTESIAN_POINT('',(-1.,-26.2865401242261,-8.07884944143965));
#65246=CARTESIAN_POINT('Origin',(-9.,-15.9099025767,-15.9099025767));
#65247=CARTESIAN_POINT('Origin',(-1.,-15.9099025767,-15.9099025767));
#65248=CARTESIAN_POINT('',(-9.,-8.07884944143965,-26.2865401242261));
#65249=CARTESIAN_POINT('Origin',(-9.,-15.9099025767,-15.9099025767));
#65250=CARTESIAN_POINT('',(-1.,-8.07884944143965,-26.2865401242261));
#65251=CARTESIAN_POINT('Origin',(-1.,-15.9099025767,15.9099025767));
#65252=CARTESIAN_POINT('',(-9.,-26.2865401242261,8.07884944143965));
#65253=CARTESIAN_POINT('Origin',(-9.,-15.9099025767,15.9099025767));
#65254=CARTESIAN_POINT('',(-1.,-26.2865401242261,8.07884944143965));
#65255=CARTESIAN_POINT('Origin',(-15.25,0.,0.));
#65256=CARTESIAN_POINT('Origin',(-9.,0.,0.));
#65257=CARTESIAN_POINT('',(-9.,-19.5160185954358,19.3745972392358));
#65258=CARTESIAN_POINT('Origin',(-9.,0.,0.));
#65259=CARTESIAN_POINT('',(-15.25,-19.5160185954358,19.3745972392358));
#65260=CARTESIAN_POINT('',(-9.,19.3745972392358,-19.5160185954358));
#65261=CARTESIAN_POINT('',(-15.25,19.3745972392358,-19.5160185954358));
#65262=CARTESIAN_POINT('Origin',(-9.,0.,0.));
#65263=CARTESIAN_POINT('',(-26.4377160017629,5.20014826788293E-15,-27.5));
#65264=CARTESIAN_POINT('',(-21.5,0.795787808628117,-27.4884834387719));
#65265=CARTESIAN_POINT('Ctrl Pts',(-26.4377160017635,3.62918028962156E-12,
-27.5));
#65266=CARTESIAN_POINT('Ctrl Pts',(-26.4059901055898,-0.197224429757389,
-27.5));
#65267=CARTESIAN_POINT('Ctrl Pts',(-26.3612673723093,-0.394306822151656,
-27.4978432541329));
#65268=CARTESIAN_POINT('Ctrl Pts',(-26.1640017219763,-1.04038440540881,
-27.4840667670191));
#65269=CARTESIAN_POINT('Ctrl Pts',(-25.9451630528242,-1.46536445881011,
-27.4630238360419));
#65270=CARTESIAN_POINT('Ctrl Pts',(-25.4583216143471,-2.03730160051001,
-27.4254298732512));
#65271=CARTESIAN_POINT('Ctrl Pts',(-25.2031277311753,-2.25352124915401,
-27.4079090802056));
#65272=CARTESIAN_POINT('Ctrl Pts',(-24.6276828245851,-2.54794284417893,
-27.3821077345433));
#65273=CARTESIAN_POINT('Ctrl Pts',(-24.3071450917694,-2.62563132929186,
-27.3743686707592));
#65274=CARTESIAN_POINT('Ctrl Pts',(-23.6928549082306,-2.62563132929186,
-27.3743686707592));
#65275=CARTESIAN_POINT('Ctrl Pts',(-23.3723171754149,-2.54794284417893,
-27.3821077345433));
#65276=CARTESIAN_POINT('Ctrl Pts',(-22.7968722688247,-2.25352124915401,
-27.4079090802056));
#65277=CARTESIAN_POINT('Ctrl Pts',(-22.5416783856529,-2.03730160051001,
-27.4254298732512));
#65278=CARTESIAN_POINT('Ctrl Pts',(-22.0548369471758,-1.46536445881011,
-27.4630238360419));
#65279=CARTESIAN_POINT('Ctrl Pts',(-21.8359982780237,-1.04038440540881,
-27.4840667670191));
#65280=CARTESIAN_POINT('Ctrl Pts',(-21.5586819382303,-0.132127593799674,
-27.5034337727556));
#65281=CARTESIAN_POINT('Ctrl Pts',(-21.5,0.351095281866489,-27.501357226159));
#65282=CARTESIAN_POINT('Ctrl Pts',(-21.5,0.795787808628117,-27.4884834387719));
#65283=CARTESIAN_POINT('Ctrl Pts',(-21.5,0.795787808628117,-27.4884834387719));
#65284=CARTESIAN_POINT('Ctrl Pts',(-21.5,1.29514612764106,-27.4740270842301));
#65285=CARTESIAN_POINT('Ctrl Pts',(-21.5732810359516,1.83467613548264,-27.4435694082118));
#65286=CARTESIAN_POINT('Ctrl Pts',(-21.875132610179,2.86152046064611,-27.3555705260108));
#65287=CARTESIAN_POINT('Ctrl Pts',(-22.1019786827804,3.34936228446823,-27.2982789021101));
#65288=CARTESIAN_POINT('Ctrl Pts',(-22.5800189982867,4.00649576099619,-27.2078036326968));
#65289=CARTESIAN_POINT('Ctrl Pts',(-22.8176675360951,4.25837971422122,-27.1689143482003));
#65290=CARTESIAN_POINT('Ctrl Pts',(-23.230437709971,4.53014788237278,-27.1244573394495));
#65291=CARTESIAN_POINT('Ctrl Pts',(-23.3774232617091,4.60348624022732,-27.1119971008064));
#65292=CARTESIAN_POINT('Ctrl Pts',(-23.6826872283767,4.70319063996839,-27.0948822448621));
#65293=CARTESIAN_POINT('Ctrl Pts',(-23.8409645128472,4.72956268912345,-27.0902424642094));
#65294=CARTESIAN_POINT('Ctrl Pts',(-24.,4.72956268912345,-27.0902424642094));
#65295=CARTESIAN_POINT('Ctrl Pts',(-24.1590354871528,4.72956268912345,-27.0902424642094));
#65296=CARTESIAN_POINT('Ctrl Pts',(-24.3173127716233,4.70319063996839,-27.0948822448621));
#65297=CARTESIAN_POINT('Ctrl Pts',(-24.6225767382909,4.60348624022732,-27.1119971008064));
#65298=CARTESIAN_POINT('Ctrl Pts',(-24.769562290029,4.53014788237278,-27.1244573394495));
#65299=CARTESIAN_POINT('Ctrl Pts',(-25.1823324639049,4.25837971422122,-27.1689143482003));
#65300=CARTESIAN_POINT('Ctrl Pts',(-25.4199810017133,4.00649576099619,-27.2078036326968));
#65301=CARTESIAN_POINT('Ctrl Pts',(-25.8980213172196,3.34936228446823,-27.2982789021101));
#65302=CARTESIAN_POINT('Ctrl Pts',(-26.124867389821,2.86152046064611,-27.3555705260108));
#65303=CARTESIAN_POINT('Ctrl Pts',(-26.4267189640484,1.83467613548264,-27.4435694082118));
#65304=CARTESIAN_POINT('Ctrl Pts',(-26.5,1.29514612764106,-27.4740270842301));
#65305=CARTESIAN_POINT('Ctrl Pts',(-26.5,0.539056139721172,-27.4959157852184));
#65306=CARTESIAN_POINT('Ctrl Pts',(-26.4810497169061,0.269384581345093,
-27.5));
#65307=CARTESIAN_POINT('Ctrl Pts',(-26.4377160017635,3.62852109470069E-12,
-27.5));
#65308=CARTESIAN_POINT('',(-26.7834228083186,-25.9817095809707,9.0111468332335));
#65309=CARTESIAN_POINT('',(-21.2165771916814,-25.9817095809707,9.01114683323349));
#65310=CARTESIAN_POINT('',(-24.,-25.9817095809707,9.01114683323349));
#65311=CARTESIAN_POINT('Ctrl Pts',(-21.2165771916814,-25.9817095809707,
9.01114683323346));
#65312=CARTESIAN_POINT('Ctrl Pts',(-20.9800185929094,-26.0859415162294,
8.71061639897562));
#65313=CARTESIAN_POINT('Ctrl Pts',(-20.7644137903678,-26.1896244767548,
8.39410853029323));
#65314=CARTESIAN_POINT('Ctrl Pts',(-19.9481928010943,-26.5980125778779,
7.06565470065933));
#65315=CARTESIAN_POINT('Ctrl Pts',(-19.4277281498739,-26.8979580454901,
5.86356256779912));
#65316=CARTESIAN_POINT('Ctrl Pts',(-18.7008421968423,-27.3256746578734,
3.34500173130744));
#65317=CARTESIAN_POINT('Ctrl Pts',(-18.5,-27.4528451038414,2.02682423429658));
#65318=CARTESIAN_POINT('Ctrl Pts',(-18.5,-27.5154319978194,-0.135082218585487));
#65319=CARTESIAN_POINT('Ctrl Pts',(-18.6175304465915,-27.4923164791461,
-1.14719857365593));
#65320=CARTESIAN_POINT('Ctrl Pts',(-19.2063453548323,-27.3486548092588,
-3.0322593031978));
#65321=CARTESIAN_POINT('Ctrl Pts',(-19.6800566608577,-27.230211420678,-3.90460446975071));
#65322=CARTESIAN_POINT('Ctrl Pts',(-20.7520277927271,-27.0309364869423,
-5.08230700100516));
#65323=CARTESIAN_POINT('Ctrl Pts',(-21.328545241257,-26.9408345358146,-5.5257234492484));
#65324=CARTESIAN_POINT('Ctrl Pts',(-22.6156966073873,-26.8122687238307,
-6.11918487834519));
#65325=CARTESIAN_POINT('Ctrl Pts',(-23.3263251783663,-26.7757599690515,
-6.26966331470342));
#65326=CARTESIAN_POINT('Ctrl Pts',(-24.6736748216337,-26.7757599690515,
-6.26966331470342));
#65327=CARTESIAN_POINT('Ctrl Pts',(-25.3843033926127,-26.8122687238307,
-6.11918487834519));
#65328=CARTESIAN_POINT('Ctrl Pts',(-26.671454758743,-26.9408345358146,-5.5257234492484));
#65329=CARTESIAN_POINT('Ctrl Pts',(-27.2479722072729,-27.0309364869423,
-5.08230700100516));
#65330=CARTESIAN_POINT('Ctrl Pts',(-28.3199433391423,-27.230211420678,-3.90460446975071));
#65331=CARTESIAN_POINT('Ctrl Pts',(-28.7936546451677,-27.3486548092588,
-3.0322593031978));
#65332=CARTESIAN_POINT('Ctrl Pts',(-29.3824695534085,-27.4923164791461,
-1.14719857365593));
#65333=CARTESIAN_POINT('Ctrl Pts',(-29.5,-27.5154319978194,-0.135082218585487));
#65334=CARTESIAN_POINT('Ctrl Pts',(-29.5,-27.4528451038414,2.02682423429658));
#65335=CARTESIAN_POINT('Ctrl Pts',(-29.2991578031577,-27.3256746578734,
3.34500173130745));
#65336=CARTESIAN_POINT('Ctrl Pts',(-28.5722718501261,-26.8979580454901,
5.86356256779912));
#65337=CARTESIAN_POINT('Ctrl Pts',(-28.0518071989057,-26.5980125778779,
7.06565470065933));
#65338=CARTESIAN_POINT('Ctrl Pts',(-27.2355862096322,-26.1896244767548,
8.39410853029323));
#65339=CARTESIAN_POINT('Ctrl Pts',(-27.0199814070906,-26.0859415162294,
8.71061639897562));
#65340=CARTESIAN_POINT('Ctrl Pts',(-26.7834228083186,-25.9817095809707,
9.01114683323346));
#65341=CARTESIAN_POINT('Origin',(-24.,0.,0.));
#65342=CARTESIAN_POINT('',(-9.,-6.78785292759886,6.64643157139886));
#65343=CARTESIAN_POINT('',(-24.,-6.78785292759886,6.64643157139886));
#65344=CARTESIAN_POINT('',(-9.,6.64643157139886,-6.78785292759886));
#65345=CARTESIAN_POINT('Origin',(-9.,0.,0.));
#65346=CARTESIAN_POINT('',(-24.,6.64643157139886,-6.78785292759886));
#65347=CARTESIAN_POINT('Origin',(-9.,15.9099025767,-15.9099025767));
#65348=CARTESIAN_POINT('',(-9.,7.88424061023497,-8.02566196643497));
#65349=CARTESIAN_POINT('',(-9.,7.88424061023497,-8.02566196643497));
#65350=CARTESIAN_POINT('Origin',(-24.,5.48007755379487,-22.8041936936052));
#65351=CARTESIAN_POINT('',(-21.5,14.0714249456,-14.2128463018001));
#65352=CARTESIAN_POINT('',(-21.5,5.48007755379487,-22.8041936936052));
#65353=CARTESIAN_POINT('Origin',(-24.,14.0714249456,-14.2128463018001));
#65354=CARTESIAN_POINT('Origin',(-28.4,-22.6274169975687,5.65685424983145));
#65355=CARTESIAN_POINT('Origin',(-24.,-22.6274169975687,5.65685424983145));
#65356=CARTESIAN_POINT('',(-20.7,-22.6274169975687,5.65685424983145));
#65357=CARTESIAN_POINT('Origin',(-24.,-22.6274169975687,5.65685424983145));
#65358=CARTESIAN_POINT('Origin',(-24.,-19.4454364822292,8.8388347651709));
#65359=CARTESIAN_POINT('',(-20.7,-16.2634559668898,12.0208152805104));
#65360=CARTESIAN_POINT('Origin',(-24.,-16.2634559668898,12.0208152805104));
#65361=CARTESIAN_POINT('',(-20.7,-19.4454364822292,8.8388347651709));
#65362=CARTESIAN_POINT('Origin',(-26.9,-16.2634559668898,12.0208152805104));
#65363=CARTESIAN_POINT('',(-21.5,-16.2634559668898,12.0208152805104));
#65364=CARTESIAN_POINT('Origin',(-24.,-16.2634559668898,12.0208152805104));
#65365=CARTESIAN_POINT('Origin',(-24.,-5.48007755379487,22.8041936936052));
#65366=CARTESIAN_POINT('',(-21.5,-14.2128463018,14.0714249456001));
#65367=CARTESIAN_POINT('Origin',(-24.,-14.2128463018,14.0714249456001));
#65368=CARTESIAN_POINT('',(-21.5,-5.48007755379487,22.8041936936052));
#65369=CARTESIAN_POINT('Origin',(-16.,-0.070710678130059,-0.0707106780699435));
#65370=CARTESIAN_POINT('Origin',(-16.,-0.070710678130059,-0.0707106780699435));
#65371=CARTESIAN_POINT('Origin',(-24.,-28.1074945517644,0.176776695635716));
#65372=CARTESIAN_POINT('Origin',(-24.,28.1074945517644,-0.176776695635716));
#65373=CARTESIAN_POINT('',(-26.7834228083186,25.9817095809707,-9.0111468332335));
#65374=CARTESIAN_POINT('',(-21.2165771916814,25.9817095809707,-9.01114683323349));
#65375=CARTESIAN_POINT('Origin',(-24.,22.6274169975687,-5.65685424983145));
#65376=CARTESIAN_POINT('Ctrl Pts',(-26.7834228083186,25.9817095809707,-9.01114683323346));
#65377=CARTESIAN_POINT('Ctrl Pts',(-27.0199814070906,26.0859415162294,-8.71061639897562));
#65378=CARTESIAN_POINT('Ctrl Pts',(-27.2355862096322,26.1896244767548,-8.39410853029323));
#65379=CARTESIAN_POINT('Ctrl Pts',(-28.0518071989057,26.5980125778779,-7.06565470065933));
#65380=CARTESIAN_POINT('Ctrl Pts',(-28.5722718501261,26.8979580454901,-5.86356256779912));
#65381=CARTESIAN_POINT('Ctrl Pts',(-29.2991578031577,27.3256746578734,-3.34500173130745));
#65382=CARTESIAN_POINT('Ctrl Pts',(-29.5,27.4528451038414,-2.02682423429658));
#65383=CARTESIAN_POINT('Ctrl Pts',(-29.5,27.5154319978194,0.135082218585487));
#65384=CARTESIAN_POINT('Ctrl Pts',(-29.3824695534085,27.4923164791461,1.14719857365593));
#65385=CARTESIAN_POINT('Ctrl Pts',(-28.7936546451677,27.3486548092588,3.0322593031978));
#65386=CARTESIAN_POINT('Ctrl Pts',(-28.3199433391423,27.230211420678,3.90460446975071));
#65387=CARTESIAN_POINT('Ctrl Pts',(-27.2479722072729,27.0309364869423,5.08230700100516));
#65388=CARTESIAN_POINT('Ctrl Pts',(-26.671454758743,26.9408345358146,5.5257234492484));
#65389=CARTESIAN_POINT('Ctrl Pts',(-25.3843033926127,26.8122687238307,6.11918487834519));
#65390=CARTESIAN_POINT('Ctrl Pts',(-24.6736748216337,26.7757599690515,6.26966331470342));
#65391=CARTESIAN_POINT('Ctrl Pts',(-23.3263251783663,26.7757599690515,6.26966331470342));
#65392=CARTESIAN_POINT('Ctrl Pts',(-22.6156966073873,26.8122687238307,6.11918487834518));
#65393=CARTESIAN_POINT('Ctrl Pts',(-21.328545241257,26.9408345358146,5.52572344924839));
#65394=CARTESIAN_POINT('Ctrl Pts',(-20.7520277927271,27.0309364869423,5.08230700100516));
#65395=CARTESIAN_POINT('Ctrl Pts',(-19.6800566608577,27.230211420678,3.90460446975071));
#65396=CARTESIAN_POINT('Ctrl Pts',(-19.2063453548323,27.3486548092588,3.0322593031978));
#65397=CARTESIAN_POINT('Ctrl Pts',(-18.6175304465915,27.4923164791461,1.14719857365593));
#65398=CARTESIAN_POINT('Ctrl Pts',(-18.5,27.5154319978194,0.135082218585486));
#65399=CARTESIAN_POINT('Ctrl Pts',(-18.5,27.4528451038414,-2.02682423429658));
#65400=CARTESIAN_POINT('Ctrl Pts',(-18.7008421968423,27.3256746578734,-3.34500173130745));
#65401=CARTESIAN_POINT('Ctrl Pts',(-19.4277281498739,26.8979580454901,-5.86356256779912));
#65402=CARTESIAN_POINT('Ctrl Pts',(-19.9481928010943,26.5980125778779,-7.06565470065933));
#65403=CARTESIAN_POINT('Ctrl Pts',(-20.7644137903678,26.1896244767548,-8.39410853029323));
#65404=CARTESIAN_POINT('Ctrl Pts',(-20.9800185929094,26.0859415162294,-8.71061639897562));
#65405=CARTESIAN_POINT('Ctrl Pts',(-21.2165771916814,25.9817095809707,-9.01114683323346));
#65406=CARTESIAN_POINT('Origin',(-16.,0.0707106781072506,0.070710678167366));
#65407=CARTESIAN_POINT('',(-39.,-18.3139296501367,18.4553510064113));
#65408=CARTESIAN_POINT('',(-37.5,-19.3745972391984,19.516018595473));
#65409=CARTESIAN_POINT('',(-38.25,-18.8442634446675,18.9856848009421));
#65410=CARTESIAN_POINT('',(-39.,-6.64643157136116,6.78785292763578));
#65411=CARTESIAN_POINT('',(-39.,-3.17928932187772,3.32071067815234));
#65412=CARTESIAN_POINT('',(-9.,-6.64643157136116,6.78785292763578));
#65413=CARTESIAN_POINT('',(-24.,-6.64643157136116,6.78785292763578));
#65414=CARTESIAN_POINT('',(-9.,-19.3745972391984,19.516018595473));
#65415=CARTESIAN_POINT('',(-9.,8.02566196647228,-7.88424061019766));
#65416=CARTESIAN_POINT('',(-15.25,-19.3745972391984,19.516018595473));
#65417=CARTESIAN_POINT('',(-21.5,-14.0714249455627,14.2128463018374));
#65418=CARTESIAN_POINT('Origin',(-24.,-14.0714249455627,14.2128463018374));
#65419=CARTESIAN_POINT('Origin',(-24.,-5.48007755379487,22.8041936936052));
#65420=CARTESIAN_POINT('',(-24.,-4.72956268912343,27.0902424642094));
#65421=CARTESIAN_POINT('',(-21.5,-0.795787808628118,27.4884834387719));
#65422=CARTESIAN_POINT('Ctrl Pts',(-21.5,-0.795787808628116,27.4884834387719));
#65423=CARTESIAN_POINT('Ctrl Pts',(-21.5,-0.351095281866489,27.501357226159));
#65424=CARTESIAN_POINT('Ctrl Pts',(-21.5586819382303,0.132127593799674,
27.5034337727556));
#65425=CARTESIAN_POINT('Ctrl Pts',(-21.8359982780237,1.04038440540881,27.4840667670191));
#65426=CARTESIAN_POINT('Ctrl Pts',(-22.0548369471758,1.46536445881011,27.4630238360419));
#65427=CARTESIAN_POINT('Ctrl Pts',(-22.5416783856529,2.03730160051001,27.4254298732512));
#65428=CARTESIAN_POINT('Ctrl Pts',(-22.7968722688247,2.25352124915401,27.4079090802056));
#65429=CARTESIAN_POINT('Ctrl Pts',(-23.3723171754149,2.54794284417893,27.3821077345433));
#65430=CARTESIAN_POINT('Ctrl Pts',(-23.6928549082306,2.62563132929186,27.3743686707592));
#65431=CARTESIAN_POINT('Ctrl Pts',(-24.3071450917694,2.62563132929186,27.3743686707592));
#65432=CARTESIAN_POINT('Ctrl Pts',(-24.6276828245851,2.54794284417893,27.3821077345433));
#65433=CARTESIAN_POINT('Ctrl Pts',(-25.2031277311753,2.25352124915401,27.4079090802056));
#65434=CARTESIAN_POINT('Ctrl Pts',(-25.4583216143471,2.03730160051001,27.4254298732512));
#65435=CARTESIAN_POINT('Ctrl Pts',(-25.9451630528242,1.46536445881011,27.4630238360419));
#65436=CARTESIAN_POINT('Ctrl Pts',(-26.1640017219763,1.04038440540881,27.4840667670191));
#65437=CARTESIAN_POINT('Ctrl Pts',(-26.4413180617697,0.132127593799674,
27.5034337727556));
#65438=CARTESIAN_POINT('Ctrl Pts',(-26.5,-0.351095281866489,27.501357226159));
#65439=CARTESIAN_POINT('Ctrl Pts',(-26.5,-1.29514612764106,27.4740270842301));
#65440=CARTESIAN_POINT('Ctrl Pts',(-26.4267189640484,-1.83467613548264,
27.4435694082118));
#65441=CARTESIAN_POINT('Ctrl Pts',(-26.124867389821,-2.86152046064611,27.3555705260108));
#65442=CARTESIAN_POINT('Ctrl Pts',(-25.8980213172196,-3.34936228446823,
27.2982789021101));
#65443=CARTESIAN_POINT('Ctrl Pts',(-25.4199810017133,-4.00649576099619,
27.2078036326968));
#65444=CARTESIAN_POINT('Ctrl Pts',(-25.1823324639049,-4.25837971422122,
27.1689143482003));
#65445=CARTESIAN_POINT('Ctrl Pts',(-24.769562290029,-4.53014788237278,27.1244573394495));
#65446=CARTESIAN_POINT('Ctrl Pts',(-24.6225767382909,-4.60348624022732,
27.1119971008064));
#65447=CARTESIAN_POINT('Ctrl Pts',(-24.3173127716233,-4.70319063996839,
27.0948822448621));
#65448=CARTESIAN_POINT('Ctrl Pts',(-24.1590354871528,-4.72956268912345,
27.0902424642093));
#65449=CARTESIAN_POINT('Ctrl Pts',(-24.,-4.72956268912345,27.0902424642093));
#65450=CARTESIAN_POINT('Ctrl Pts',(-24.,-4.72956268912345,27.0902424642093));
#65451=CARTESIAN_POINT('Ctrl Pts',(-23.8409645128472,-4.72956268912345,
27.0902424642093));
#65452=CARTESIAN_POINT('Ctrl Pts',(-23.6826872283767,-4.70319063996839,
27.0948822448621));
#65453=CARTESIAN_POINT('Ctrl Pts',(-23.3774232617091,-4.60348624022732,
27.1119971008064));
#65454=CARTESIAN_POINT('Ctrl Pts',(-23.230437709971,-4.53014788237278,27.1244573394495));
#65455=CARTESIAN_POINT('Ctrl Pts',(-22.8176675360951,-4.25837971422122,
27.1689143482003));
#65456=CARTESIAN_POINT('Ctrl Pts',(-22.5800189982867,-4.00649576099619,
27.2078036326968));
#65457=CARTESIAN_POINT('Ctrl Pts',(-22.1019786827804,-3.34936228446823,
27.2982789021101));
#65458=CARTESIAN_POINT('Ctrl Pts',(-21.875132610179,-2.86152046064611,27.3555705260108));
#65459=CARTESIAN_POINT('Ctrl Pts',(-21.5732810359516,-1.83467613548264,
27.4435694082118));
#65460=CARTESIAN_POINT('Ctrl Pts',(-21.5,-1.29514612764106,27.4740270842301));
#65461=CARTESIAN_POINT('Ctrl Pts',(-21.5,-0.795787808628117,27.4884834387719));
#65462=CARTESIAN_POINT('',(-21.5,-5.48007755379487,22.8041936936052));
#65463=CARTESIAN_POINT('Origin',(-24.,5.48007755379487,-22.8041936936052));
#65464=CARTESIAN_POINT('',(-21.5,14.2128463018373,-14.0714249455628));
#65465=CARTESIAN_POINT('Origin',(-24.,14.2128463018373,-14.0714249455628));
#65466=CARTESIAN_POINT('',(-21.5,16.2634559668897,-12.0208152805104));
#65467=CARTESIAN_POINT('',(-21.5,5.48007755379487,-22.8041936936052));
#65468=CARTESIAN_POINT('Origin',(-24.,16.2634559668898,-12.0208152805104));
#65469=CARTESIAN_POINT('Origin',(-26.9,16.2634559668898,-12.0208152805104));
#65470=CARTESIAN_POINT('',(-20.7,16.2634559668898,-12.0208152805104));
#65471=CARTESIAN_POINT('Origin',(-24.,16.2634559668898,-12.0208152805104));
#65472=CARTESIAN_POINT('Origin',(-24.,19.4454364822292,-8.8388347651709));
#65473=CARTESIAN_POINT('',(-20.7,22.6274169975687,-5.65685424983145));
#65474=CARTESIAN_POINT('',(-20.7,19.4454364822292,-8.8388347651709));
#65475=CARTESIAN_POINT('Origin',(-24.,22.6274169975687,-5.65685424983145));
#65476=CARTESIAN_POINT('Origin',(-28.4,22.6274169975687,-5.65685424983145));
#65477=CARTESIAN_POINT('',(-24.,25.9817095809707,-9.01114683323349));
#65478=CARTESIAN_POINT('Origin',(-16.,0.0707106781072506,0.070710678167366));
#65479=CARTESIAN_POINT('',(-37.5,19.516018595473,-19.3745972391984));
#65480=CARTESIAN_POINT('',(-39.,18.4553510064113,-18.3139296501367));
#65481=CARTESIAN_POINT('',(-38.25,18.9856848009421,-18.8442634446675));
#65482=CARTESIAN_POINT('',(-9.,19.516018595473,-19.3745972391984));
#65483=CARTESIAN_POINT('',(-15.25,19.516018595473,-19.3745972391984));
#65484=CARTESIAN_POINT('',(-9.,6.78785292763578,-6.64643157136116));
#65485=CARTESIAN_POINT('',(-9.,8.02566196647228,-7.88424061019766));
#65486=CARTESIAN_POINT('',(-39.,6.78785292763578,-6.64643157136116));
#65487=CARTESIAN_POINT('',(-24.,6.78785292763578,-6.64643157136116));
#65488=CARTESIAN_POINT('',(-39.,-3.17928932187772,3.32071067815234));
#65489=CARTESIAN_POINT('Origin',(-39.,0.,13.));
#65490=CARTESIAN_POINT('',(-39.,8.4950947355237,4.25245404848513));
#65491=CARTESIAN_POINT('Origin',(-39.,0.,0.));
#65492=CARTESIAN_POINT('',(-39.,10.8187337521138,6.57609306507525));
#65493=CARTESIAN_POINT('',(-39.,7.54567369566792,3.30303300862935));
#65494=CARTESIAN_POINT('',(-39.,6.57609306499454,10.8187337521945));
#65495=CARTESIAN_POINT('',(-39.,5.44741340857436,11.9474134086147));
#65496=CARTESIAN_POINT('',(-39.,4.25245404837755,8.49509473557755));
#65497=CARTESIAN_POINT('',(-39.,3.30303300854864,7.54567369574863));
#65498=CARTESIAN_POINT('Origin',(-39.,0.,0.));
#65499=CARTESIAN_POINT('Origin',(-39.,0.,0.));
#65500=CARTESIAN_POINT('Origin',(-38.25,0.,0.));
#65501=CARTESIAN_POINT('Origin',(-37.5,0.,0.));
#65502=CARTESIAN_POINT('Origin',(-9.,15.9099025767,-15.9099025767));
#65503=CARTESIAN_POINT('',(-9.,26.2865401242261,-8.07884944143965));
#65504=CARTESIAN_POINT('Origin',(-9.,0.,0.));
#65505=CARTESIAN_POINT('',(-9.,17.244648771018,-2.97860517091918));
#65506=CARTESIAN_POINT('Origin',(-9.,15.9099025767,-15.9099025767));
#65507=CARTESIAN_POINT('',(-9.,17.244648771018,2.97860517091918));
#65508=CARTESIAN_POINT('Origin',(-9.,0.,0.));
#65509=CARTESIAN_POINT('',(-9.,26.2865401242261,8.07884944143965));
#65510=CARTESIAN_POINT('Origin',(-9.,15.9099025767,15.9099025767));
#65511=CARTESIAN_POINT('',(-9.,8.07884944143965,26.2865401242261));
#65512=CARTESIAN_POINT('Origin',(-9.,0.,0.));
#65513=CARTESIAN_POINT('',(-9.,2.97860517091918,17.244648771018));
#65514=CARTESIAN_POINT('Origin',(-9.,15.9099025767,15.9099025767));
#65515=CARTESIAN_POINT('',(-9.,-2.97860517091918,17.244648771018));
#65516=CARTESIAN_POINT('Origin',(-9.,0.,0.));
#65517=CARTESIAN_POINT('',(-9.,-8.07884944143965,26.2865401242261));
#65518=CARTESIAN_POINT('Origin',(-9.,-15.9099025767,15.9099025767));
#65519=CARTESIAN_POINT('Origin',(-9.,0.,0.));
#65520=CARTESIAN_POINT('',(-9.,4.25245404837755,8.49509473557755));
#65521=CARTESIAN_POINT('Origin',(-9.,0.,0.));
#65522=CARTESIAN_POINT('',(-9.,6.57609306499454,10.8187337521945));
#65523=CARTESIAN_POINT('',(-9.,0.0530330085486312,4.29567369574864));
#65524=CARTESIAN_POINT('',(-9.,10.8187337521138,6.57609306507525));
#65525=CARTESIAN_POINT('',(-9.,16.6523646969244,0.742462120264717));
#65526=CARTESIAN_POINT('',(-9.,8.4950947355237,4.25245404848513));
#65527=CARTESIAN_POINT('',(-9.,4.29567369566792,0.0530330086293516));
#65528=CARTESIAN_POINT('Origin',(-9.,0.,0.));
#65529=CARTESIAN_POINT('Origin',(-24.,0.,0.));
#65530=CARTESIAN_POINT('',(-24.,4.25245404837755,8.49509473557755));
#65531=CARTESIAN_POINT('Origin',(-24.,0.,0.));
#65532=CARTESIAN_POINT('',(-24.,8.4950947355237,4.25245404848513));
#65533=CARTESIAN_POINT('Origin',(-15.25,0.,0.));
#65534=CARTESIAN_POINT('',(-3.7202200813,-0.2994444445,27.498369643029));
#65535=CARTESIAN_POINT('',(-4.3435534146,-0.2994444445,27.498369643029));
#65536=CARTESIAN_POINT('',(-4.03188674795,-0.2994444445,27.498369643029));
#65537=CARTESIAN_POINT('',(-4.3435534146,-1.1061111111,27.4777458720671));
#65538=CARTESIAN_POINT('Ctrl Pts',(-4.3435534146,-0.2994444445,27.498369643029));
#65539=CARTESIAN_POINT('Ctrl Pts',(-4.39419602744118,-0.2994444445,27.498369643029));
#65540=CARTESIAN_POINT('Ctrl Pts',(-4.44821405117923,-0.309565273785878,
27.4982652712794));
#65541=CARTESIAN_POINT('Ctrl Pts',(-4.54758440972013,-0.350724834122933,
27.4977711038395));
#65542=CARTESIAN_POINT('Ctrl Pts',(-4.59293670765284,-0.381763557784472,
27.4973733109335));
#65543=CARTESIAN_POINT('Ctrl Pts',(-4.66456223528332,-0.453385171307823,
27.4962856562635));
#65544=CARTESIAN_POINT('Ctrl Pts',(-4.69560557365306,-0.498744419672721,
27.4955218892374));
#65545=CARTESIAN_POINT('Ctrl Pts',(-4.7367677324877,-0.598121989127674,
27.493539605584));
#65546=CARTESIAN_POINT('Ctrl Pts',(-4.7468867479,-0.652140069806569,27.4923130926182));
#65547=CARTESIAN_POINT('Ctrl Pts',(-4.7468867479,-0.753430235839141,27.4897237204729));
#65548=CARTESIAN_POINT('Ctrl Pts',(-4.73676246101481,-0.80745512421137,
27.4881881502515));
#65549=CARTESIAN_POINT('Ctrl Pts',(-4.69559144465381,-0.906836412476876,
27.4850890353706));
#65550=CARTESIAN_POINT('Ctrl Pts',(-4.66454479714166,-0.952193095307298,
27.4835334801247));
#65551=CARTESIAN_POINT('Ctrl Pts',(-4.59292152712871,-1.0238019031852,27.4809590925011));
#65552=CARTESIAN_POINT('Ctrl Pts',(-4.54757596140155,-1.054834879545,27.479769785307));
#65553=CARTESIAN_POINT('Ctrl Pts',(-4.44821406584017,-1.09598961694164,
27.4781591602539));
#65554=CARTESIAN_POINT('Ctrl Pts',(-4.39419749547155,-1.1061111111,27.4777458720671));
#65555=CARTESIAN_POINT('Ctrl Pts',(-4.3435534146,-1.1061111111,27.4777458720671));
#65556=CARTESIAN_POINT('',(-3.7202200813,-1.1061111111,27.4777458720671));
#65557=CARTESIAN_POINT('',(-4.03188674795,-1.1061111111,27.4777458720671));
#65558=CARTESIAN_POINT('Origin',(-3.7202200813,0.,0.));
#65559=CARTESIAN_POINT('Origin',(-29.,9.72271824131503,9.72271824131503));
#65560=CARTESIAN_POINT('',(-31.1,8.69741340859454,8.69741340859454));
#65561=CARTESIAN_POINT('Origin',(-29.,8.69741340859454,8.69741340859454));
#65562=CARTESIAN_POINT('',(-31.1,19.4454364826301,19.4454364826301));
#65563=CARTESIAN_POINT('',(-31.1,9.72271824131503,9.72271824131503));
#65564=CARTESIAN_POINT('',(-26.9,19.4454364826301,19.4454364826301));
#65565=CARTESIAN_POINT('Ctrl Pts',(-26.9,19.4454364826301,19.4454364826301));
#65566=CARTESIAN_POINT('Ctrl Pts',(-26.9,19.2589082724023,19.6319646928578));
#65567=CARTESIAN_POINT('Ctrl Pts',(-26.9527396524836,19.0570372826678,19.827917294343));
#65568=CARTESIAN_POINT('Ctrl Pts',(-27.167084371912,18.6805067132861,20.1830533656328));
#65569=CARTESIAN_POINT('Ctrl Pts',(-27.3286837627136,18.5059934629633,20.3423953731785));
#65570=CARTESIAN_POINT('Ctrl Pts',(-27.7014679712018,18.2281408464247,20.5917392401225));
#65571=CARTESIAN_POINT('Ctrl Pts',(-27.9375391926626,18.1062776437531,20.6984118527539));
#65572=CARTESIAN_POINT('Ctrl Pts',(-28.4549053217882,17.9439937491035,20.8392569853186));
#65573=CARTESIAN_POINT('Ctrl Pts',(-28.7362089711958,17.9037322369437,20.8735807179272));
#65574=CARTESIAN_POINT('Ctrl Pts',(-29.2637910288042,17.9037322369437,20.8735807179272));
#65575=CARTESIAN_POINT('Ctrl Pts',(-29.5450946782118,17.9439937491035,20.8392569853186));
#65576=CARTESIAN_POINT('Ctrl Pts',(-30.0624608073374,18.1062776437531,20.6984118527539));
#65577=CARTESIAN_POINT('Ctrl Pts',(-30.2985320287982,18.2281408464247,20.5917392401225));
#65578=CARTESIAN_POINT('Ctrl Pts',(-30.6713162372864,18.5059934629633,20.3423953731785));
#65579=CARTESIAN_POINT('Ctrl Pts',(-30.832915628088,18.6805067132861,20.1830533656328));
#65580=CARTESIAN_POINT('Ctrl Pts',(-31.0472603475164,19.0570372826678,19.827917294343));
#65581=CARTESIAN_POINT('Ctrl Pts',(-31.1,19.2589082724023,19.6319646928578));
#65582=CARTESIAN_POINT('Ctrl Pts',(-31.1,19.4454364826301,19.4454364826301));
#65583=CARTESIAN_POINT('',(-29.,20.8735807179272,17.9037322369437));
#65584=CARTESIAN_POINT('Ctrl Pts',(-29.,20.8735807179272,17.9037322369437));
#65585=CARTESIAN_POINT('Ctrl Pts',(-28.9409243315885,20.8735807179272,17.9037322369437));
#65586=CARTESIAN_POINT('Ctrl Pts',(-28.8823185723426,20.8719561180177,17.9056270228153));
#65587=CARTESIAN_POINT('Ctrl Pts',(-28.8241875429964,20.868766419503,17.9093441853626));
#65588=CARTESIAN_POINT('Ctrl Pts',(-28.7651735233883,20.8655282705693,17.9131178103254));
#65589=CARTESIAN_POINT('Ctrl Pts',(-28.7066479020686,20.8606771585548,17.9187695517304));
#65590=CARTESIAN_POINT('Ctrl Pts',(-28.6486082424822,20.8542378533544,17.9262611346121));
#65591=CARTESIAN_POINT('Ctrl Pts',(-28.5905518731159,20.8477966942601,17.9337548743414));
#65592=CARTESIAN_POINT('Ctrl Pts',(-28.5329808778428,20.8397663253161,17.9430896171325));
#65593=CARTESIAN_POINT('Ctrl Pts',(-28.475898465847,20.8301348968028,17.954263695967));
#65594=CARTESIAN_POINT('Ctrl Pts',(-28.4194214387268,20.8206056139583,17.9653192686261));
#65595=CARTESIAN_POINT('Ctrl Pts',(-28.3634218934566,20.809508840884,17.978175580729));
#65596=CARTESIAN_POINT('Ctrl Pts',(-28.307920773518,20.7967996666906,17.9928644519354));
#65597=CARTESIAN_POINT('Ctrl Pts',(-28.2704559732151,20.7882206204714,18.0027798487244));
#65598=CARTESIAN_POINT('Ctrl Pts',(-28.233218662767,20.7789061710475,18.01353096647));
#65599=CARTESIAN_POINT('Ctrl Pts',(-28.1962227045941,20.7688345408256,18.0251355561008));
#65600=CARTESIAN_POINT('Ctrl Pts',(-28.1419909449969,20.7540707056415,18.0421465309792));
#65601=CARTESIAN_POINT('Ctrl Pts',(-28.0891325289024,20.7379131154835,18.0607204150564));
#65602=CARTESIAN_POINT('Ctrl Pts',(-28.0376128730261,20.7204071307495,18.0807817717886));
#65603=CARTESIAN_POINT('Ctrl Pts',(-27.9853278203101,20.7026410700278,18.1011411681483));
#65604=CARTESIAN_POINT('Ctrl Pts',(-27.9344207901101,20.6834860586877,18.1230327563019));
#65605=CARTESIAN_POINT('Ctrl Pts',(-27.8848692043026,20.662952907283,18.1464142890666));
#65606=CARTESIAN_POINT('Ctrl Pts',(-27.835309647837,20.6424164530025,18.1697995828855));
#65607=CARTESIAN_POINT('Ctrl Pts',(-27.7871052343873,20.6205010894759,18.1946756264686));
#65608=CARTESIAN_POINT('Ctrl Pts',(-27.7402584745463,20.5971853396141,18.2210324451026));
#65609=CARTESIAN_POINT('Ctrl Pts',(-27.6939156433813,20.5741203963182,18.2471057445187));
#65610=CARTESIAN_POINT('Ctrl Pts',(-27.6489008029551,20.5496846281942,18.2746285373045));
#65611=CARTESIAN_POINT('Ctrl Pts',(-27.6052508789822,20.5238311574231,18.3036172535751));
#65612=CARTESIAN_POINT('Ctrl Pts',(-27.5745062838357,20.505621400804,18.3240353039275));
#65613=CARTESIAN_POINT('Ctrl Pts',(-27.5444395295393,20.4867077633294,18.3451811575672));
#65614=CARTESIAN_POINT('Ctrl Pts',(-27.5150764042051,20.4670676659985,18.3670667542599));
#65615=CARTESIAN_POINT('Ctrl Pts',(-27.4739307803984,20.4395466154596,18.3977343524141));
#65616=CARTESIAN_POINT('Ctrl Pts',(-27.4348258110997,20.4110406080958,18.4293596244423));
#65617=CARTESIAN_POINT('Ctrl Pts',(-27.397693251414,20.3815788026156,18.4618845126644));
#65618=CARTESIAN_POINT('Ctrl Pts',(-27.3600131663981,20.3516825782612,18.494888985389));
#65619=CARTESIAN_POINT('Ctrl Pts',(-27.32436345212,20.3208017675861,18.5288201934746));
#65620=CARTESIAN_POINT('Ctrl Pts',(-27.2907051878983,20.2889367073675,18.5636476038707));
#65621=CARTESIAN_POINT('Ctrl Pts',(-27.2570404826908,20.257065549318,18.5984816789854));
#65622=CARTESIAN_POINT('Ctrl Pts',(-27.225367491637,20.224209272259,18.6342127921753));
#65623=CARTESIAN_POINT('Ctrl Pts',(-27.1956878552695,20.1903450809994,18.6708335250196));
#65624=CARTESIAN_POINT('Ctrl Pts',(-27.1663254278762,20.1568428222527,18.7070628640827));
#65625=CARTESIAN_POINT('Ctrl Pts',(-27.138913630464,20.1223535486345,18.7441634385671));
#65626=CARTESIAN_POINT('Ctrl Pts',(-27.1134998926827,20.0868402088014,18.7821430446352));
#65627=CARTESIAN_POINT('Ctrl Pts',(-27.0945077136319,20.0603004012924,18.810525940726));
#65628=CARTESIAN_POINT('Ctrl Pts',(-27.0766323337211,20.0331883084273,18.8394001223222));
#65629=CARTESIAN_POINT('Ctrl Pts',(-27.0599121975429,20.0054856370759,18.868771672389));
#65630=CARTESIAN_POINT('Ctrl Pts',(-27.0375591557561,19.9684501151328,18.9080383074801));
#65631=CARTESIAN_POINT('Ctrl Pts',(-27.0176337763097,19.9309625884957,18.9475518440566));
#65632=CARTESIAN_POINT('Ctrl Pts',(-27.000049650795,19.893040530158,18.9872827250967));
#65633=CARTESIAN_POINT('Ctrl Pts',(-26.9822027462842,19.8545517606461,19.0276073485451));
#65634=CARTESIAN_POINT('Ctrl Pts',(-26.9667672171665,19.8156148371944,19.0681563988552));
#65635=CARTESIAN_POINT('Ctrl Pts',(-26.9536989008189,19.7762288706783,19.1089181312319));
#65636=CARTESIAN_POINT('Ctrl Pts',(-26.9406270335039,19.7368322020733,19.1496909395251));
#65637=CARTESIAN_POINT('Ctrl Pts',(-26.9299234702477,19.6969856526238,19.1906771391979));
#65638=CARTESIAN_POINT('Ctrl Pts',(-26.9215940204688,19.6566779068226,19.2318754015355));
#65639=CARTESIAN_POINT('Ctrl Pts',(-26.9133527431819,19.6167968439941,19.2726375542201));
#65640=CARTESIAN_POINT('Ctrl Pts',(-26.9074355517788,19.5764637104953,19.3136078904466));
#65641=CARTESIAN_POINT('Ctrl Pts',(-26.9038985506748,19.5356661328462,19.354786536779));
#65642=CARTESIAN_POINT('Ctrl Pts',(-26.9013126263588,19.5058387607383,19.3848925106586));
#65643=CARTESIAN_POINT('Ctrl Pts',(-26.9,19.4757630666449,19.4151098986153));
#65644=CARTESIAN_POINT('Ctrl Pts',(-26.9,19.4454364826301,19.4454364826301));
#65645=CARTESIAN_POINT('Ctrl Pts',(-31.1,19.4454364826301,19.4454364826301));
#65646=CARTESIAN_POINT('Ctrl Pts',(-31.1,19.6319646928578,19.2589082724023));
#65647=CARTESIAN_POINT('Ctrl Pts',(-31.0472603475164,19.827917294343,19.0570372826678));
#65648=CARTESIAN_POINT('Ctrl Pts',(-30.832915628088,20.1830533656328,18.6805067132861));
#65649=CARTESIAN_POINT('Ctrl Pts',(-30.6713162372864,20.3423953731785,18.5059934629633));
#65650=CARTESIAN_POINT('Ctrl Pts',(-30.2985320287982,20.5917392401225,18.2281408464247));
#65651=CARTESIAN_POINT('Ctrl Pts',(-30.0624608073374,20.6984118527539,18.1062776437531));
#65652=CARTESIAN_POINT('Ctrl Pts',(-29.5450946782118,20.8392569853186,17.9439937491035));
#65653=CARTESIAN_POINT('Ctrl Pts',(-29.2637910288042,20.8735807179272,17.9037322369437));
#65654=CARTESIAN_POINT('Ctrl Pts',(-29.,20.8735807179272,17.9037322369437));
#65655=CARTESIAN_POINT('Origin',(-24.,6.47002704781655,2.22738636077798));
#65656=CARTESIAN_POINT('',(-24.,10.8187337521138,6.57609306507525));
#65657=CARTESIAN_POINT('Origin',(-24.,2.22738636069727,6.47002704789727));
#65658=CARTESIAN_POINT('',(-24.,6.57609306499454,10.8187337521945));
#65659=CARTESIAN_POINT('Origin',(-24.,8.69741340855418,8.69741340863489));
#65660=CARTESIAN_POINT('Origin',(-1.,-15.9099025767,15.9099025767));
#65661=CARTESIAN_POINT('',(7.,-8.07884944143965,26.2865401242261));
#65662=CARTESIAN_POINT('',(7.,-2.97860517091918,17.244648771018));
#65663=CARTESIAN_POINT('Origin',(7.,-15.9099025767,15.9099025767));
#65664=CARTESIAN_POINT('',(-1.,-8.07884944143965,26.2865401242261));
#65665=CARTESIAN_POINT('',(-1.,-2.97860517091918,17.244648771018));
#65666=CARTESIAN_POINT('Origin',(-1.,15.9099025767,15.9099025767));
#65667=CARTESIAN_POINT('',(7.,26.2865401242261,8.07884944143965));
#65668=CARTESIAN_POINT('',(7.,17.244648771018,2.97860517091918));
#65669=CARTESIAN_POINT('Origin',(7.,15.9099025767,15.9099025767));
#65670=CARTESIAN_POINT('',(-1.,26.2865401242261,8.07884944143965));
#65671=CARTESIAN_POINT('',(-1.,17.244648771018,2.97860517091918));
#65672=CARTESIAN_POINT('Origin',(-1.,15.9099025767,-15.9099025767));
#65673=CARTESIAN_POINT('',(7.,26.2865401242261,-8.07884944143965));
#65674=CARTESIAN_POINT('',(-1.,26.2865401242261,-8.07884944143965));
#65675=CARTESIAN_POINT('',(7.,17.244648771018,-2.97860517091918));
#65676=CARTESIAN_POINT('Origin',(7.,15.9099025767,-15.9099025767));
#65677=CARTESIAN_POINT('',(-1.,17.244648771018,-2.97860517091918));
#65678=CARTESIAN_POINT('Origin',(-1.,0.,0.));
#65679=CARTESIAN_POINT('',(7.,2.97860517091918,17.244648771018));
#65680=CARTESIAN_POINT('Origin',(7.,0.,0.));
#65681=CARTESIAN_POINT('',(-1.,2.97860517091918,17.244648771018));
#65682=CARTESIAN_POINT('Origin',(-1.,0.,0.));
#65683=CARTESIAN_POINT('Origin',(7.,0.,0.));
#65684=CARTESIAN_POINT('Origin',(-1.,15.9099025767,15.9099025767));
#65685=CARTESIAN_POINT('',(7.,8.07884944143965,26.2865401242261));
#65686=CARTESIAN_POINT('',(-1.,8.07884944143965,26.2865401242261));
#65687=CARTESIAN_POINT('Origin',(7.,15.9099025767,15.9099025767));
#65688=CARTESIAN_POINT('Origin',(7.,0.,13.75));
#65689=CARTESIAN_POINT('Origin',(7.,0.,0.));
#65690=CARTESIAN_POINT('Origin',(7.,0.,13.75));
#65691=CARTESIAN_POINT('Origin',(7.,0.,0.));
#65692=CARTESIAN_POINT('Origin',(-15.25,0.,0.));
#65693=CARTESIAN_POINT('',(-4.3435534146,-2.1388888889,27.4166948102965));
#65694=CARTESIAN_POINT('',(-5.18767834635794,0.459060516890588,27.4961681592514));
#65695=CARTESIAN_POINT('Ctrl Pts',(-5.18767834635794,0.459060516890587,
27.4961681592514));
#65696=CARTESIAN_POINT('Ctrl Pts',(-5.24965809277248,0.414029595245434,
27.4969199701236));
#65697=CARTESIAN_POINT('Ctrl Pts',(-5.30712124170086,0.364629158505802,
27.4976316978157));
#65698=CARTESIAN_POINT('Ctrl Pts',(-5.48660165044913,0.185124728033571,
27.4996725546973));
#65699=CARTESIAN_POINT('Ctrl Pts',(-5.59711475871681,0.0236269477990792,
27.5005588966783));
#65700=CARTESIAN_POINT('Ctrl Pts',(-5.74364605565176,-0.330191593200779,
27.4985867159418));
#65701=CARTESIAN_POINT('Ctrl Pts',(-5.7796645257,-0.522511665581369,27.4956269007824));
#65702=CARTESIAN_POINT('Ctrl Pts',(-5.7796645257,-0.883231079115617,27.4864055040933));
#65703=CARTESIAN_POINT('Ctrl Pts',(-5.74357914128894,-1.07563756694651,
27.4795264541498));
#65704=CARTESIAN_POINT('Ctrl Pts',(-5.59693543031386,-1.42950329514698,
27.4633918271089));
#65705=CARTESIAN_POINT('Ctrl Pts',(-5.4863803371174,-1.5909684685238,27.4542371442706));
#65706=CARTESIAN_POINT('Ctrl Pts',(-5.2314028462211,-1.84584631737978,27.4382787767415));
#65707=CARTESIAN_POINT('Ctrl Pts',(-5.06999631183931,-1.9563112878812,27.4304254942484));
#65708=CARTESIAN_POINT('Ctrl Pts',(-4.71625542419335,-2.1028344711005,27.4195821238672));
#65709=CARTESIAN_POINT('Ctrl Pts',(-4.52391635613999,-2.1388888889,27.4166948102965));
#65710=CARTESIAN_POINT('Ctrl Pts',(-4.3435534146,-2.1388888889,27.4166948102965));
#65711=CARTESIAN_POINT('',(-5.7631397208,2.1388888889,27.4166948102965));
#65712=CARTESIAN_POINT('Origin',(-5.03051074634245,0.000272929993637497,
-3.21571077187848));
#65713=CARTESIAN_POINT('',(-4.7295794663,2.1388888889,27.4166948102965));
#65714=CARTESIAN_POINT('',(-5.24635959355,2.1388888889,27.4166948102965));
#65715=CARTESIAN_POINT('',(-4.2292347159,0.6783333333,27.491632615924));
#65716=CARTESIAN_POINT('Origin',(-3.9969811813186,0.000362414293276214,
-3.21399783711568));
#65717=CARTESIAN_POINT('',(-3.7202200813,0.6783333333,27.491632615924));
#65718=CARTESIAN_POINT('',(-3.9747273986,0.6783333333,27.491632615924));
#65719=CARTESIAN_POINT('',(-3.7202200813,2.1388888889,27.4166948102965));
#65720=CARTESIAN_POINT('Origin',(-3.7202200813,0.,0.));
#65721=CARTESIAN_POINT('',(-2.7424423035,2.1388888889,27.4166948102965));
#65722=CARTESIAN_POINT('',(-3.2313311924,2.1388888889,27.4166948102965));
#65723=CARTESIAN_POINT('',(-2.7424423035,-2.1388888889,27.4166948102965));
#65724=CARTESIAN_POINT('Origin',(-2.7424423035,0.,0.));
#65725=CARTESIAN_POINT('',(-3.54299785905,-2.1388888889,27.4166948102965));
#65726=CARTESIAN_POINT('',(-1.4888888889,-1.1611111111,27.4754767199348));
#65727=CARTESIAN_POINT('',(-1.4888888889,2.1388888889,27.4166948102965));
#65728=CARTESIAN_POINT('Origin',(-1.4888888889,0.,0.));
#65729=CARTESIAN_POINT('',(-0.5111111111,2.1388888889,27.4166948102965));
#65730=CARTESIAN_POINT('',(-1.,2.1388888889,27.4166948102965));
#65731=CARTESIAN_POINT('',(-0.5111111111,-1.1611111111,27.4754767199348));
#65732=CARTESIAN_POINT('Origin',(-0.5111111111,0.,0.));
#65733=CARTESIAN_POINT('',(0.5277777778,-1.1611111111,27.4754767199348));
#65734=CARTESIAN_POINT('',(0.00833333335000042,-1.1611111111,27.4754767199348));
#65735=CARTESIAN_POINT('',(0.5277777778,-2.1388888889,27.4166948102965));
#65736=CARTESIAN_POINT('Origin',(0.527777777800001,0.,0.));
#65737=CARTESIAN_POINT('',(-2.5277777778,-2.1388888889,27.4166948102965));
#65738=CARTESIAN_POINT('',(-1.,-2.1388888889,27.4166948102965));
#65739=CARTESIAN_POINT('',(-2.5277777778,-1.1611111111,27.4754767199348));
#65740=CARTESIAN_POINT('Origin',(-2.5277777778,0.,0.));
#65741=CARTESIAN_POINT('',(-2.00833333335,-1.1611111111,27.4754767199348));
#65742=CARTESIAN_POINT('',(3.7631397208,2.75,27.362154520432));
#65743=CARTESIAN_POINT('',(1.8075841652,2.75,27.362154520432));
#65744=CARTESIAN_POINT('',(2.785361943,2.75,27.362154520432));
#65745=CARTESIAN_POINT('',(-1.,4.3709594736,27.150409081267));
#65746=CARTESIAN_POINT('Origin',(6.57072389467804,-5.08186381864562E-9,
-3.39134897942017E-8));
#65747=CARTESIAN_POINT('',(-3.8075841652,2.75,27.362154520432));
#65748=CARTESIAN_POINT('Origin',(-8.57072394033692,-3.14535625323131E-8,
-2.40405939599952E-7));
#65749=CARTESIAN_POINT('',(-5.7631397208,2.75,27.362154520432));
#65750=CARTESIAN_POINT('',(-4.785361943,2.75,27.362154520432));
#65751=CARTESIAN_POINT('',(-1.,5.5,26.944387170615));
#65752=CARTESIAN_POINT('Origin',(-10.5262794172666,1.40492439903994E-8,
9.1254430678589E-8));
#65753=CARTESIAN_POINT('Origin',(8.52627943337224,4.74967842833962E-9,2.95255420112994E-8));
#65754=CARTESIAN_POINT('',(1.9747474276,-0.2016666667,27.4992605456136));
#65755=CARTESIAN_POINT('',(0.5561396937,2.1388888889,27.4166948102965));
#65756=CARTESIAN_POINT('Origin',(1.85251751839491,0.,0.));
#65757=CARTESIAN_POINT('',(1.6994942043,2.1388888889,27.4166948102965));
#65758=CARTESIAN_POINT('',(1.127816949,2.1388888889,27.4166948102965));
#65759=CARTESIAN_POINT('',(2.785361943,0.3473197978,27.4978066208572));
#65760=CARTESIAN_POINT('Origin',(2.9955115927225,0.000594682442375816,-10.0686161186405));
#65761=CARTESIAN_POINT('',(2.785361943,2.1388888889,27.4166948102965));
#65762=CARTESIAN_POINT('Origin',(2.785361943,0.,0.));
#65763=CARTESIAN_POINT('',(3.7631397208,2.1388888889,27.4166948102965));
#65764=CARTESIAN_POINT('',(3.2742508319,2.1388888889,27.4166948102965));
#65765=CARTESIAN_POINT('',(3.7631397208,-2.1388888889,27.4166948102965));
#65766=CARTESIAN_POINT('Origin',(3.7631397208,0.,0.));
#65767=CARTESIAN_POINT('',(2.785361943,-2.1388888889,27.4166948102965));
#65768=CARTESIAN_POINT('',(3.2742508319,-2.1388888889,27.4166948102965));
#65769=CARTESIAN_POINT('',(2.785361943,-0.7484330612,27.4898135307045));
#65770=CARTESIAN_POINT('Origin',(2.785361943,0.,0.));
#65771=CARTESIAN_POINT('',(1.8474876449,-2.1388888889,27.4166948102965));
#65772=CARTESIAN_POINT('Origin',(3.28939526747748,-0.001172927507095,-12.4577275280589));
#65773=CARTESIAN_POINT('',(0.6680745397,-2.1388888889,27.4166948102965));
#65774=CARTESIAN_POINT('',(1.2577810923,-2.1388888889,27.4166948102965));
#65775=CARTESIAN_POINT('Origin',(2.11077331185338,0.,0.));
#65776=CARTESIAN_POINT('',(-1.,-4.3709594736,27.150409081267));
#65777=CARTESIAN_POINT('',(1.8075841652,-2.75,27.362154520432));
#65778=CARTESIAN_POINT('Origin',(6.57072389476503,5.14153497555014E-9,-3.42402284303489E-8));
#65779=CARTESIAN_POINT('',(3.7631397208,-2.75,27.362154520432));
#65780=CARTESIAN_POINT('',(2.785361943,-2.75,27.362154520432));
#65781=CARTESIAN_POINT('',(-1.,-5.5,26.944387170615));
#65782=CARTESIAN_POINT('Origin',(8.5262794280497,-7.82302223001352E-9,5.00813346349105E-8));
#65783=CARTESIAN_POINT('',(-5.7631397208,-2.75,27.362154520432));
#65784=CARTESIAN_POINT('Origin',(-10.5262794294935,-6.98918367625367E-9,
4.45900916190567E-8));
#65785=CARTESIAN_POINT('',(-3.8075841652,-2.75,27.362154520432));
#65786=CARTESIAN_POINT('',(-4.785361943,-2.75,27.362154520432));
#65787=CARTESIAN_POINT('Origin',(-8.57072394746809,3.55609436342164E-8,
-2.70109778988115E-7));
#65788=CARTESIAN_POINT('Origin',(-1.,0.,0.));
#65789=CARTESIAN_POINT('',(-1.4888888889,2.1388888889,26.9151473026053));
#65790=CARTESIAN_POINT('',(-1.4888888889,-1.1611111111,26.9750221684372));
#65791=CARTESIAN_POINT('Origin',(-1.4888888889,0.,0.));
#65792=CARTESIAN_POINT('',(-2.5277777778,-1.1611111111,26.9750221684372));
#65793=CARTESIAN_POINT('',(-2.00833333335,-1.1611111111,26.9750221684372));
#65794=CARTESIAN_POINT('',(-2.5277777778,-2.1388888889,26.9151473026053));
#65795=CARTESIAN_POINT('Origin',(-2.5277777778,0.,0.));
#65796=CARTESIAN_POINT('',(0.5277777778,-2.1388888889,26.9151473026053));
#65797=CARTESIAN_POINT('',(-1.,-2.1388888889,26.9151473026053));
#65798=CARTESIAN_POINT('',(0.5277777778,-1.1611111111,26.9750221684372));
#65799=CARTESIAN_POINT('Origin',(0.5277777778,0.,0.));
#65800=CARTESIAN_POINT('',(-0.5111111111,-1.1611111111,26.9750221684372));
#65801=CARTESIAN_POINT('',(0.00833333334999997,-1.1611111111,26.9750221684372));
#65802=CARTESIAN_POINT('',(-0.5111111111,2.1388888889,26.9151473026053));
#65803=CARTESIAN_POINT('Origin',(-0.5111111111,0.,0.));
#65804=CARTESIAN_POINT('',(-1.,2.1388888889,26.9151473026053));
#65805=CARTESIAN_POINT('Origin',(-0.5111111111,0.4888888889,0.));
#65806=CARTESIAN_POINT('',(-0.5111111111,2.1388888889,0.));
#65807=CARTESIAN_POINT('',(-0.5111111111,-1.1611111111,0.));
#65808=CARTESIAN_POINT('Origin',(-1.,2.1388888889,0.));
#65809=CARTESIAN_POINT('',(-1.4888888889,2.1388888889,0.));
#65810=CARTESIAN_POINT('Origin',(0.00833333334999997,-1.1611111111,0.));
#65811=CARTESIAN_POINT('',(0.5277777778,-1.1611111111,0.));
#65812=CARTESIAN_POINT('Origin',(0.5277777778,-1.65,0.));
#65813=CARTESIAN_POINT('',(0.5277777778,-2.1388888889,0.));
#65814=CARTESIAN_POINT('Origin',(-1.,-2.1388888889,0.));
#65815=CARTESIAN_POINT('',(-2.5277777778,-2.1388888889,0.));
#65816=CARTESIAN_POINT('Origin',(-2.5277777778,-1.65,0.));
#65817=CARTESIAN_POINT('',(-2.5277777778,-1.1611111111,0.));
#65818=CARTESIAN_POINT('Origin',(-2.00833333335,-1.1611111111,0.));
#65819=CARTESIAN_POINT('',(-1.4888888889,-1.1611111111,0.));
#65820=CARTESIAN_POINT('Origin',(-1.4888888889,0.4888888889,0.));
#65821=CARTESIAN_POINT('Origin',(2.24242807365,1.24310434335,0.));
#65822=CARTESIAN_POINT('',(1.6994942043,2.1388888889,26.9151473026053));
#65823=CARTESIAN_POINT('',(1.6994942043,2.1388888889,0.));
#65824=CARTESIAN_POINT('',(2.785361943,0.3473197978,26.9977659993944));
#65825=CARTESIAN_POINT('Origin',(2.99587202900024,0.,0.));
#65826=CARTESIAN_POINT('',(2.785361943,0.3473197978,0.));
#65827=CARTESIAN_POINT('Origin',(1.127816949,2.1388888889,0.));
#65828=CARTESIAN_POINT('',(0.5561396937,2.1388888889,26.9151473026053));
#65829=CARTESIAN_POINT('',(0.5561396937,2.1388888889,0.));
#65830=CARTESIAN_POINT('',(1.127816949,2.1388888889,26.9151473026053));
#65831=CARTESIAN_POINT('Origin',(1.26544356065,0.9686111111,0.));
#65832=CARTESIAN_POINT('',(1.9747474276,-0.2016666667,26.9992468516354));
#65833=CARTESIAN_POINT('',(1.9747474276,-0.2016666667,0.));
#65834=CARTESIAN_POINT('Origin',(1.85251751839491,0.,0.));
#65835=CARTESIAN_POINT('Origin',(1.2577810923,-2.1388888889,0.));
#65836=CARTESIAN_POINT('',(1.8474876449,-2.1388888889,26.9151473026053));
#65837=CARTESIAN_POINT('',(1.8474876449,-2.1388888889,0.));
#65838=CARTESIAN_POINT('',(0.6680745397,-2.1388888889,26.9151473026053));
#65839=CARTESIAN_POINT('',(1.2577810923,-2.1388888889,26.9151473026053));
#65840=CARTESIAN_POINT('',(0.6680745397,-2.1388888889,0.));
#65841=CARTESIAN_POINT('Origin',(2.31642479395,-1.44366097505,0.));
#65842=CARTESIAN_POINT('',(2.785361943,-0.7484330612,26.9896248205288));
#65843=CARTESIAN_POINT('',(2.785361943,-0.7484330612,0.));
#65844=CARTESIAN_POINT('Origin',(3.289365669055,-0.00121680896187332,-12.2292518146672));
#65845=CARTESIAN_POINT('Origin',(2.785361943,-1.44366097505,0.));
#65846=CARTESIAN_POINT('',(2.785361943,-2.1388888889,26.9151473026053));
#65847=CARTESIAN_POINT('',(2.785361943,-2.1388888889,0.));
#65848=CARTESIAN_POINT('Origin',(2.785361943,0.,0.));
#65849=CARTESIAN_POINT('Origin',(3.2742508319,-2.1388888889,0.));
#65850=CARTESIAN_POINT('',(3.7631397208,-2.1388888889,26.9151473026053));
#65851=CARTESIAN_POINT('',(3.7631397208,-2.1388888889,0.));
#65852=CARTESIAN_POINT('',(3.2742508319,-2.1388888889,26.9151473026053));
#65853=CARTESIAN_POINT('Origin',(3.7631397208,0.,0.));
#65854=CARTESIAN_POINT('',(3.7631397208,2.1388888889,26.9151473026053));
#65855=CARTESIAN_POINT('',(3.7631397208,2.1388888889,0.));
#65856=CARTESIAN_POINT('Origin',(3.7631397208,0.,0.));
#65857=CARTESIAN_POINT('Origin',(3.2742508319,2.1388888889,0.));
#65858=CARTESIAN_POINT('',(2.785361943,2.1388888889,26.9151473026053));
#65859=CARTESIAN_POINT('',(2.785361943,2.1388888889,0.));
#65860=CARTESIAN_POINT('',(3.2742508319,2.1388888889,26.9151473026053));
#65861=CARTESIAN_POINT('Origin',(2.785361943,1.24310434335,0.));
#65862=CARTESIAN_POINT('Origin',(2.785361943,0.,0.));
#65863=CARTESIAN_POINT('Origin',(1.32141098365,-1.1702777778,0.));
#65864=CARTESIAN_POINT('Origin',(2.11077331185338,0.,0.));
#65865=CARTESIAN_POINT('Origin',(-1.,0.,0.));
#65866=CARTESIAN_POINT('Origin',(-1.,0.,0.));
#65867=CARTESIAN_POINT('',(-1.,5.5,26.4338797757726));
#65868=CARTESIAN_POINT('',(-5.7631397208,2.75,26.8595886044444));
#65869=CARTESIAN_POINT('Origin',(-10.5262794446456,-1.76125336537325E-9,
-1.09255759994653E-8));
#65870=CARTESIAN_POINT('',(-3.8075841652,2.75,26.8595886044444));
#65871=CARTESIAN_POINT('',(-4.785361943,2.75,26.8595886044444));
#65872=CARTESIAN_POINT('',(-1.,4.3709594736,26.6438494456065));
#65873=CARTESIAN_POINT('Origin',(-8.57072391451643,-1.65472496815866E-8,
-1.22794205914545E-7));
#65874=CARTESIAN_POINT('',(1.8075841652,2.75,26.8595886044444));
#65875=CARTESIAN_POINT('Origin',(6.57072386138071,1.41313644119734E-8,1.099020696671E-7));
#65876=CARTESIAN_POINT('',(3.7631397208,2.75,26.8595886044444));
#65877=CARTESIAN_POINT('',(2.785361943,2.75,26.8595886044444));
#65878=CARTESIAN_POINT('Origin',(8.52627943983032,1.0193068611386E-9,6.87394141607456E-9));
#65879=CARTESIAN_POINT('Origin',(-2.4037920826,3.5604797368,0.));
#65880=CARTESIAN_POINT('',(-1.,4.3709594736,0.));
#65881=CARTESIAN_POINT('',(-3.8075841652,2.75,0.));
#65882=CARTESIAN_POINT('Origin',(0.4037920826,3.5604797368,0.));
#65883=CARTESIAN_POINT('',(1.8075841652,2.75,0.));
#65884=CARTESIAN_POINT('Origin',(-4.785361943,2.75,0.));
#65885=CARTESIAN_POINT('',(-5.7631397208,2.75,0.));
#65886=CARTESIAN_POINT('Origin',(-3.3815698604,4.125,0.));
#65887=CARTESIAN_POINT('',(-1.,5.5,0.));
#65888=CARTESIAN_POINT('Origin',(1.3815698604,4.125,0.));
#65889=CARTESIAN_POINT('',(3.7631397208,2.75,0.));
#65890=CARTESIAN_POINT('Origin',(2.785361943,2.75,0.));
#65891=CARTESIAN_POINT('Origin',(-4.785361943,-2.75,0.));
#65892=CARTESIAN_POINT('',(-5.7631397208,-2.75,26.8595886044444));
#65893=CARTESIAN_POINT('',(-5.7631397208,-2.75,0.));
#65894=CARTESIAN_POINT('',(-3.8075841652,-2.75,26.8595886044444));
#65895=CARTESIAN_POINT('',(-4.785361943,-2.75,26.8595886044444));
#65896=CARTESIAN_POINT('',(-3.8075841652,-2.75,0.));
#65897=CARTESIAN_POINT('Origin',(-3.3815698604,-4.125,0.));
#65898=CARTESIAN_POINT('',(-1.,-5.5,26.4338797757726));
#65899=CARTESIAN_POINT('',(-1.,-5.5,0.));
#65900=CARTESIAN_POINT('Origin',(-10.5262794408649,-4.21045975862455E-10,
2.9073410345859E-9));
#65901=CARTESIAN_POINT('Origin',(1.3815698604,-4.125,0.));
#65902=CARTESIAN_POINT('',(3.7631397208,-2.75,26.8595886044444));
#65903=CARTESIAN_POINT('',(3.7631397208,-2.75,0.));
#65904=CARTESIAN_POINT('Origin',(8.52627944157111,-1.4747092436096E-11,
2.30344632257129E-10));
#65905=CARTESIAN_POINT('Origin',(2.785361943,-2.75,0.));
#65906=CARTESIAN_POINT('',(1.8075841652,-2.75,26.8595886044444));
#65907=CARTESIAN_POINT('',(1.8075841652,-2.75,0.));
#65908=CARTESIAN_POINT('',(2.785361943,-2.75,26.8595886044444));
#65909=CARTESIAN_POINT('Origin',(-2.4037920826,-3.5604797368,0.));
#65910=CARTESIAN_POINT('',(-1.,-4.3709594736,26.6438494456065));
#65911=CARTESIAN_POINT('Origin',(-8.5707238773724,-4.8968212817968E-9,4.16328171937153E-8));
#65912=CARTESIAN_POINT('',(-1.,-4.3709594736,0.));
#65913=CARTESIAN_POINT('Origin',(0.4037920826,-3.5604797368,0.));
#65914=CARTESIAN_POINT('Origin',(6.57072379448721,-5.27513027703819E-8,
3.97860180356702E-7));
#65915=CARTESIAN_POINT('Origin',(-1.,0.,0.));
#65916=CARTESIAN_POINT('Origin',(-4.4794070911,1.4086111111,0.));
#65917=CARTESIAN_POINT('',(-4.7295794663,2.1388888889,26.9151473026053));
#65918=CARTESIAN_POINT('',(-4.7295794663,2.1388888889,0.));
#65919=CARTESIAN_POINT('',(-4.2292347159,0.6783333333,26.9914776158871));
#65920=CARTESIAN_POINT('Origin',(-3.9969858265374,0.000375974154255831,
-3.15507438280649));
#65921=CARTESIAN_POINT('',(-4.2292347159,0.6783333333,0.));
#65922=CARTESIAN_POINT('Origin',(-5.24635959355,2.1388888889,0.));
#65923=CARTESIAN_POINT('',(-5.7631397208,2.1388888889,26.9151473026053));
#65924=CARTESIAN_POINT('',(-5.7631397208,2.1388888889,0.));
#65925=CARTESIAN_POINT('',(-5.24635959355,2.1388888889,26.9151473026053));
#65926=CARTESIAN_POINT('Origin',(-5.47540903359635,1.29897470288934,0.));
#65927=CARTESIAN_POINT('',(-5.18767834635794,0.459060516890588,26.9960971890722));
#65928=CARTESIAN_POINT('',(-5.18767834635794,0.459060516890588,0.));
#65929=CARTESIAN_POINT('Origin',(-5.03051424673138,0.000283144313856232,
-3.15681890149318));
#65930=CARTESIAN_POINT('Origin',(-4.3435534146,-0.7027777778,0.));
#65931=CARTESIAN_POINT('',(-4.3435534146,-2.1388888889,26.9151473026053));
#65932=CARTESIAN_POINT('',(-4.3435534146,-2.1388888889,0.));
#65933=CARTESIAN_POINT('Ctrl Pts',(-4.3435534146,-2.1388888889,26.9151473026053));
#65934=CARTESIAN_POINT('Ctrl Pts',(-4.52391792341369,-2.1388888889,26.9151473026053));
#65935=CARTESIAN_POINT('Ctrl Pts',(-4.71625693450842,-2.10283382592968,
26.918088482717));
#65936=CARTESIAN_POINT('Ctrl Pts',(-5.06999455179236,-1.95631203649358,
26.9291336821038));
#65937=CARTESIAN_POINT('Ctrl Pts',(-5.23139805095757,-1.84584924667606,
26.9371329701837));
#65938=CARTESIAN_POINT('Ctrl Pts',(-5.48637421277749,-1.59097645605588,
26.9533878020362));
#65939=CARTESIAN_POINT('Ctrl Pts',(-5.59693050287028,-1.42951212256183,
26.9627125508631));
#65940=CARTESIAN_POINT('Ctrl Pts',(-5.74357733669248,-1.07564498446733,
26.979146778132));
#65941=CARTESIAN_POINT('Ctrl Pts',(-5.7796645257,-0.883236025485049,26.9861535121304));
#65942=CARTESIAN_POINT('Ctrl Pts',(-5.7796645257,-0.522513729514313,26.9955458651961));
#65943=CARTESIAN_POINT('Ctrl Pts',(-5.7436467578758,-0.330194423649562,
26.9985605075207));
#65944=CARTESIAN_POINT('Ctrl Pts',(-5.59711654864042,0.0236237606196166,
27.0005692486945));
#65945=CARTESIAN_POINT('Ctrl Pts',(-5.48660381528006,0.185121924893265,
26.9996665127352));
#65946=CARTESIAN_POINT('Ctrl Pts',(-5.30712307306233,0.364627587033973,
26.9975878598176));
#65947=CARTESIAN_POINT('Ctrl Pts',(-5.24965906631465,0.414028887925648,
26.9968629383849));
#65948=CARTESIAN_POINT('Ctrl Pts',(-5.18767834635794,0.459060516890587,
26.9960971890722));
#65949=CARTESIAN_POINT('Origin',(-3.54299785905,-2.1388888889,0.));
#65950=CARTESIAN_POINT('',(-2.7424423035,-2.1388888889,26.9151473026053));
#65951=CARTESIAN_POINT('',(-2.7424423035,-2.1388888889,0.));
#65952=CARTESIAN_POINT('',(-3.54299785905,-2.1388888889,26.9151473026053));
#65953=CARTESIAN_POINT('Origin',(-3.7202200813,-0.7027777778,0.));
#65954=CARTESIAN_POINT('',(-3.7202200813,-1.1061111111,26.9773334154787));
#65955=CARTESIAN_POINT('',(-3.7202200813,-1.1061111111,0.));
#65956=CARTESIAN_POINT('',(-3.7202200813,-0.2994444445,26.9983394493931));
#65957=CARTESIAN_POINT('Origin',(-3.7202200813,0.,0.));
#65958=CARTESIAN_POINT('',(-3.7202200813,-0.2994444445,0.));
#65959=CARTESIAN_POINT('Origin',(-4.03188674795,-1.1061111111,0.));
#65960=CARTESIAN_POINT('',(-4.3435534146,-1.1061111111,26.9773334154787));
#65961=CARTESIAN_POINT('',(-4.3435534146,-1.1061111111,0.));
#65962=CARTESIAN_POINT('',(-4.03188674795,-1.1061111111,26.9773334154787));
#65963=CARTESIAN_POINT('Origin',(-2.7424423035,0.,0.));
#65964=CARTESIAN_POINT('',(-2.7424423035,2.1388888889,26.9151473026053));
#65965=CARTESIAN_POINT('',(-2.7424423035,2.1388888889,0.));
#65966=CARTESIAN_POINT('Origin',(-2.7424423035,0.,0.));
#65967=CARTESIAN_POINT('Origin',(-3.2313311924,2.1388888889,0.));
#65968=CARTESIAN_POINT('',(-3.7202200813,2.1388888889,26.9151473026053));
#65969=CARTESIAN_POINT('',(-3.7202200813,2.1388888889,0.));
#65970=CARTESIAN_POINT('',(-3.2313311924,2.1388888889,26.9151473026053));
#65971=CARTESIAN_POINT('Origin',(-3.7202200813,1.4086111111,0.));
#65972=CARTESIAN_POINT('',(-3.7202200813,0.6783333333,26.9914776158871));
#65973=CARTESIAN_POINT('',(-3.7202200813,0.6783333333,0.));
#65974=CARTESIAN_POINT('Origin',(-3.7202200813,0.,0.));
#65975=CARTESIAN_POINT('Origin',(-3.9747273986,0.6783333333,0.));
#65976=CARTESIAN_POINT('',(-3.9747273986,0.6783333333,26.9914776158871));
#65977=CARTESIAN_POINT('Origin',(-4.3435534146,-0.7027777778,0.));
#65978=CARTESIAN_POINT('',(-4.3435534146,-0.2994444445,26.9983394493931));
#65979=CARTESIAN_POINT('',(-4.3435534146,-0.2994444445,0.));
#65980=CARTESIAN_POINT('Ctrl Pts',(-4.3435534146,-1.1061111111,26.9773334154787));
#65981=CARTESIAN_POINT('Ctrl Pts',(-4.39419751981262,-1.1061111111,26.9773334154787));
#65982=CARTESIAN_POINT('Ctrl Pts',(-4.44821399727505,-1.09598960220443,
26.9777543707312));
#65983=CARTESIAN_POINT('Ctrl Pts',(-4.54757547767286,-1.05483512303673,
26.9793948590167));
#65984=CARTESIAN_POINT('Ctrl Pts',(-4.59292073016298,-1.02380242963024,
26.9806062123945));
#65985=CARTESIAN_POINT('Ctrl Pts',(-4.66454409879151,-0.952194064006125,
26.9832283238713));
#65986=CARTESIAN_POINT('Ctrl Pts',(-4.69559097470685,-0.906837278676475,
26.9848127252447));
#65987=CARTESIAN_POINT('Ctrl Pts',(-4.73676234178596,-0.807455680198994,
26.9879693009873));
#65988=CARTESIAN_POINT('Ctrl Pts',(-4.7468867479,-0.753430573531451,26.989533338241));
#65989=CARTESIAN_POINT('Ctrl Pts',(-4.7468867479,-0.652140283928571,26.9921706971532));
#65990=CARTESIAN_POINT('Ctrl Pts',(-4.73676781048986,-0.598122239682042,
26.9934199350385));
#65991=CARTESIAN_POINT('Ctrl Pts',(-4.69560563233662,-0.498744499118134,
26.9954389467467));
#65992=CARTESIAN_POINT('Ctrl Pts',(-4.66456218935101,-0.453385052203247,
26.9962168650025));
#65993=CARTESIAN_POINT('Ctrl Pts',(-4.59293647859085,-0.381763401892919,
26.9973246659964));
#65994=CARTESIAN_POINT('Ctrl Pts',(-4.54758424200201,-0.350724746147987,
26.9977298257009));
#65995=CARTESIAN_POINT('Ctrl Pts',(-4.44821398195441,-0.309565263618254,
26.9982331447194));
#65996=CARTESIAN_POINT('Ctrl Pts',(-4.39419599674402,-0.2994444445,26.9983394493931));
#65997=CARTESIAN_POINT('Ctrl Pts',(-4.3435534146,-0.2994444445,26.9983394493931));
#65998=CARTESIAN_POINT('Origin',(-4.03188674795,-0.2994444445,0.));
#65999=CARTESIAN_POINT('',(-4.03188674795,-0.2994444445,26.9983394493931));
#66000=CARTESIAN_POINT('Origin',(-1.,0.,0.));
#66001=CARTESIAN_POINT('',(0.,0.,0.));
#66002=CARTESIAN_POINT('',(0.,0.,0.));
#66003=CARTESIAN_POINT('',(0.,0.,0.));
#66004=CARTESIAN_POINT('',(0.,0.,0.));
#66005=CARTESIAN_POINT('',(0.,0.,0.));
#66006=CARTESIAN_POINT('',(0.,0.,0.));
#66007=CARTESIAN_POINT('',(0.,0.,0.));
#66008=CARTESIAN_POINT('',(0.,0.,0.));
#66009=CARTESIAN_POINT('',(0.,0.,0.));
#66010=CARTESIAN_POINT('',(0.,0.,0.));
#66011=CARTESIAN_POINT('',(0.,0.,0.));
#66012=CARTESIAN_POINT('Origin',(-480.,-24.5,0.));
#66013=CARTESIAN_POINT('',(-480.,-7.49999999999999,2.5));
#66014=CARTESIAN_POINT('Origin',(-480.,-7.49999999999999,0.));
#66015=CARTESIAN_POINT('',(-480.,-24.5,2.5));
#66016=CARTESIAN_POINT('',(-480.,-24.5,2.5));
#66017=CARTESIAN_POINT('Origin',(-480.,-24.5,0.));
#66018=CARTESIAN_POINT('Origin',(-480.,-7.49999999999999,0.));
#66019=CARTESIAN_POINT('',(-480.,-5.99784845243109,0.));
#66020=CARTESIAN_POINT('',(-480.,-7.49999999999999,2.5));
#66021=CARTESIAN_POINT('Origin',(-420.,-24.5,0.));
#66022=CARTESIAN_POINT('',(-420.,-7.49999999999999,2.5));
#66023=CARTESIAN_POINT('Origin',(-420.,-7.49999999999999,0.));
#66024=CARTESIAN_POINT('',(-420.,-24.5,2.5));
#66025=CARTESIAN_POINT('',(-420.,-24.5,2.5));
#66026=CARTESIAN_POINT('Origin',(-420.,-24.5,0.));
#66027=CARTESIAN_POINT('Origin',(-420.,-7.49999999999999,0.));
#66028=CARTESIAN_POINT('',(-420.,-5.99784845243109,0.));
#66029=CARTESIAN_POINT('',(-420.,-7.49999999999999,2.5));
#66030=CARTESIAN_POINT('Origin',(-360.,-24.5,0.));
#66031=CARTESIAN_POINT('',(-360.,-7.49999999999999,2.5));
#66032=CARTESIAN_POINT('Origin',(-360.,-7.49999999999999,0.));
#66033=CARTESIAN_POINT('',(-360.,-24.5,2.5));
#66034=CARTESIAN_POINT('',(-360.,-24.5,2.5));
#66035=CARTESIAN_POINT('Origin',(-360.,-24.5,0.));
#66036=CARTESIAN_POINT('Origin',(-360.,-7.49999999999999,0.));
#66037=CARTESIAN_POINT('',(-360.,-5.99784845243109,0.));
#66038=CARTESIAN_POINT('',(-360.,-7.49999999999999,2.5));
#66039=CARTESIAN_POINT('Origin',(-300.,-24.5,0.));
#66040=CARTESIAN_POINT('',(-300.,-7.49999999999999,2.5));
#66041=CARTESIAN_POINT('Origin',(-300.,-7.49999999999999,0.));
#66042=CARTESIAN_POINT('',(-300.,-24.5,2.5));
#66043=CARTESIAN_POINT('',(-300.,-24.5,2.5));
#66044=CARTESIAN_POINT('Origin',(-300.,-24.5,0.));
#66045=CARTESIAN_POINT('Origin',(-300.,-7.49999999999999,0.));
#66046=CARTESIAN_POINT('',(-300.,-5.99784845243109,0.));
#66047=CARTESIAN_POINT('',(-300.,-7.49999999999999,2.5));
#66048=CARTESIAN_POINT('Origin',(-240.,-24.5,0.));
#66049=CARTESIAN_POINT('',(-240.,-7.49999999999999,2.5));
#66050=CARTESIAN_POINT('Origin',(-240.,-7.49999999999999,0.));
#66051=CARTESIAN_POINT('',(-240.,-24.5,2.5));
#66052=CARTESIAN_POINT('',(-240.,-24.5,2.5));
#66053=CARTESIAN_POINT('Origin',(-240.,-24.5,0.));
#66054=CARTESIAN_POINT('Origin',(-240.,-7.49999999999999,0.));
#66055=CARTESIAN_POINT('',(-240.,-5.99784845243109,0.));
#66056=CARTESIAN_POINT('',(-240.,-7.49999999999999,2.5));
#66057=CARTESIAN_POINT('Origin',(-180.,-24.5,0.));
#66058=CARTESIAN_POINT('',(-180.,-7.49999999999999,2.5));
#66059=CARTESIAN_POINT('Origin',(-180.,-7.49999999999999,0.));
#66060=CARTESIAN_POINT('',(-180.,-24.5,2.5));
#66061=CARTESIAN_POINT('',(-180.,-24.5,2.5));
#66062=CARTESIAN_POINT('Origin',(-180.,-24.5,0.));
#66063=CARTESIAN_POINT('Origin',(-180.,-7.49999999999999,0.));
#66064=CARTESIAN_POINT('',(-180.,-5.99784845243109,0.));
#66065=CARTESIAN_POINT('',(-180.,-7.49999999999999,2.5));
#66066=CARTESIAN_POINT('Origin',(-120.,-24.5,0.));
#66067=CARTESIAN_POINT('',(-120.,-7.49999999999999,2.5));
#66068=CARTESIAN_POINT('Origin',(-120.,-7.49999999999999,0.));
#66069=CARTESIAN_POINT('',(-120.,-24.5,2.5));
#66070=CARTESIAN_POINT('',(-120.,-24.5,2.5));
#66071=CARTESIAN_POINT('Origin',(-120.,-24.5,0.));
#66072=CARTESIAN_POINT('Origin',(-120.,-7.49999999999999,0.));
#66073=CARTESIAN_POINT('',(-120.,-5.99784845243109,0.));
#66074=CARTESIAN_POINT('',(-120.,-7.49999999999999,2.5));
#66075=CARTESIAN_POINT('Origin',(-60.,-24.5,0.));
#66076=CARTESIAN_POINT('',(-60.,-7.49999999999999,2.5));
#66077=CARTESIAN_POINT('Origin',(-60.,-7.49999999999999,0.));
#66078=CARTESIAN_POINT('',(-60.,-24.5,2.5));
#66079=CARTESIAN_POINT('',(-60.,-24.5,2.5));
#66080=CARTESIAN_POINT('Origin',(-60.,-24.5,0.));
#66081=CARTESIAN_POINT('Origin',(-60.,-7.49999999999999,0.));
#66082=CARTESIAN_POINT('',(-60.,-5.99784845243109,0.));
#66083=CARTESIAN_POINT('',(-60.,-7.49999999999999,2.5));
#66084=CARTESIAN_POINT('Origin',(480.,-24.5,0.));
#66085=CARTESIAN_POINT('',(480.,-7.49999999999999,2.5));
#66086=CARTESIAN_POINT('Origin',(480.,-7.49999999999999,0.));
#66087=CARTESIAN_POINT('',(480.,-24.5,2.5));
#66088=CARTESIAN_POINT('',(480.,-24.5,2.5));
#66089=CARTESIAN_POINT('Origin',(480.,-24.5,0.));
#66090=CARTESIAN_POINT('Origin',(480.,-7.49999999999999,0.));
#66091=CARTESIAN_POINT('',(480.,-5.99784845243109,0.));
#66092=CARTESIAN_POINT('',(480.,-7.49999999999999,2.5));
#66093=CARTESIAN_POINT('Origin',(420.,-24.5,0.));
#66094=CARTESIAN_POINT('',(420.,-7.49999999999999,2.5));
#66095=CARTESIAN_POINT('Origin',(420.,-7.49999999999999,0.));
#66096=CARTESIAN_POINT('',(420.,-24.5,2.5));
#66097=CARTESIAN_POINT('',(420.,-24.5,2.5));
#66098=CARTESIAN_POINT('Origin',(420.,-24.5,0.));
#66099=CARTESIAN_POINT('Origin',(420.,-7.49999999999999,0.));
#66100=CARTESIAN_POINT('',(420.,-5.99784845243109,0.));
#66101=CARTESIAN_POINT('',(420.,-7.49999999999999,2.5));
#66102=CARTESIAN_POINT('Origin',(360.,-24.5,0.));
#66103=CARTESIAN_POINT('',(360.,-7.49999999999999,2.5));
#66104=CARTESIAN_POINT('Origin',(360.,-7.49999999999999,0.));
#66105=CARTESIAN_POINT('',(360.,-24.5,2.5));
#66106=CARTESIAN_POINT('',(360.,-24.5,2.5));
#66107=CARTESIAN_POINT('Origin',(360.,-24.5,0.));
#66108=CARTESIAN_POINT('Origin',(360.,-7.49999999999999,0.));
#66109=CARTESIAN_POINT('',(360.,-5.99784845243109,0.));
#66110=CARTESIAN_POINT('',(360.,-7.49999999999999,2.5));
#66111=CARTESIAN_POINT('Origin',(300.,-24.5,0.));
#66112=CARTESIAN_POINT('',(300.,-7.49999999999999,2.5));
#66113=CARTESIAN_POINT('Origin',(300.,-7.49999999999999,0.));
#66114=CARTESIAN_POINT('',(300.,-24.5,2.5));
#66115=CARTESIAN_POINT('',(300.,-24.5,2.5));
#66116=CARTESIAN_POINT('Origin',(300.,-24.5,0.));
#66117=CARTESIAN_POINT('Origin',(300.,-7.49999999999999,0.));
#66118=CARTESIAN_POINT('',(300.,-5.99784845243109,0.));
#66119=CARTESIAN_POINT('',(300.,-7.49999999999999,2.5));
#66120=CARTESIAN_POINT('Origin',(240.,-24.5,0.));
#66121=CARTESIAN_POINT('',(240.,-7.49999999999999,2.5));
#66122=CARTESIAN_POINT('Origin',(240.,-7.49999999999999,0.));
#66123=CARTESIAN_POINT('',(240.,-24.5,2.5));
#66124=CARTESIAN_POINT('',(240.,-24.5,2.5));
#66125=CARTESIAN_POINT('Origin',(240.,-24.5,0.));
#66126=CARTESIAN_POINT('Origin',(240.,-7.49999999999999,0.));
#66127=CARTESIAN_POINT('',(240.,-5.99784845243109,0.));
#66128=CARTESIAN_POINT('',(240.,-7.49999999999999,2.5));
#66129=CARTESIAN_POINT('Origin',(180.,-24.5,0.));
#66130=CARTESIAN_POINT('',(180.,-7.49999999999999,2.5));
#66131=CARTESIAN_POINT('Origin',(180.,-7.49999999999999,0.));
#66132=CARTESIAN_POINT('',(180.,-24.5,2.5));
#66133=CARTESIAN_POINT('',(180.,-24.5,2.5));
#66134=CARTESIAN_POINT('Origin',(180.,-24.5,0.));
#66135=CARTESIAN_POINT('Origin',(180.,-7.49999999999999,0.));
#66136=CARTESIAN_POINT('',(180.,-5.99784845243109,0.));
#66137=CARTESIAN_POINT('',(180.,-7.49999999999999,2.5));
#66138=CARTESIAN_POINT('Origin',(120.,-24.5,0.));
#66139=CARTESIAN_POINT('',(120.,-7.49999999999999,2.5));
#66140=CARTESIAN_POINT('Origin',(120.,-7.49999999999999,0.));
#66141=CARTESIAN_POINT('',(120.,-24.5,2.5));
#66142=CARTESIAN_POINT('',(120.,-24.5,2.5));
#66143=CARTESIAN_POINT('Origin',(120.,-24.5,0.));
#66144=CARTESIAN_POINT('Origin',(120.,-7.49999999999999,0.));
#66145=CARTESIAN_POINT('',(120.,-5.99784845243109,0.));
#66146=CARTESIAN_POINT('',(120.,-7.49999999999999,2.5));
#66147=CARTESIAN_POINT('Origin',(60.,-24.5,0.));
#66148=CARTESIAN_POINT('',(60.,-7.49999999999999,2.5));
#66149=CARTESIAN_POINT('Origin',(60.,-7.49999999999999,0.));
#66150=CARTESIAN_POINT('',(60.,-24.5,2.5));
#66151=CARTESIAN_POINT('',(60.,-24.5,2.5));
#66152=CARTESIAN_POINT('Origin',(60.,-24.5,0.));
#66153=CARTESIAN_POINT('Origin',(60.,-7.49999999999999,0.));
#66154=CARTESIAN_POINT('',(60.,-5.99784845243109,0.));
#66155=CARTESIAN_POINT('',(60.,-7.49999999999999,2.5));
#66156=CARTESIAN_POINT('Origin',(0.,-24.5,0.));
#66157=CARTESIAN_POINT('',(-3.06161699786838E-16,-7.49999999999999,2.5));
#66158=CARTESIAN_POINT('Origin',(0.,-7.49999999999999,0.));
#66159=CARTESIAN_POINT('',(-3.06161699786838E-16,-24.5,2.5));
#66160=CARTESIAN_POINT('',(-3.06161699786838E-16,-24.5,2.5));
#66161=CARTESIAN_POINT('Origin',(0.,-24.5,0.));
#66162=CARTESIAN_POINT('Origin',(0.,-7.49999999999999,0.));
#66163=CARTESIAN_POINT('',(-4.5317201340139E-15,-5.99784845243109,0.));
#66164=CARTESIAN_POINT('',(-3.06161699786838E-16,-7.49999999999999,2.5));
#66165=CARTESIAN_POINT('Origin',(-515.,-26.5,17.5));
#66166=CARTESIAN_POINT('',(-515.,-26.5,17.5));
#66167=CARTESIAN_POINT('',(-515.,-26.5,11.5));
#66168=CARTESIAN_POINT('',(-515.,-26.5,17.5));
#66169=CARTESIAN_POINT('',(515.,-26.5,11.5));
#66170=CARTESIAN_POINT('',(-515.,-26.5,11.5));
#66171=CARTESIAN_POINT('',(515.,-26.5,17.5));
#66172=CARTESIAN_POINT('',(515.,-26.5,17.5));
#66173=CARTESIAN_POINT('',(-515.,-26.5,17.5));
#66174=CARTESIAN_POINT('Origin',(515.,26.5,17.5));
#66175=CARTESIAN_POINT('',(515.,-24.7,11.5));
#66176=CARTESIAN_POINT('',(515.,-26.5,11.5));
#66177=CARTESIAN_POINT('',(515.,-24.5,11.3));
#66178=CARTESIAN_POINT('Origin',(515.,-24.7,11.3));
#66179=CARTESIAN_POINT('',(515.,-24.5,-11.3));
#66180=CARTESIAN_POINT('',(515.,-24.5,11.5));
#66181=CARTESIAN_POINT('',(515.,-24.7,-11.5));
#66182=CARTESIAN_POINT('Origin',(515.,-24.7,-11.3));
#66183=CARTESIAN_POINT('',(515.,-26.5,-11.5));
#66184=CARTESIAN_POINT('',(515.,-26.5,-11.5));
#66185=CARTESIAN_POINT('',(515.,-26.5,-17.5));
#66186=CARTESIAN_POINT('',(515.,-26.5,17.5));
#66187=CARTESIAN_POINT('',(515.,26.5,-17.5));
#66188=CARTESIAN_POINT('',(515.,26.5,-17.5));
#66189=CARTESIAN_POINT('',(515.,26.5,17.5));
#66190=CARTESIAN_POINT('',(515.,26.5,17.5));
#66191=CARTESIAN_POINT('',(515.,26.5,17.5));
#66192=CARTESIAN_POINT('Origin',(-515.,26.5,17.5));
#66193=CARTESIAN_POINT('',(-515.,26.5,-17.5));
#66194=CARTESIAN_POINT('',(-515.,26.5,-17.5));
#66195=CARTESIAN_POINT('',(-515.,26.5,17.5));
#66196=CARTESIAN_POINT('',(-515.,26.5,17.5));
#66197=CARTESIAN_POINT('',(-515.,26.5,17.5));
#66198=CARTESIAN_POINT('Origin',(-515.,26.5,17.5));
#66199=CARTESIAN_POINT('',(-515.,-26.5,-11.5));
#66200=CARTESIAN_POINT('',(-515.,-24.7,-11.5));
#66201=CARTESIAN_POINT('',(-515.,-26.5,-11.5));
#66202=CARTESIAN_POINT('',(-515.,-24.5,-11.3));
#66203=CARTESIAN_POINT('Origin',(-515.,-24.7,-11.3));
#66204=CARTESIAN_POINT('',(-515.,-24.5,11.3));
#66205=CARTESIAN_POINT('',(-515.,-24.5,11.5));
#66206=CARTESIAN_POINT('',(-515.,-24.7,11.5));
#66207=CARTESIAN_POINT('Origin',(-515.,-24.7,11.3));
#66208=CARTESIAN_POINT('',(-515.,-26.5,11.5));
#66209=CARTESIAN_POINT('',(-515.,26.5,17.5));
#66210=CARTESIAN_POINT('',(-515.,-26.5,-17.5));
#66211=CARTESIAN_POINT('',(-515.,26.5,-17.5));
#66212=CARTESIAN_POINT('',(-515.,-26.5,17.5));
#66213=CARTESIAN_POINT('Origin',(-515.,-26.5,17.5));
#66214=CARTESIAN_POINT('',(-515.,-26.5,-11.5));
#66215=CARTESIAN_POINT('',(-515.,-26.5,-17.5));
#66216=CARTESIAN_POINT('Origin',(0.,0.,17.5));
#66217=CARTESIAN_POINT('Origin',(0.,0.,-17.5));
#66218=CARTESIAN_POINT('Origin',(-515.,-26.5,11.5));
#66219=CARTESIAN_POINT('',(515.,-24.7,11.5));
#66220=CARTESIAN_POINT('Origin',(-515.,-24.5,11.5));
#66221=CARTESIAN_POINT('',(515.,-24.5,-11.3));
#66222=CARTESIAN_POINT('',(-515.,-24.5,11.3));
#66223=CARTESIAN_POINT('Origin',(-515.,-26.5,-11.5));
#66224=CARTESIAN_POINT('',(-515.,-24.7,-11.5));
#66225=CARTESIAN_POINT('Origin',(-515.,-24.7,-11.3));
#66226=CARTESIAN_POINT('Origin',(-515.,-24.7,11.3));
#66227=CARTESIAN_POINT('',(0.,0.,0.));
#66228=CARTESIAN_POINT('Origin',(20.,1.71450551880629E-15,0.));
#66229=CARTESIAN_POINT('',(0.,-5.,-6.12323399573677E-16));
#66230=CARTESIAN_POINT('Origin',(0.,-7.34788079488412E-16,0.));
#66231=CARTESIAN_POINT('',(-5.4,-5.,-6.12323399573677E-16));
#66232=CARTESIAN_POINT('',(20.,-5.,-6.12323399573677E-16));
#66233=CARTESIAN_POINT('Origin',(-5.4,-1.39609735102798E-15,0.));
#66234=CARTESIAN_POINT('Origin',(-5.4,-1.39609735102798E-15,0.));
#66235=CARTESIAN_POINT('',(-6.,-4.4,-5.38844591624836E-16));
#66236=CARTESIAN_POINT('',(-5.4,-5.,-6.12323399573677E-16));
#66237=CARTESIAN_POINT('Origin',(-6.,-1.46957615897682E-15,0.));
#66238=CARTESIAN_POINT('Origin',(20.,1.71450551880629E-15,0.));
#66239=CARTESIAN_POINT('',(19.4585,-3.,3.67394039744206E-16));
#66240=CARTESIAN_POINT('',(19.4585,3.,-3.67394039744206E-16));
#66241=CARTESIAN_POINT('Origin',(19.4585,1.64819089463247E-15,0.));
#66242=CARTESIAN_POINT('',(20.,2.4585,-3.01079415570377E-16));
#66243=CARTESIAN_POINT('',(20.,2.4585,-3.01079415570377E-16));
#66244=CARTESIAN_POINT('Origin',(20.,1.71450551880629E-15,0.));
#66245=CARTESIAN_POINT('Origin',(19.4585,1.64819089463247E-15,0.));
#66246=CARTESIAN_POINT('Origin',(20.,1.71450551880629E-15,0.));
#66247=CARTESIAN_POINT('',(0.,-3.,-3.67394039744206E-16));
#66248=CARTESIAN_POINT('',(20.,-3.,-3.67394039744206E-16));
#66249=CARTESIAN_POINT('Origin',(0.,-7.34788079488412E-16,0.));
#66250=CARTESIAN_POINT('Origin',(20.,2.4585,0.));
#66251=CARTESIAN_POINT('Origin',(-6.,-1.46957615897682E-15,0.));
#66252=CARTESIAN_POINT('',(-6.,1.44337567297406,2.5));
#66253=CARTESIAN_POINT('',(-6.,2.88675134594813,0.));
#66254=CARTESIAN_POINT('',(-6.,1.44337567297406,2.5));
#66255=CARTESIAN_POINT('',(-6.,-1.44337567297407,2.5));
#66256=CARTESIAN_POINT('',(-6.,-1.44337567297407,2.5));
#66257=CARTESIAN_POINT('',(-6.,-2.88675134594813,-7.77133304087269E-16));
#66258=CARTESIAN_POINT('',(-6.,-2.88675134594813,-7.77133304087269E-16));
#66259=CARTESIAN_POINT('',(-6.,-1.44337567297407,-2.5));
#66260=CARTESIAN_POINT('',(-6.,-1.44337567297407,-2.5));
#66261=CARTESIAN_POINT('',(-6.,1.44337567297406,-2.5));
#66262=CARTESIAN_POINT('',(-6.,1.44337567297406,-2.5));
#66263=CARTESIAN_POINT('',(-6.,2.88675134594813,3.50584097974525E-17));
#66264=CARTESIAN_POINT('Origin',(1.22464679914735E-16,3.,0.));
#66265=CARTESIAN_POINT('Origin',(-3.,1.44337567297406,2.5));
#66266=CARTESIAN_POINT('',(-3.,2.88675134594813,3.50584097974525E-17));
#66267=CARTESIAN_POINT('',(-3.,2.88675134594813,3.50584097974525E-17));
#66268=CARTESIAN_POINT('',(-3.,1.44337567297406,2.5));
#66269=CARTESIAN_POINT('',(-3.,1.44337567297406,2.5));
#66270=CARTESIAN_POINT('',(-3.,1.44337567297406,2.5));
#66271=CARTESIAN_POINT('Origin',(-3.,-1.44337567297407,2.5));
#66272=CARTESIAN_POINT('',(-3.,-1.44337567297407,2.5));
#66273=CARTESIAN_POINT('',(-3.,-1.44337567297407,2.5));
#66274=CARTESIAN_POINT('',(-3.,-1.44337567297407,2.5));
#66275=CARTESIAN_POINT('Origin',(-3.,-2.88675134594813,-7.77133304087269E-16));
#66276=CARTESIAN_POINT('',(-3.,-2.88675134594813,-7.77133304087269E-16));
#66277=CARTESIAN_POINT('',(-3.,-2.88675134594813,-7.77133304087269E-16));
#66278=CARTESIAN_POINT('',(-3.,-2.88675134594813,-7.77133304087269E-16));
#66279=CARTESIAN_POINT('Origin',(-3.,-1.44337567297406,-2.5));
#66280=CARTESIAN_POINT('',(-3.,-1.44337567297406,-2.5));
#66281=CARTESIAN_POINT('',(-3.,-1.44337567297406,-2.5));
#66282=CARTESIAN_POINT('',(-3.,-1.44337567297406,-2.5));
#66283=CARTESIAN_POINT('Origin',(-3.,1.44337567297407,-2.5));
#66284=CARTESIAN_POINT('',(-3.,1.44337567297407,-2.5));
#66285=CARTESIAN_POINT('',(-3.,1.44337567297407,-2.5));
#66286=CARTESIAN_POINT('',(-3.,1.44337567297407,-2.5));
#66287=CARTESIAN_POINT('Origin',(-3.,2.88675134594813,3.50584097974525E-17));
#66288=CARTESIAN_POINT('',(-3.,2.88675134594813,3.50584097974525E-17));
#66289=CARTESIAN_POINT('Origin',(-3.,3.67394039744206E-16,0.));
#66290=CARTESIAN_POINT('',(0.,0.,0.));
#66291=CARTESIAN_POINT('Origin',(-7.3,0.,0.));
#66292=CARTESIAN_POINT('',(-6.79999999999999,5.20474889637625E-16,-4.25));
#66293=CARTESIAN_POINT('',(-6.79999999999999,-5.20474889637625E-16,4.25));
#66294=CARTESIAN_POINT('Origin',(-6.79999999999999,0.,0.));
#66295=CARTESIAN_POINT('Origin',(-6.79999999999999,0.,0.));
#66296=CARTESIAN_POINT('',(-7.3,-4.59242549680257E-16,3.75));
#66297=CARTESIAN_POINT('',(-7.3,-4.59242549680257E-16,3.75));
#66298=CARTESIAN_POINT('Origin',(-7.3,0.,0.));
#66299=CARTESIAN_POINT('Origin',(-1003.59827876194,5.22934144793585E-14,
0.));
#66300=CARTESIAN_POINT('',(-3.59827876194487,-1.94294868429572E-16,0.));
#66301=CARTESIAN_POINT('',(-4.80000000000004,2.00000000000045,-2.44929359829514E-16));
#66302=CARTESIAN_POINT('',(-1003.59827876194,1664.2794823505,-2.03815454094715E-13));
#66303=CARTESIAN_POINT('',(-4.8,1.73205080756888,-1.));
#66304=CARTESIAN_POINT('Origin',(-4.8,-1.3121927336947E-16,0.));
#66305=CARTESIAN_POINT('',(-4.8,-1.3121927336947E-16,-2.));
#66306=CARTESIAN_POINT('Origin',(-4.8,-1.3121927336947E-16,0.));
#66307=CARTESIAN_POINT('',(-4.8,-1.73205080756888,-1.));
#66308=CARTESIAN_POINT('Origin',(-4.8,-1.3121927336947E-16,0.));
#66309=CARTESIAN_POINT('',(-4.8,-1.73205080756888,1.));
#66310=CARTESIAN_POINT('Origin',(-4.8,-1.3121927336947E-16,0.));
#66311=CARTESIAN_POINT('',(-4.8,2.4435937631482E-16,2.));
#66312=CARTESIAN_POINT('Origin',(-4.8,-1.3121927336947E-16,0.));
#66313=CARTESIAN_POINT('',(-4.8,1.73205080756888,0.999999999999999));
#66314=CARTESIAN_POINT('Origin',(-4.8,-1.3121927336947E-16,0.));
#66315=CARTESIAN_POINT('Origin',(-4.8,-1.3121927336947E-16,0.));
#66316=CARTESIAN_POINT('Origin',(-7.3,0.,0.));
#66317=CARTESIAN_POINT('',(-2.3,-5.20474889637625E-16,-4.25));
#66318=CARTESIAN_POINT('',(-7.3,-5.20474889637625E-16,-4.25));
#66319=CARTESIAN_POINT('Origin',(-2.3,0.,0.));
#66320=CARTESIAN_POINT('Origin',(-7.3,0.,0.));
#66321=CARTESIAN_POINT('',(-2.3,-2.52889564023928E-16,-2.065));
#66322=CARTESIAN_POINT('Origin',(-2.3,0.,0.));
#66323=CARTESIAN_POINT('',(2.85,-2.52889564023928E-16,-2.065));
#66324=CARTESIAN_POINT('',(-7.3,-2.52889564023928E-16,-2.065));
#66325=CARTESIAN_POINT('Origin',(2.85,0.,0.));
#66326=CARTESIAN_POINT('Origin',(-7.3,0.,0.));
#66327=CARTESIAN_POINT('',(2.85,-3.67394039744206E-16,-3.));
#66328=CARTESIAN_POINT('Origin',(2.85,0.,0.));
#66329=CARTESIAN_POINT('',(22.7,-3.67394039744206E-16,-3.));
#66330=CARTESIAN_POINT('',(-7.3,-3.67394039744206E-16,-3.));
#66331=CARTESIAN_POINT('Origin',(22.7,0.,0.));
#66332=CARTESIAN_POINT('Origin',(-7.3,0.,0.));
#66333=CARTESIAN_POINT('',(-7.3,1.15470053837925,2.));
#66334=CARTESIAN_POINT('',(-7.3,2.3094010767585,1.33236321473148E-16));
#66335=CARTESIAN_POINT('',(-7.3,1.15470053837925,2.));
#66336=CARTESIAN_POINT('',(-7.3,-1.15470053837925,2.));
#66337=CARTESIAN_POINT('',(-7.3,-1.15470053837925,2.));
#66338=CARTESIAN_POINT('',(-7.3,-2.3094010767585,4.08864764769604E-16));
#66339=CARTESIAN_POINT('',(-7.3,-2.3094010767585,4.08864764769604E-16));
#66340=CARTESIAN_POINT('',(-7.3,-1.15470053837925,-2.));
#66341=CARTESIAN_POINT('',(-7.3,-1.15470053837925,-2.));
#66342=CARTESIAN_POINT('',(-7.3,1.15470053837925,-2.));
#66343=CARTESIAN_POINT('',(-7.3,1.15470053837925,-2.));
#66344=CARTESIAN_POINT('',(-7.3,2.3094010767585,1.33236321473148E-16));
#66345=CARTESIAN_POINT('Origin',(22.7,3.,0.));
#66346=CARTESIAN_POINT('Origin',(2.85,3.,0.));
#66347=CARTESIAN_POINT('Origin',(-2.3,2.065,0.));
#66348=CARTESIAN_POINT('Origin',(-4.8,-1.15470053837925,2.));
#66349=CARTESIAN_POINT('',(-4.8,-1.15470053837925,2.));
#66350=CARTESIAN_POINT('',(-4.8,-1.15470053837925,2.));
#66351=CARTESIAN_POINT('',(-4.8,-1.15470053837925,2.));
#66352=CARTESIAN_POINT('',(-4.8,1.15470053837925,2.));
#66353=CARTESIAN_POINT('',(-4.8,1.15470053837925,2.));
#66354=CARTESIAN_POINT('',(-4.8,-1.15470053837925,2.));
#66355=CARTESIAN_POINT('Origin',(-4.8,-2.3094010767585,4.08864764769604E-16));
#66356=CARTESIAN_POINT('',(-4.8,-2.3094010767585,4.08864764769604E-16));
#66357=CARTESIAN_POINT('',(-4.8,-2.3094010767585,4.08864764769604E-16));
#66358=CARTESIAN_POINT('',(-4.8,-2.3094010767585,4.08864764769604E-16));
#66359=CARTESIAN_POINT('',(-4.8,-2.3094010767585,4.08864764769604E-16));
#66360=CARTESIAN_POINT('Origin',(-4.8,-1.15470053837925,-2.));
#66361=CARTESIAN_POINT('',(-4.8,-1.15470053837925,-2.));
#66362=CARTESIAN_POINT('',(-4.8,-1.15470053837925,-2.));
#66363=CARTESIAN_POINT('',(-4.8,-1.15470053837925,-2.));
#66364=CARTESIAN_POINT('',(-4.8,-1.15470053837925,-2.));
#66365=CARTESIAN_POINT('Origin',(-4.8,1.15470053837925,-2.));
#66366=CARTESIAN_POINT('',(-4.8,1.15470053837925,-2.));
#66367=CARTESIAN_POINT('',(-4.8,1.15470053837925,-2.));
#66368=CARTESIAN_POINT('',(-4.8,1.15470053837925,-2.));
#66369=CARTESIAN_POINT('',(-4.8,1.15470053837925,-2.));
#66370=CARTESIAN_POINT('Origin',(-4.8,2.3094010767585,1.33236321473148E-16));
#66371=CARTESIAN_POINT('',(-4.8,2.3094010767585,1.33236321473148E-16));
#66372=CARTESIAN_POINT('',(-4.8,2.3094010767585,1.33236321473148E-16));
#66373=CARTESIAN_POINT('',(-4.8,2.3094010767585,1.33236321473148E-16));
#66374=CARTESIAN_POINT('',(-4.8,2.3094010767585,1.33236321473148E-16));
#66375=CARTESIAN_POINT('Origin',(-4.8,1.15470053837925,2.));
#66376=CARTESIAN_POINT('',(-4.8,1.15470053837925,2.));
#66377=CARTESIAN_POINT('',(-4.8,1.15470053837925,2.));
#66378=CARTESIAN_POINT('Origin',(-4.8,0.,0.));
#66379=CARTESIAN_POINT('Origin',(-4.8,0.,0.));
#66380=CARTESIAN_POINT('Origin',(-4.8,0.,0.));
#66381=CARTESIAN_POINT('Origin',(-4.8,0.,0.));
#66382=CARTESIAN_POINT('Origin',(-4.8,0.,0.));
#66383=CARTESIAN_POINT('Origin',(-4.8,0.,0.));
#66384=CARTESIAN_POINT('Origin',(-7.3,-2.80889253323697E-17,0.));
#66385=CARTESIAN_POINT('',(-1.,5.,-6.12323399573677E-16));
#66386=CARTESIAN_POINT('Origin',(-1.,-3.84779799073558E-18,0.));
#66387=CARTESIAN_POINT('',(0.,5.,-6.12323399573677E-16));
#66388=CARTESIAN_POINT('',(-7.3,5.,-6.12323399573677E-16));
#66389=CARTESIAN_POINT('Origin',(0.,0.,0.));
#66390=CARTESIAN_POINT('Origin',(-7.3,-2.80889253323697E-17,0.));
#66391=CARTESIAN_POINT('',(0.,2.5,-3.06161699786838E-16));
#66392=CARTESIAN_POINT('Origin',(0.,0.,0.));
#66393=CARTESIAN_POINT('',(-1.,2.5,-3.06161699786838E-16));
#66394=CARTESIAN_POINT('',(-7.3,2.5,-3.06161699786838E-16));
#66395=CARTESIAN_POINT('Origin',(-1.,-3.84779799073558E-18,0.));
#66396=CARTESIAN_POINT('Origin',(-1.,5.,0.));
#66397=CARTESIAN_POINT('Origin',(-3.54259174671033E-17,5.,0.));
#66398=CARTESIAN_POINT('Origin',(-2.3,-2.80889253323697E-17,0.));
#66399=CARTESIAN_POINT('',(-1.,1.065,4.11439849795812));
#66400=CARTESIAN_POINT('',(-1.,-1.065,4.11439849795812));
#66401=CARTESIAN_POINT('Origin',(-1.,-1.22125762314651E-17,0.));
#66402=CARTESIAN_POINT('',(-2.3,-1.065,4.11439849795812));
#66403=CARTESIAN_POINT('',(-2.3,-1.065,4.11439849795812));
#66404=CARTESIAN_POINT('',(-2.3,1.065,4.11439849795812));
#66405=CARTESIAN_POINT('Origin',(-2.3,-2.80889253323697E-17,0.));
#66406=CARTESIAN_POINT('',(-2.3,1.065,4.11439849795812));
#66407=CARTESIAN_POINT('Origin',(-2.3,-2.80889253323697E-17,0.));
#66408=CARTESIAN_POINT('',(-1.,1.065,2.26180790519443));
#66409=CARTESIAN_POINT('',(-1.,-1.065,2.26180790519443));
#66410=CARTESIAN_POINT('Origin',(-1.,-1.22125762314651E-17,0.));
#66411=CARTESIAN_POINT('',(-2.3,1.065,2.26180790519443));
#66412=CARTESIAN_POINT('',(-2.3,1.065,2.26180790519443));
#66413=CARTESIAN_POINT('',(-2.3,-1.065,2.26180790519443));
#66414=CARTESIAN_POINT('Origin',(-2.3,-2.80889253323697E-17,0.));
#66415=CARTESIAN_POINT('',(-2.3,-1.065,2.26180790519443));
#66416=CARTESIAN_POINT('Origin',(-2.3,4.25,0.));
#66417=CARTESIAN_POINT('',(-2.3,-1.065,4.11439849795812));
#66418=CARTESIAN_POINT('',(-2.3,1.065,4.11439849795812));
#66419=CARTESIAN_POINT('Origin',(-1.,4.25,0.));
#66420=CARTESIAN_POINT('',(-1.,-1.065,4.11439849795812));
#66421=CARTESIAN_POINT('',(-1.,1.065,4.11439849795812));
#66422=CARTESIAN_POINT('Origin',(-2.3,1.065,4.11439849795812));
#66423=CARTESIAN_POINT('Origin',(-2.3,-1.065,4.11439849795812));
#66424=CARTESIAN_POINT('',(0.,0.,0.));
#66425=CARTESIAN_POINT('Origin',(0.,-60.,8.));
#66426=CARTESIAN_POINT('',(-4.,-60.,0.));
#66427=CARTESIAN_POINT('Origin',(0.,-60.,0.));
#66428=CARTESIAN_POINT('',(-4.,-60.,8.));
#66429=CARTESIAN_POINT('',(-4.,-60.,8.));
#66430=CARTESIAN_POINT('Origin',(0.,-60.,8.));
#66431=CARTESIAN_POINT('Origin',(0.,60.,8.));
#66432=CARTESIAN_POINT('',(-4.,60.,0.));
#66433=CARTESIAN_POINT('Origin',(0.,60.,0.));
#66434=CARTESIAN_POINT('',(-4.,60.,8.));
#66435=CARTESIAN_POINT('',(-4.,60.,8.));
#66436=CARTESIAN_POINT('Origin',(0.,60.,8.));
#66437=CARTESIAN_POINT('Origin',(-30.5,-108.5,8.));
#66438=CARTESIAN_POINT('',(-33.75,-108.5,0.));
#66439=CARTESIAN_POINT('Origin',(-30.5,-108.5,0.));
#66440=CARTESIAN_POINT('',(-33.75,-108.5,8.));
#66441=CARTESIAN_POINT('',(-33.75,-108.5,8.));
#66442=CARTESIAN_POINT('Origin',(-30.5,-108.5,8.));
#66443=CARTESIAN_POINT('Origin',(-30.5,-63.5,8.));
#66444=CARTESIAN_POINT('',(-33.75,-63.5,0.));
#66445=CARTESIAN_POINT('Origin',(-30.5,-63.5,0.));
#66446=CARTESIAN_POINT('',(-33.75,-63.5,8.));
#66447=CARTESIAN_POINT('',(-33.75,-63.5,8.));
#66448=CARTESIAN_POINT('Origin',(-30.5,-63.5,8.));
#66449=CARTESIAN_POINT('Origin',(26.5,-108.5,8.));
#66450=CARTESIAN_POINT('',(23.25,-108.5,0.));
#66451=CARTESIAN_POINT('Origin',(26.5,-108.5,0.));
#66452=CARTESIAN_POINT('',(23.25,-108.5,8.));
#66453=CARTESIAN_POINT('',(23.25,-108.5,8.));
#66454=CARTESIAN_POINT('Origin',(26.5,-108.5,8.));
#66455=CARTESIAN_POINT('Origin',(26.5,-63.5,8.));
#66456=CARTESIAN_POINT('',(23.25,-63.5,0.));
#66457=CARTESIAN_POINT('Origin',(26.5,-63.5,0.));
#66458=CARTESIAN_POINT('',(23.25,-63.5,8.));
#66459=CARTESIAN_POINT('',(23.25,-63.5,8.));
#66460=CARTESIAN_POINT('Origin',(26.5,-63.5,8.));
#66461=CARTESIAN_POINT('Origin',(-30.5,63.5,8.));
#66462=CARTESIAN_POINT('',(-33.75,63.5,0.));
#66463=CARTESIAN_POINT('Origin',(-30.5,63.5,0.));
#66464=CARTESIAN_POINT('',(-33.75,63.5,8.));
#66465=CARTESIAN_POINT('',(-33.75,63.5,8.));
#66466=CARTESIAN_POINT('Origin',(-30.5,63.5,8.));
#66467=CARTESIAN_POINT('Origin',(-30.5,108.5,8.));
#66468=CARTESIAN_POINT('',(-33.75,108.5,0.));
#66469=CARTESIAN_POINT('Origin',(-30.5,108.5,0.));
#66470=CARTESIAN_POINT('',(-33.75,108.5,8.));
#66471=CARTESIAN_POINT('',(-33.75,108.5,8.));
#66472=CARTESIAN_POINT('Origin',(-30.5,108.5,8.));
#66473=CARTESIAN_POINT('Origin',(26.5,63.5,8.));
#66474=CARTESIAN_POINT('',(23.25,63.5,0.));
#66475=CARTESIAN_POINT('Origin',(26.5,63.5,0.));
#66476=CARTESIAN_POINT('',(23.25,63.5,8.));
#66477=CARTESIAN_POINT('',(23.25,63.5,8.));
#66478=CARTESIAN_POINT('Origin',(26.5,63.5,8.));
#66479=CARTESIAN_POINT('Origin',(26.5,108.5,8.));
#66480=CARTESIAN_POINT('',(23.25,108.5,0.));
#66481=CARTESIAN_POINT('Origin',(26.5,108.5,0.));
#66482=CARTESIAN_POINT('',(23.25,108.5,8.));
#66483=CARTESIAN_POINT('',(23.25,108.5,8.));
#66484=CARTESIAN_POINT('Origin',(26.5,108.5,8.));
#66485=CARTESIAN_POINT('Origin',(0.,0.,0.));
#66486=CARTESIAN_POINT('',(-37.,140.,0.));
#66487=CARTESIAN_POINT('',(-37.,-140.,0.));
#66488=CARTESIAN_POINT('',(-37.,151.313708498985,0.));
#66489=CARTESIAN_POINT('',(45.,140.,0.));
#66490=CARTESIAN_POINT('',(-45.,140.,0.));
#66491=CARTESIAN_POINT('',(45.,-140.,0.));
#66492=CARTESIAN_POINT('',(45.,140.,0.));
#66493=CARTESIAN_POINT('',(-45.,-140.,0.));
#66494=CARTESIAN_POINT('Origin',(45.,140.,8.));
#66495=CARTESIAN_POINT('',(45.,140.,8.));
#66496=CARTESIAN_POINT('',(45.,140.,8.));
#66497=CARTESIAN_POINT('',(45.,-140.,8.));
#66498=CARTESIAN_POINT('',(45.,140.,8.));
#66499=CARTESIAN_POINT('',(45.,-140.,8.));
#66500=CARTESIAN_POINT('Origin',(-45.,140.,8.));
#66501=CARTESIAN_POINT('',(-37.,140.,-8.));
#66502=CARTESIAN_POINT('',(-37.,140.,0.));
#66503=CARTESIAN_POINT('',(-45.,140.,-8.));
#66504=CARTESIAN_POINT('',(-45.,140.,-8.));
#66505=CARTESIAN_POINT('',(-45.,140.,8.));
#66506=CARTESIAN_POINT('',(-45.,140.,8.));
#66507=CARTESIAN_POINT('',(-45.,140.,8.));
#66508=CARTESIAN_POINT('Origin',(-45.,140.,8.));
#66509=CARTESIAN_POINT('',(-45.,-140.,-8.));
#66510=CARTESIAN_POINT('',(-45.,151.313708498985,-8.));
#66511=CARTESIAN_POINT('',(-45.,-140.,8.));
#66512=CARTESIAN_POINT('',(-45.,-140.,8.));
#66513=CARTESIAN_POINT('',(-45.,140.,8.));
#66514=CARTESIAN_POINT('Origin',(-45.,-140.,8.));
#66515=CARTESIAN_POINT('',(-37.,-140.,-8.));
#66516=CARTESIAN_POINT('',(-45.,-140.,-8.));
#66517=CARTESIAN_POINT('',(-37.,-140.,0.));
#66518=CARTESIAN_POINT('',(-45.,-140.,8.));
#66519=CARTESIAN_POINT('Origin',(0.,0.,8.));
#66520=CARTESIAN_POINT('Origin',(-37.,151.313708498985,0.));
#66521=CARTESIAN_POINT('',(-37.,151.313708498985,-8.));
#66522=CARTESIAN_POINT('Origin',(-45.,151.313708498985,-8.));
#66523=CARTESIAN_POINT('',(0.,0.,0.));
#66524=CARTESIAN_POINT('Origin',(25.,2.32682891837997E-15,0.));
#66525=CARTESIAN_POINT('',(0.,-5.,-6.12323399573677E-16));
#66526=CARTESIAN_POINT('Origin',(0.,-7.34788079488413E-16,0.));
#66527=CARTESIAN_POINT('',(-5.4,-5.,-6.12323399573677E-16));
#66528=CARTESIAN_POINT('',(25.,-5.,-6.12323399573677E-16));
#66529=CARTESIAN_POINT('Origin',(-5.4,-1.39609735102798E-15,0.));
#66530=CARTESIAN_POINT('Origin',(-5.4,-1.39609735102798E-15,0.));
#66531=CARTESIAN_POINT('',(-6.,-4.4,-5.38844591624836E-16));
#66532=CARTESIAN_POINT('',(-5.4,-5.,-6.12323399573677E-16));
#66533=CARTESIAN_POINT('Origin',(-6.,-1.46957615897682E-15,0.));
#66534=CARTESIAN_POINT('Origin',(25.,2.32682891837997E-15,0.));
#66535=CARTESIAN_POINT('',(24.4585,-3.,3.67394039744206E-16));
#66536=CARTESIAN_POINT('',(24.4585,3.,-3.67394039744206E-16));
#66537=CARTESIAN_POINT('Origin',(24.4585,2.26051429420614E-15,0.));
#66538=CARTESIAN_POINT('',(25.,2.4585,-3.01079415570377E-16));
#66539=CARTESIAN_POINT('',(25.,2.4585,-3.01079415570377E-16));
#66540=CARTESIAN_POINT('Origin',(25.,2.32682891837997E-15,0.));
#66541=CARTESIAN_POINT('Origin',(24.4585,2.26051429420614E-15,0.));
#66542=CARTESIAN_POINT('Origin',(25.,2.32682891837997E-15,0.));
#66543=CARTESIAN_POINT('',(0.,-3.,-3.67394039744206E-16));
#66544=CARTESIAN_POINT('',(25.,-3.,-3.67394039744206E-16));
#66545=CARTESIAN_POINT('Origin',(0.,-7.34788079488413E-16,0.));
#66546=CARTESIAN_POINT('Origin',(25.,2.4585,0.));
#66547=CARTESIAN_POINT('Origin',(-6.,-1.46957615897682E-15,0.));
#66548=CARTESIAN_POINT('',(-6.,1.44337567297406,2.5));
#66549=CARTESIAN_POINT('',(-6.,2.88675134594813,0.));
#66550=CARTESIAN_POINT('',(-6.,1.44337567297406,2.5));
#66551=CARTESIAN_POINT('',(-6.,-1.44337567297407,2.5));
#66552=CARTESIAN_POINT('',(-6.,-1.44337567297407,2.5));
#66553=CARTESIAN_POINT('',(-6.,-2.88675134594813,-7.77133304087269E-16));
#66554=CARTESIAN_POINT('',(-6.,-2.88675134594813,-7.77133304087269E-16));
#66555=CARTESIAN_POINT('',(-6.,-1.44337567297407,-2.5));
#66556=CARTESIAN_POINT('',(-6.,-1.44337567297407,-2.5));
#66557=CARTESIAN_POINT('',(-6.,1.44337567297406,-2.5));
#66558=CARTESIAN_POINT('',(-6.,1.44337567297406,-2.5));
#66559=CARTESIAN_POINT('',(-6.,2.88675134594813,3.50584097974525E-17));
#66560=CARTESIAN_POINT('Origin',(1.22464679914735E-16,3.,0.));
#66561=CARTESIAN_POINT('Origin',(-3.,1.44337567297406,2.5));
#66562=CARTESIAN_POINT('',(-3.,2.88675134594813,3.50584097974525E-17));
#66563=CARTESIAN_POINT('',(-3.,2.88675134594813,3.50584097974525E-17));
#66564=CARTESIAN_POINT('',(-3.,1.44337567297406,2.5));
#66565=CARTESIAN_POINT('',(-3.,1.44337567297406,2.5));
#66566=CARTESIAN_POINT('',(-3.,1.44337567297406,2.5));
#66567=CARTESIAN_POINT('Origin',(-3.,-1.44337567297407,2.5));
#66568=CARTESIAN_POINT('',(-3.,-1.44337567297407,2.5));
#66569=CARTESIAN_POINT('',(-3.,-1.44337567297407,2.5));
#66570=CARTESIAN_POINT('',(-3.,-1.44337567297407,2.5));
#66571=CARTESIAN_POINT('Origin',(-3.,-2.88675134594813,-7.77133304087269E-16));
#66572=CARTESIAN_POINT('',(-3.,-2.88675134594813,-7.77133304087269E-16));
#66573=CARTESIAN_POINT('',(-3.,-2.88675134594813,-7.77133304087269E-16));
#66574=CARTESIAN_POINT('',(-3.,-2.88675134594813,-7.77133304087269E-16));
#66575=CARTESIAN_POINT('Origin',(-3.,-1.44337567297406,-2.5));
#66576=CARTESIAN_POINT('',(-3.,-1.44337567297406,-2.5));
#66577=CARTESIAN_POINT('',(-3.,-1.44337567297406,-2.5));
#66578=CARTESIAN_POINT('',(-3.,-1.44337567297406,-2.5));
#66579=CARTESIAN_POINT('Origin',(-3.,1.44337567297407,-2.5));
#66580=CARTESIAN_POINT('',(-3.,1.44337567297407,-2.5));
#66581=CARTESIAN_POINT('',(-3.,1.44337567297407,-2.5));
#66582=CARTESIAN_POINT('',(-3.,1.44337567297407,-2.5));
#66583=CARTESIAN_POINT('Origin',(-3.,2.88675134594813,3.50584097974525E-17));
#66584=CARTESIAN_POINT('',(-3.,2.88675134594813,3.50584097974525E-17));
#66585=CARTESIAN_POINT('Origin',(-3.,3.67394039744206E-16,0.));
#66586=CARTESIAN_POINT('',(0.,0.,0.));
#66587=CARTESIAN_POINT('',(122.5,-34.0000000000004,1.40512601554121E-13));
#66588=CARTESIAN_POINT('',(122.5,-58.5,420.));
#66589=CARTESIAN_POINT('',(1.00000000000024,-11.5,-365.25));
#66590=CARTESIAN_POINT('',(5.62582244889689E-13,-38.0000000000003,550.));
#66591=CARTESIAN_POINT('',(-9.35331661127613E-14,-50.5,95.1444544197237));
#66592=CARTESIAN_POINT('',(-8.53598572143175E-14,-95.0000000000001,95.1444544197237));
#66593=CARTESIAN_POINT('',(-122.5,-58.5,420.));
#66594=CARTESIAN_POINT('',(16.6170093578837,-23.8829906421161,112.144454419724));
#66595=CARTESIAN_POINT('',(-122.5,-71.5,-240.));
#66596=CARTESIAN_POINT('',(-3.29253317792477E-13,-40.5,-373.));
#66597=CARTESIAN_POINT('',(2.49470960878785E-13,-12.5,-374.75));
#66598=CARTESIAN_POINT('',(6.30047885637073E-13,-12.5,417.));
#66599=CARTESIAN_POINT('',(12.0000000000006,-11.,437.));
#66600=CARTESIAN_POINT('',(4.17141435587613E-13,-40.5,501.));
#66601=CARTESIAN_POINT('',(124.5,-94.5,95.1444544197237));
#66602=CARTESIAN_POINT('',(24.0000000000006,-3.00000000000026,548.6));
#66603=CARTESIAN_POINT('',(-122.5,-34.0000000000004,1.11022302462516E-13));
#66604=CARTESIAN_POINT('',(23.4999999999999,-40.5,112.144454419724));
#66605=CARTESIAN_POINT('',(16.6170093578837,-57.1170093578839,112.144454419724));
#66606=CARTESIAN_POINT('',(122.5,-71.5,-240.));
#66607=CARTESIAN_POINT('',(-122.5,-71.5,-180.));
#66608=CARTESIAN_POINT('',(122.5,-71.5,-180.));
#66609=CARTESIAN_POINT('',(-122.5,-71.5,-120.));
#66610=CARTESIAN_POINT('',(122.5,-71.5,-120.));
#66611=CARTESIAN_POINT('',(-122.5,-71.5,-60.));
#66612=CARTESIAN_POINT('',(122.5,-71.5,-60.));
#66613=CARTESIAN_POINT('',(-122.5,-71.5,0.));
#66614=CARTESIAN_POINT('',(122.5,-71.5,0.));
#66615=CARTESIAN_POINT('',(-122.5,-71.5,60.));
#66616=CARTESIAN_POINT('',(122.5,-71.5,60.));
#66617=CARTESIAN_POINT('',(-122.5,-71.5,120.));
#66618=CARTESIAN_POINT('',(122.5,-71.5,120.));
#66619=CARTESIAN_POINT('',(-122.5,-71.5,180.));
#66620=CARTESIAN_POINT('',(122.5,-71.5,180.));
#66621=CARTESIAN_POINT('',(-122.5,-71.5,240.));
#66622=CARTESIAN_POINT('',(122.5,-71.5,240.));
#66623=CARTESIAN_POINT('',(-122.5,-71.5,300.));
#66624=CARTESIAN_POINT('',(122.5,-71.5,300.));
#66625=CARTESIAN_POINT('',(-122.5,-71.5,360.));
#66626=CARTESIAN_POINT('',(122.5,-71.5,360.));
#66627=CARTESIAN_POINT('',(-122.5,-71.5,420.));
#66628=CARTESIAN_POINT('',(-23.9999999999994,-3.00000000000026,548.6));
#66629=CARTESIAN_POINT('',(-16.6170093578839,-23.8829906421161,112.144454419724));
#66630=CARTESIAN_POINT('',(-23.5000000000001,-40.5,112.144454419724));
#66631=CARTESIAN_POINT('',(-16.6170093578839,-57.1170093578839,112.144454419724));
#66632=CARTESIAN_POINT('',(122.5,-71.5,420.));
#66633=CARTESIAN_POINT('',(-124.5,-94.5,95.1444544197237));
#66634=CARTESIAN_POINT('',(122.5,-71.5,-300.));
#66635=CARTESIAN_POINT('',(-122.5,-71.5,-300.));
#66636=CARTESIAN_POINT('',(122.5,-71.5,-360.));
#66637=CARTESIAN_POINT('',(-122.5,-71.5,-360.));
#66638=CARTESIAN_POINT('',(122.5,-71.5,-420.));
#66639=CARTESIAN_POINT('',(-122.5,-71.5,-420.));
#66640=UNCERTAINTY_MEASURE_WITH_UNIT(LENGTH_MEASURE(0.01),#66722,
'DISTANCE_ACCURACY_VALUE',
'Maximum model space distance between geometric entities at asserted c
onnectivities');
#66641=UNCERTAINTY_MEASURE_WITH_UNIT(LENGTH_MEASURE(0.01),#66722,
'DISTANCE_ACCURACY_VALUE',
'Maximum model space distance between geometric entities at asserted c
onnectivities');
#66642=UNCERTAINTY_MEASURE_WITH_UNIT(LENGTH_MEASURE(0.01),#66722,
'DISTANCE_ACCURACY_VALUE',
'Maximum model space distance between geometric entities at asserted c
onnectivities');
#66643=UNCERTAINTY_MEASURE_WITH_UNIT(LENGTH_MEASURE(0.01),#66722,
'DISTANCE_ACCURACY_VALUE',
'Maximum model space distance between geometric entities at asserted c
onnectivities');
#66644=UNCERTAINTY_MEASURE_WITH_UNIT(LENGTH_MEASURE(0.01),#66722,
'DISTANCE_ACCURACY_VALUE',
'Maximum model space distance between geometric entities at asserted c
onnectivities');
#66645=UNCERTAINTY_MEASURE_WITH_UNIT(LENGTH_MEASURE(0.01),#66722,
'DISTANCE_ACCURACY_VALUE',
'Maximum model space distance between geometric entities at asserted c
onnectivities');
#66646=UNCERTAINTY_MEASURE_WITH_UNIT(LENGTH_MEASURE(0.01),#66722,
'DISTANCE_ACCURACY_VALUE',
'Maximum model space distance between geometric entities at asserted c
onnectivities');
#66647=UNCERTAINTY_MEASURE_WITH_UNIT(LENGTH_MEASURE(0.01),#66722,
'DISTANCE_ACCURACY_VALUE',
'Maximum model space distance between geometric entities at asserted c
onnectivities');
#66648=UNCERTAINTY_MEASURE_WITH_UNIT(LENGTH_MEASURE(0.01),#66722,
'DISTANCE_ACCURACY_VALUE',
'Maximum model space distance between geometric entities at asserted c
onnectivities');
#66649=UNCERTAINTY_MEASURE_WITH_UNIT(LENGTH_MEASURE(0.01),#66722,
'DISTANCE_ACCURACY_VALUE',
'Maximum model space distance between geometric entities at asserted c
onnectivities');
#66650=UNCERTAINTY_MEASURE_WITH_UNIT(LENGTH_MEASURE(0.01),#66722,
'DISTANCE_ACCURACY_VALUE',
'Maximum model space distance between geometric entities at asserted c
onnectivities');
#66651=UNCERTAINTY_MEASURE_WITH_UNIT(LENGTH_MEASURE(0.01),#66722,
'DISTANCE_ACCURACY_VALUE',
'Maximum model space distance between geometric entities at asserted c
onnectivities');
#66652=UNCERTAINTY_MEASURE_WITH_UNIT(LENGTH_MEASURE(0.01),#66722,
'DISTANCE_ACCURACY_VALUE',
'Maximum model space distance between geometric entities at asserted c
onnectivities');
#66653=UNCERTAINTY_MEASURE_WITH_UNIT(LENGTH_MEASURE(0.01),#66722,
'DISTANCE_ACCURACY_VALUE',
'Maximum model space distance between geometric entities at asserted c
onnectivities');
#66654=UNCERTAINTY_MEASURE_WITH_UNIT(LENGTH_MEASURE(0.01),#66722,
'DISTANCE_ACCURACY_VALUE',
'Maximum model space distance between geometric entities at asserted c
onnectivities');
#66655=UNCERTAINTY_MEASURE_WITH_UNIT(LENGTH_MEASURE(0.01),#66722,
'DISTANCE_ACCURACY_VALUE',
'Maximum model space distance between geometric entities at asserted c
onnectivities');
#66656=UNCERTAINTY_MEASURE_WITH_UNIT(LENGTH_MEASURE(0.01),#66722,
'DISTANCE_ACCURACY_VALUE',
'Maximum model space distance between geometric entities at asserted c
onnectivities');
#66657=UNCERTAINTY_MEASURE_WITH_UNIT(LENGTH_MEASURE(0.01),#66722,
'DISTANCE_ACCURACY_VALUE',
'Maximum model space distance between geometric entities at asserted c
onnectivities');
#66658=UNCERTAINTY_MEASURE_WITH_UNIT(LENGTH_MEASURE(0.01),#66722,
'DISTANCE_ACCURACY_VALUE',
'Maximum model space distance between geometric entities at asserted c
onnectivities');
#66659=UNCERTAINTY_MEASURE_WITH_UNIT(LENGTH_MEASURE(0.01),#66722,
'DISTANCE_ACCURACY_VALUE',
'Maximum model space distance between geometric entities at asserted c
onnectivities');
#66660=UNCERTAINTY_MEASURE_WITH_UNIT(LENGTH_MEASURE(0.01),#66722,
'DISTANCE_ACCURACY_VALUE',
'Maximum model space distance between geometric entities at asserted c
onnectivities');
#66661=UNCERTAINTY_MEASURE_WITH_UNIT(LENGTH_MEASURE(0.01),#66722,
'DISTANCE_ACCURACY_VALUE',
'Maximum model space distance between geometric entities at asserted c
onnectivities');
#66662=UNCERTAINTY_MEASURE_WITH_UNIT(LENGTH_MEASURE(0.01),#66722,
'DISTANCE_ACCURACY_VALUE',
'Maximum model space distance between geometric entities at asserted c
onnectivities');
#66663=UNCERTAINTY_MEASURE_WITH_UNIT(LENGTH_MEASURE(0.01),#66722,
'DISTANCE_ACCURACY_VALUE',
'Maximum model space distance between geometric entities at asserted c
onnectivities');
#66664=UNCERTAINTY_MEASURE_WITH_UNIT(LENGTH_MEASURE(0.01),#66722,
'DISTANCE_ACCURACY_VALUE',
'Maximum model space distance between geometric entities at asserted c
onnectivities');
#66665=UNCERTAINTY_MEASURE_WITH_UNIT(LENGTH_MEASURE(0.01),#66722,
'DISTANCE_ACCURACY_VALUE',
'Maximum model space distance between geometric entities at asserted c
onnectivities');
#66666=UNCERTAINTY_MEASURE_WITH_UNIT(LENGTH_MEASURE(0.01),#66722,
'DISTANCE_ACCURACY_VALUE',
'Maximum model space distance between geometric entities at asserted c
onnectivities');
#66667=UNCERTAINTY_MEASURE_WITH_UNIT(LENGTH_MEASURE(0.01),#66722,
'DISTANCE_ACCURACY_VALUE',
'Maximum model space distance between geometric entities at asserted c
onnectivities');
#66668=UNCERTAINTY_MEASURE_WITH_UNIT(LENGTH_MEASURE(0.01),#66722,
'DISTANCE_ACCURACY_VALUE',
'Maximum model space distance between geometric entities at asserted c
onnectivities');
#66669=UNCERTAINTY_MEASURE_WITH_UNIT(LENGTH_MEASURE(0.01),#66722,
'DISTANCE_ACCURACY_VALUE',
'Maximum model space distance between geometric entities at asserted c
onnectivities');
#66670=UNCERTAINTY_MEASURE_WITH_UNIT(LENGTH_MEASURE(0.01),#66722,
'DISTANCE_ACCURACY_VALUE',
'Maximum model space distance between geometric entities at asserted c
onnectivities');
#66671=UNCERTAINTY_MEASURE_WITH_UNIT(LENGTH_MEASURE(0.01),#66722,
'DISTANCE_ACCURACY_VALUE',
'Maximum model space distance between geometric entities at asserted c
onnectivities');
#66672=UNCERTAINTY_MEASURE_WITH_UNIT(LENGTH_MEASURE(0.01),#66722,
'DISTANCE_ACCURACY_VALUE',
'Maximum model space distance between geometric entities at asserted c
onnectivities');
#66673=UNCERTAINTY_MEASURE_WITH_UNIT(LENGTH_MEASURE(0.01),#66722,
'DISTANCE_ACCURACY_VALUE',
'Maximum model space distance between geometric entities at asserted c
onnectivities');
#66674=UNCERTAINTY_MEASURE_WITH_UNIT(LENGTH_MEASURE(0.01),#66722,
'DISTANCE_ACCURACY_VALUE',
'Maximum model space distance between geometric entities at asserted c
onnectivities');
#66675=UNCERTAINTY_MEASURE_WITH_UNIT(LENGTH_MEASURE(0.01),#66722,
'DISTANCE_ACCURACY_VALUE',
'Maximum model space distance between geometric entities at asserted c
onnectivities');
#66676=UNCERTAINTY_MEASURE_WITH_UNIT(LENGTH_MEASURE(0.01),#66722,
'DISTANCE_ACCURACY_VALUE',
'Maximum model space distance between geometric entities at asserted c
onnectivities');
#66677=UNCERTAINTY_MEASURE_WITH_UNIT(LENGTH_MEASURE(0.01),#66722,
'DISTANCE_ACCURACY_VALUE',
'Maximum model space distance between geometric entities at asserted c
onnectivities');
#66678=UNCERTAINTY_MEASURE_WITH_UNIT(LENGTH_MEASURE(0.01),#66722,
'DISTANCE_ACCURACY_VALUE',
'Maximum model space distance between geometric entities at asserted c
onnectivities');
#66679=UNCERTAINTY_MEASURE_WITH_UNIT(LENGTH_MEASURE(0.01),#66722,
'DISTANCE_ACCURACY_VALUE',
'Maximum model space distance between geometric entities at asserted c
onnectivities');
#66680=UNCERTAINTY_MEASURE_WITH_UNIT(LENGTH_MEASURE(0.01),#66722,
'DISTANCE_ACCURACY_VALUE',
'Maximum model space distance between geometric entities at asserted c
onnectivities');
#66681=(
GEOMETRIC_REPRESENTATION_CONTEXT(3)
GLOBAL_UNCERTAINTY_ASSIGNED_CONTEXT((#66640))
GLOBAL_UNIT_ASSIGNED_CONTEXT((#66722,#66724,#66725))
REPRESENTATION_CONTEXT('','3D')
);
#66682=(
GEOMETRIC_REPRESENTATION_CONTEXT(3)
GLOBAL_UNCERTAINTY_ASSIGNED_CONTEXT((#66641))
GLOBAL_UNIT_ASSIGNED_CONTEXT((#66722,#66724,#66725))
REPRESENTATION_CONTEXT('','3D')
);
#66683=(
GEOMETRIC_REPRESENTATION_CONTEXT(3)
GLOBAL_UNCERTAINTY_ASSIGNED_CONTEXT((#66642))
GLOBAL_UNIT_ASSIGNED_CONTEXT((#66722,#66724,#66725))
REPRESENTATION_CONTEXT('','3D')
);
#66684=(
GEOMETRIC_REPRESENTATION_CONTEXT(3)
GLOBAL_UNCERTAINTY_ASSIGNED_CONTEXT((#66643))
GLOBAL_UNIT_ASSIGNED_CONTEXT((#66722,#66724,#66725))
REPRESENTATION_CONTEXT('','3D')
);
#66685=(
GEOMETRIC_REPRESENTATION_CONTEXT(3)
GLOBAL_UNCERTAINTY_ASSIGNED_CONTEXT((#66644))
GLOBAL_UNIT_ASSIGNED_CONTEXT((#66722,#66724,#66725))
REPRESENTATION_CONTEXT('','3D')
);
#66686=(
GEOMETRIC_REPRESENTATION_CONTEXT(3)
GLOBAL_UNCERTAINTY_ASSIGNED_CONTEXT((#66645))
GLOBAL_UNIT_ASSIGNED_CONTEXT((#66722,#66724,#66725))
REPRESENTATION_CONTEXT('','3D')
);
#66687=(
GEOMETRIC_REPRESENTATION_CONTEXT(3)
GLOBAL_UNCERTAINTY_ASSIGNED_CONTEXT((#66646))
GLOBAL_UNIT_ASSIGNED_CONTEXT((#66722,#66724,#66725))
REPRESENTATION_CONTEXT('','3D')
);
#66688=(
GEOMETRIC_REPRESENTATION_CONTEXT(3)
GLOBAL_UNCERTAINTY_ASSIGNED_CONTEXT((#66647))
GLOBAL_UNIT_ASSIGNED_CONTEXT((#66722,#66724,#66725))
REPRESENTATION_CONTEXT('','3D')
);
#66689=(
GEOMETRIC_REPRESENTATION_CONTEXT(3)
GLOBAL_UNCERTAINTY_ASSIGNED_CONTEXT((#66648))
GLOBAL_UNIT_ASSIGNED_CONTEXT((#66722,#66724,#66725))
REPRESENTATION_CONTEXT('','3D')
);
#66690=(
GEOMETRIC_REPRESENTATION_CONTEXT(3)
GLOBAL_UNCERTAINTY_ASSIGNED_CONTEXT((#66649))
GLOBAL_UNIT_ASSIGNED_CONTEXT((#66722,#66724,#66725))
REPRESENTATION_CONTEXT('','3D')
);
#66691=(
GEOMETRIC_REPRESENTATION_CONTEXT(3)
GLOBAL_UNCERTAINTY_ASSIGNED_CONTEXT((#66650))
GLOBAL_UNIT_ASSIGNED_CONTEXT((#66722,#66724,#66725))
REPRESENTATION_CONTEXT('','3D')
);
#66692=(
GEOMETRIC_REPRESENTATION_CONTEXT(3)
GLOBAL_UNCERTAINTY_ASSIGNED_CONTEXT((#66651))
GLOBAL_UNIT_ASSIGNED_CONTEXT((#66722,#66724,#66725))
REPRESENTATION_CONTEXT('','3D')
);
#66693=(
GEOMETRIC_REPRESENTATION_CONTEXT(3)
GLOBAL_UNCERTAINTY_ASSIGNED_CONTEXT((#66652))
GLOBAL_UNIT_ASSIGNED_CONTEXT((#66722,#66724,#66725))
REPRESENTATION_CONTEXT('','3D')
);
#66694=(
GEOMETRIC_REPRESENTATION_CONTEXT(3)
GLOBAL_UNCERTAINTY_ASSIGNED_CONTEXT((#66653))
GLOBAL_UNIT_ASSIGNED_CONTEXT((#66722,#66724,#66725))
REPRESENTATION_CONTEXT('','3D')
);
#66695=(
GEOMETRIC_REPRESENTATION_CONTEXT(3)
GLOBAL_UNCERTAINTY_ASSIGNED_CONTEXT((#66654))
GLOBAL_UNIT_ASSIGNED_CONTEXT((#66722,#66724,#66725))
REPRESENTATION_CONTEXT('','3D')
);
#66696=(
GEOMETRIC_REPRESENTATION_CONTEXT(3)
GLOBAL_UNCERTAINTY_ASSIGNED_CONTEXT((#66655))
GLOBAL_UNIT_ASSIGNED_CONTEXT((#66722,#66724,#66725))
REPRESENTATION_CONTEXT('','3D')
);
#66697=(
GEOMETRIC_REPRESENTATION_CONTEXT(3)
GLOBAL_UNCERTAINTY_ASSIGNED_CONTEXT((#66656))
GLOBAL_UNIT_ASSIGNED_CONTEXT((#66722,#66724,#66725))
REPRESENTATION_CONTEXT('','3D')
);
#66698=(
GEOMETRIC_REPRESENTATION_CONTEXT(3)
GLOBAL_UNCERTAINTY_ASSIGNED_CONTEXT((#66657))
GLOBAL_UNIT_ASSIGNED_CONTEXT((#66722,#66724,#66725))
REPRESENTATION_CONTEXT('','3D')
);
#66699=(
GEOMETRIC_REPRESENTATION_CONTEXT(3)
GLOBAL_UNCERTAINTY_ASSIGNED_CONTEXT((#66658))
GLOBAL_UNIT_ASSIGNED_CONTEXT((#66722,#66724,#66725))
REPRESENTATION_CONTEXT('','3D')
);
#66700=(
GEOMETRIC_REPRESENTATION_CONTEXT(3)
GLOBAL_UNCERTAINTY_ASSIGNED_CONTEXT((#66659))
GLOBAL_UNIT_ASSIGNED_CONTEXT((#66722,#66724,#66725))
REPRESENTATION_CONTEXT('','3D')
);
#66701=(
GEOMETRIC_REPRESENTATION_CONTEXT(3)
GLOBAL_UNCERTAINTY_ASSIGNED_CONTEXT((#66660))
GLOBAL_UNIT_ASSIGNED_CONTEXT((#66722,#66724,#66725))
REPRESENTATION_CONTEXT('','3D')
);
#66702=(
GEOMETRIC_REPRESENTATION_CONTEXT(3)
GLOBAL_UNCERTAINTY_ASSIGNED_CONTEXT((#66661))
GLOBAL_UNIT_ASSIGNED_CONTEXT((#66722,#66724,#66725))
REPRESENTATION_CONTEXT('','3D')
);
#66703=(
GEOMETRIC_REPRESENTATION_CONTEXT(3)
GLOBAL_UNCERTAINTY_ASSIGNED_CONTEXT((#66662))
GLOBAL_UNIT_ASSIGNED_CONTEXT((#66722,#66724,#66725))
REPRESENTATION_CONTEXT('','3D')
);
#66704=(
GEOMETRIC_REPRESENTATION_CONTEXT(3)
GLOBAL_UNCERTAINTY_ASSIGNED_CONTEXT((#66663))
GLOBAL_UNIT_ASSIGNED_CONTEXT((#66722,#66724,#66725))
REPRESENTATION_CONTEXT('','3D')
);
#66705=(
GEOMETRIC_REPRESENTATION_CONTEXT(3)
GLOBAL_UNCERTAINTY_ASSIGNED_CONTEXT((#66664))
GLOBAL_UNIT_ASSIGNED_CONTEXT((#66722,#66724,#66725))
REPRESENTATION_CONTEXT('','3D')
);
#66706=(
GEOMETRIC_REPRESENTATION_CONTEXT(3)
GLOBAL_UNCERTAINTY_ASSIGNED_CONTEXT((#66665))
GLOBAL_UNIT_ASSIGNED_CONTEXT((#66722,#66724,#66725))
REPRESENTATION_CONTEXT('','3D')
);
#66707=(
GEOMETRIC_REPRESENTATION_CONTEXT(3)
GLOBAL_UNCERTAINTY_ASSIGNED_CONTEXT((#66666))
GLOBAL_UNIT_ASSIGNED_CONTEXT((#66722,#66724,#66725))
REPRESENTATION_CONTEXT('','3D')
);
#66708=(
GEOMETRIC_REPRESENTATION_CONTEXT(3)
GLOBAL_UNCERTAINTY_ASSIGNED_CONTEXT((#66667))
GLOBAL_UNIT_ASSIGNED_CONTEXT((#66722,#66724,#66725))
REPRESENTATION_CONTEXT('','3D')
);
#66709=(
GEOMETRIC_REPRESENTATION_CONTEXT(3)
GLOBAL_UNCERTAINTY_ASSIGNED_CONTEXT((#66668))
GLOBAL_UNIT_ASSIGNED_CONTEXT((#66722,#66724,#66725))
REPRESENTATION_CONTEXT('','3D')
);
#66710=(
GEOMETRIC_REPRESENTATION_CONTEXT(3)
GLOBAL_UNCERTAINTY_ASSIGNED_CONTEXT((#66669))
GLOBAL_UNIT_ASSIGNED_CONTEXT((#66722,#66724,#66725))
REPRESENTATION_CONTEXT('','3D')
);
#66711=(
GEOMETRIC_REPRESENTATION_CONTEXT(3)
GLOBAL_UNCERTAINTY_ASSIGNED_CONTEXT((#66670))
GLOBAL_UNIT_ASSIGNED_CONTEXT((#66722,#66724,#66725))
REPRESENTATION_CONTEXT('','3D')
);
#66712=(
GEOMETRIC_REPRESENTATION_CONTEXT(3)
GLOBAL_UNCERTAINTY_ASSIGNED_CONTEXT((#66671))
GLOBAL_UNIT_ASSIGNED_CONTEXT((#66722,#66724,#66725))
REPRESENTATION_CONTEXT('','3D')
);
#66713=(
GEOMETRIC_REPRESENTATION_CONTEXT(3)
GLOBAL_UNCERTAINTY_ASSIGNED_CONTEXT((#66672))
GLOBAL_UNIT_ASSIGNED_CONTEXT((#66722,#66724,#66725))
REPRESENTATION_CONTEXT('','3D')
);
#66714=(
GEOMETRIC_REPRESENTATION_CONTEXT(3)
GLOBAL_UNCERTAINTY_ASSIGNED_CONTEXT((#66673))
GLOBAL_UNIT_ASSIGNED_CONTEXT((#66722,#66724,#66725))
REPRESENTATION_CONTEXT('','3D')
);
#66715=(
GEOMETRIC_REPRESENTATION_CONTEXT(3)
GLOBAL_UNCERTAINTY_ASSIGNED_CONTEXT((#66674))
GLOBAL_UNIT_ASSIGNED_CONTEXT((#66722,#66724,#66725))
REPRESENTATION_CONTEXT('','3D')
);
#66716=(
GEOMETRIC_REPRESENTATION_CONTEXT(3)
GLOBAL_UNCERTAINTY_ASSIGNED_CONTEXT((#66675))
GLOBAL_UNIT_ASSIGNED_CONTEXT((#66722,#66724,#66725))
REPRESENTATION_CONTEXT('','3D')
);
#66717=(
GEOMETRIC_REPRESENTATION_CONTEXT(3)
GLOBAL_UNCERTAINTY_ASSIGNED_CONTEXT((#66676))
GLOBAL_UNIT_ASSIGNED_CONTEXT((#66722,#66724,#66725))
REPRESENTATION_CONTEXT('','3D')
);
#66718=(
GEOMETRIC_REPRESENTATION_CONTEXT(3)
GLOBAL_UNCERTAINTY_ASSIGNED_CONTEXT((#66677))
GLOBAL_UNIT_ASSIGNED_CONTEXT((#66722,#66724,#66725))
REPRESENTATION_CONTEXT('','3D')
);
#66719=(
GEOMETRIC_REPRESENTATION_CONTEXT(3)
GLOBAL_UNCERTAINTY_ASSIGNED_CONTEXT((#66678))
GLOBAL_UNIT_ASSIGNED_CONTEXT((#66722,#66724,#66725))
REPRESENTATION_CONTEXT('','3D')
);
#66720=(
GEOMETRIC_REPRESENTATION_CONTEXT(3)
GLOBAL_UNCERTAINTY_ASSIGNED_CONTEXT((#66679))
GLOBAL_UNIT_ASSIGNED_CONTEXT((#66722,#66724,#66725))
REPRESENTATION_CONTEXT('','3D')
);
#66721=(
GEOMETRIC_REPRESENTATION_CONTEXT(3)
GLOBAL_UNCERTAINTY_ASSIGNED_CONTEXT((#66680))
GLOBAL_UNIT_ASSIGNED_CONTEXT((#66722,#66724,#66725))
REPRESENTATION_CONTEXT('','3D')
);
#66722=(
LENGTH_UNIT()
NAMED_UNIT(*)
SI_UNIT(.MILLI.,.METRE.)
);
#66723=(
LENGTH_UNIT()
NAMED_UNIT(*)
SI_UNIT($,.METRE.)
);
#66724=(
NAMED_UNIT(*)
PLANE_ANGLE_UNIT()
SI_UNIT($,.RADIAN.)
);
#66725=(
NAMED_UNIT(*)
SI_UNIT($,.STERADIAN.)
SOLID_ANGLE_UNIT()
);
#66726=SHAPE_DEFINITION_REPRESENTATION(#66766,#66890);
#66727=SHAPE_DEFINITION_REPRESENTATION(#66767,#66891);
#66728=SHAPE_DEFINITION_REPRESENTATION(#66768,#66892);
#66729=SHAPE_DEFINITION_REPRESENTATION(#66769,#66893);
#66730=SHAPE_DEFINITION_REPRESENTATION(#66770,#66894);
#66731=SHAPE_DEFINITION_REPRESENTATION(#66771,#66895);
#66732=SHAPE_DEFINITION_REPRESENTATION(#66772,#66896);
#66733=SHAPE_DEFINITION_REPRESENTATION(#66773,#66897);
#66734=SHAPE_DEFINITION_REPRESENTATION(#66776,#66898);
#66735=SHAPE_DEFINITION_REPRESENTATION(#66777,#66899);
#66736=SHAPE_DEFINITION_REPRESENTATION(#66778,#66900);
#66737=SHAPE_DEFINITION_REPRESENTATION(#66779,#66901);
#66738=SHAPE_DEFINITION_REPRESENTATION(#66780,#66902);
#66739=SHAPE_DEFINITION_REPRESENTATION(#66791,#66903);
#66740=SHAPE_DEFINITION_REPRESENTATION(#66792,#66904);
#66741=SHAPE_DEFINITION_REPRESENTATION(#66793,#66905);
#66742=SHAPE_DEFINITION_REPRESENTATION(#66796,#66906);
#66743=SHAPE_DEFINITION_REPRESENTATION(#66797,#66907);
#66744=SHAPE_DEFINITION_REPRESENTATION(#66798,#66908);
#66745=SHAPE_DEFINITION_REPRESENTATION(#66801,#66909);
#66746=SHAPE_DEFINITION_REPRESENTATION(#66802,#66910);
#66747=SHAPE_DEFINITION_REPRESENTATION(#66803,#66911);
#66748=SHAPE_DEFINITION_REPRESENTATION(#66804,#66912);
#66749=SHAPE_DEFINITION_REPRESENTATION(#66809,#66913);
#66750=SHAPE_DEFINITION_REPRESENTATION(#66810,#66914);
#66751=SHAPE_DEFINITION_REPRESENTATION(#66811,#66915);
#66752=SHAPE_DEFINITION_REPRESENTATION(#66812,#66916);
#66753=SHAPE_DEFINITION_REPRESENTATION(#66813,#66917);
#66754=SHAPE_DEFINITION_REPRESENTATION(#66814,#66918);
#66755=SHAPE_DEFINITION_REPRESENTATION(#66815,#66919);
#66756=SHAPE_DEFINITION_REPRESENTATION(#66816,#66920);
#66757=SHAPE_DEFINITION_REPRESENTATION(#66817,#66921);
#66758=SHAPE_DEFINITION_REPRESENTATION(#66818,#66922);
#66759=SHAPE_DEFINITION_REPRESENTATION(#66819,#66923);
#66760=SHAPE_DEFINITION_REPRESENTATION(#66820,#66924);
#66761=SHAPE_DEFINITION_REPRESENTATION(#66831,#66925);
#66762=SHAPE_DEFINITION_REPRESENTATION(#66832,#66926);
#66763=SHAPE_DEFINITION_REPRESENTATION(#66833,#66927);
#66764=SHAPE_DEFINITION_REPRESENTATION(#66834,#66928);
#66765=SHAPE_DEFINITION_REPRESENTATION(#66835,#66929);
#66766=PRODUCT_DEFINITION_SHAPE('',$,#66931);
#66767=PRODUCT_DEFINITION_SHAPE('',$,#66932);
#66768=PRODUCT_DEFINITION_SHAPE('',$,#66933);
#66769=PRODUCT_DEFINITION_SHAPE('',$,#66934);
#66770=PRODUCT_DEFINITION_SHAPE('',$,#66935);
#66771=PRODUCT_DEFINITION_SHAPE('',$,#66936);
#66772=PRODUCT_DEFINITION_SHAPE('',$,#66937);
#66773=PRODUCT_DEFINITION_SHAPE('',$,#66938);
#66774=PRODUCT_DEFINITION_SHAPE($,$,#952);
#66775=PRODUCT_DEFINITION_SHAPE($,$,#953);
#66776=PRODUCT_DEFINITION_SHAPE('',$,#66939);
#66777=PRODUCT_DEFINITION_SHAPE('',$,#66940);
#66778=PRODUCT_DEFINITION_SHAPE('',$,#66941);
#66779=PRODUCT_DEFINITION_SHAPE('',$,#66942);
#66780=PRODUCT_DEFINITION_SHAPE('',$,#66943);
#66781=PRODUCT_DEFINITION_SHAPE($,$,#954);
#66782=PRODUCT_DEFINITION_SHAPE($,$,#955);
#66783=PRODUCT_DEFINITION_SHAPE($,$,#956);
#66784=PRODUCT_DEFINITION_SHAPE($,$,#957);
#66785=PRODUCT_DEFINITION_SHAPE($,$,#958);
#66786=PRODUCT_DEFINITION_SHAPE($,$,#959);
#66787=PRODUCT_DEFINITION_SHAPE($,$,#960);
#66788=PRODUCT_DEFINITION_SHAPE($,$,#961);
#66789=PRODUCT_DEFINITION_SHAPE($,$,#962);
#66790=PRODUCT_DEFINITION_SHAPE($,$,#963);
#66791=PRODUCT_DEFINITION_SHAPE('',$,#66944);
#66792=PRODUCT_DEFINITION_SHAPE('',$,#66945);
#66793=PRODUCT_DEFINITION_SHAPE('',$,#66946);
#66794=PRODUCT_DEFINITION_SHAPE($,$,#964);
#66795=PRODUCT_DEFINITION_SHAPE($,$,#965);
#66796=PRODUCT_DEFINITION_SHAPE('',$,#66947);
#66797=PRODUCT_DEFINITION_SHAPE('',$,#66948);
#66798=PRODUCT_DEFINITION_SHAPE('',$,#66949);
#66799=PRODUCT_DEFINITION_SHAPE($,$,#966);
#66800=PRODUCT_DEFINITION_SHAPE($,$,#967);
#66801=PRODUCT_DEFINITION_SHAPE('',$,#66950);
#66802=PRODUCT_DEFINITION_SHAPE('',$,#66951);
#66803=PRODUCT_DEFINITION_SHAPE('',$,#66952);
#66804=PRODUCT_DEFINITION_SHAPE('',$,#66953);
#66805=PRODUCT_DEFINITION_SHAPE($,$,#968);
#66806=PRODUCT_DEFINITION_SHAPE($,$,#969);
#66807=PRODUCT_DEFINITION_SHAPE($,$,#970);
#66808=PRODUCT_DEFINITION_SHAPE($,$,#971);
#66809=PRODUCT_DEFINITION_SHAPE('',$,#66954);
#66810=PRODUCT_DEFINITION_SHAPE('',$,#66955);
#66811=PRODUCT_DEFINITION_SHAPE('',$,#66956);
#66812=PRODUCT_DEFINITION_SHAPE('',$,#66957);
#66813=PRODUCT_DEFINITION_SHAPE('',$,#66958);
#66814=PRODUCT_DEFINITION_SHAPE('',$,#66959);
#66815=PRODUCT_DEFINITION_SHAPE('',$,#66960);
#66816=PRODUCT_DEFINITION_SHAPE('',$,#66961);
#66817=PRODUCT_DEFINITION_SHAPE('',$,#66962);
#66818=PRODUCT_DEFINITION_SHAPE('',$,#66963);
#66819=PRODUCT_DEFINITION_SHAPE('',$,#66964);
#66820=PRODUCT_DEFINITION_SHAPE('',$,#66965);
#66821=PRODUCT_DEFINITION_SHAPE($,$,#972);
#66822=PRODUCT_DEFINITION_SHAPE($,$,#973);
#66823=PRODUCT_DEFINITION_SHAPE($,$,#974);
#66824=PRODUCT_DEFINITION_SHAPE($,$,#975);
#66825=PRODUCT_DEFINITION_SHAPE($,$,#976);
#66826=PRODUCT_DEFINITION_SHAPE($,$,#977);
#66827=PRODUCT_DEFINITION_SHAPE($,$,#978);
#66828=PRODUCT_DEFINITION_SHAPE($,$,#979);
#66829=PRODUCT_DEFINITION_SHAPE($,$,#980);
#66830=PRODUCT_DEFINITION_SHAPE($,$,#981);
#66831=PRODUCT_DEFINITION_SHAPE('',$,#66966);
#66832=PRODUCT_DEFINITION_SHAPE('',$,#66967);
#66833=PRODUCT_DEFINITION_SHAPE('',$,#66968);
#66834=PRODUCT_DEFINITION_SHAPE('',$,#66969);
#66835=PRODUCT_DEFINITION_SHAPE('',$,#66970);
#66836=PRODUCT_DEFINITION_SHAPE($,$,#982);
#66837=PRODUCT_DEFINITION_SHAPE($,$,#983);
#66838=PRODUCT_DEFINITION_SHAPE($,$,#984);
#66839=PRODUCT_DEFINITION_SHAPE($,$,#985);
#66840=PRODUCT_DEFINITION_SHAPE($,$,#986);
#66841=PRODUCT_DEFINITION_SHAPE($,$,#987);
#66842=PRODUCT_DEFINITION_SHAPE($,$,#988);
#66843=PRODUCT_DEFINITION_SHAPE($,$,#989);
#66844=PRODUCT_DEFINITION_SHAPE($,$,#990);
#66845=PRODUCT_DEFINITION_SHAPE($,$,#991);
#66846=PRODUCT_DEFINITION_SHAPE($,$,#992);
#66847=PRODUCT_DEFINITION_SHAPE($,$,#993);
#66848=PRODUCT_DEFINITION_SHAPE($,$,#994);
#66849=PRODUCT_DEFINITION_SHAPE($,$,#995);
#66850=PRODUCT_DEFINITION_SHAPE($,$,#996);
#66851=PRODUCT_DEFINITION_SHAPE($,$,#997);
#66852=PRODUCT_DEFINITION_SHAPE($,$,#998);
#66853=PRODUCT_DEFINITION_SHAPE($,$,#999);
#66854=PRODUCT_DEFINITION_SHAPE($,$,#1000);
#66855=PRODUCT_DEFINITION_SHAPE($,$,#1001);
#66856=PRODUCT_DEFINITION_SHAPE($,$,#1002);
#66857=PRODUCT_DEFINITION_SHAPE($,$,#1003);
#66858=PRODUCT_DEFINITION_SHAPE($,$,#1004);
#66859=PRODUCT_DEFINITION_SHAPE($,$,#1005);
#66860=PRODUCT_DEFINITION_SHAPE($,$,#1006);
#66861=PRODUCT_DEFINITION_SHAPE($,$,#1007);
#66862=PRODUCT_DEFINITION_SHAPE($,$,#1008);
#66863=PRODUCT_DEFINITION_SHAPE($,$,#1009);
#66864=PRODUCT_DEFINITION_SHAPE($,$,#1010);
#66865=PRODUCT_DEFINITION_SHAPE($,$,#1011);
#66866=PRODUCT_DEFINITION_SHAPE($,$,#1012);
#66867=PRODUCT_DEFINITION_SHAPE($,$,#1013);
#66868=PRODUCT_DEFINITION_SHAPE($,$,#1014);
#66869=PRODUCT_DEFINITION_SHAPE($,$,#1015);
#66870=PRODUCT_DEFINITION_SHAPE($,$,#1016);
#66871=PRODUCT_DEFINITION_SHAPE($,$,#1017);
#66872=PRODUCT_DEFINITION_SHAPE($,$,#1018);
#66873=PRODUCT_DEFINITION_SHAPE($,$,#1019);
#66874=PRODUCT_DEFINITION_SHAPE($,$,#1020);
#66875=PRODUCT_DEFINITION_SHAPE($,$,#1021);
#66876=PRODUCT_DEFINITION_SHAPE($,$,#1022);
#66877=PRODUCT_DEFINITION_SHAPE($,$,#1023);
#66878=PRODUCT_DEFINITION_SHAPE($,$,#1024);
#66879=PRODUCT_DEFINITION_SHAPE($,$,#1025);
#66880=PRODUCT_DEFINITION_SHAPE($,$,#1026);
#66881=PRODUCT_DEFINITION_SHAPE($,$,#1027);
#66882=PRODUCT_DEFINITION_SHAPE($,$,#1028);
#66883=PRODUCT_DEFINITION_SHAPE($,$,#1029);
#66884=PRODUCT_DEFINITION_SHAPE($,$,#1030);
#66885=PRODUCT_DEFINITION_SHAPE($,$,#1031);
#66886=PRODUCT_DEFINITION_SHAPE($,$,#1032);
#66887=PRODUCT_DEFINITION_SHAPE($,$,#1033);
#66888=PRODUCT_DEFINITION_SHAPE($,$,#1034);
#66889=PRODUCT_DEFINITION_SHAPE($,$,#1035);
#66890=SHAPE_REPRESENTATION('',(#26041,#28702,#28703,#28704,#28705,#28706,
#28707,#28708,#28709,#28710,#28711,#28712,#28713,#28714,#28715,#28716,#28717,
#28718,#28719,#28720,#28721,#28722,#28723,#28724,#28725,#28726,#28727,#28728,
#28729,#28730,#28731,#28732,#28733,#28734,#28735,#28736,#28737,#28738,#28739,
#28740,#28741,#28742,#28743,#28744,#28745,#28746,#28747,#28748,#28749,#28750,
#28751,#28752,#28753,#28754,#28755),#66681);
#66891=SHAPE_REPRESENTATION('',(#26042),#66682);
#66892=SHAPE_REPRESENTATION('',(#26069,#27264,#27265,#27266,#27267,#27268),
#66683);
#66893=SHAPE_REPRESENTATION('',(#26070),#66684);
#66894=SHAPE_REPRESENTATION('',(#26095),#66685);
#66895=SHAPE_REPRESENTATION('',(#26141,#26201,#26202),#66686);
#66896=SHAPE_REPRESENTATION('',(#26142),#66687);
#66897=SHAPE_REPRESENTATION('',(#26176),#66688);
#66898=SHAPE_REPRESENTATION('',(#26203),#66689);
#66899=SHAPE_REPRESENTATION('',(#26228,#27269,#27270,#27271,#27272,#27273),
#66690);
#66900=SHAPE_REPRESENTATION('',(#26229),#66691);
#66901=SHAPE_REPRESENTATION('',(#26592),#66692);
#66902=SHAPE_REPRESENTATION('',(#27192),#66693);
#66903=SHAPE_REPRESENTATION('',(#27274,#27392,#27393),#66694);
#66904=SHAPE_REPRESENTATION('',(#27275),#66695);
#66905=SHAPE_REPRESENTATION('',(#27328),#66696);
#66906=SHAPE_REPRESENTATION('',(#27394,#27468,#27469),#66697);
#66907=SHAPE_REPRESENTATION('',(#27395),#66698);
#66908=SHAPE_REPRESENTATION('',(#27435),#66699);
#66909=SHAPE_REPRESENTATION('',(#27470,#27677,#27678,#27679,#27680),#66700);
#66910=SHAPE_REPRESENTATION('',(#27471),#66701);
#66911=SHAPE_REPRESENTATION('',(#27602),#66702);
#66912=SHAPE_REPRESENTATION('',(#27668),#66703);
#66913=SHAPE_REPRESENTATION('',(#27681),#66704);
#66914=SHAPE_REPRESENTATION('',(#27712,#28478),#66705);
#66915=SHAPE_REPRESENTATION('',(#27713,#28469,#28470,#28471,#28472,#28473,
#28474,#28475,#28476,#28477),#66706);
#66916=SHAPE_REPRESENTATION('',(#27714),#66707);
#66917=SHAPE_REPRESENTATION('',(#27944),#66708);
#66918=SHAPE_REPRESENTATION('',(#27957),#66709);
#66919=SHAPE_REPRESENTATION('',(#27979),#66710);
#66920=SHAPE_REPRESENTATION('',(#28001),#66711);
#66921=SHAPE_REPRESENTATION('',(#28209),#66712);
#66922=SHAPE_REPRESENTATION('',(#28222),#66713);
#66923=SHAPE_REPRESENTATION('',(#28244),#66714);
#66924=SHAPE_REPRESENTATION('',(#28266),#66715);
#66925=SHAPE_REPRESENTATION('',(#28479),#66716);
#66926=SHAPE_REPRESENTATION('',(#28564),#66717);
#66927=SHAPE_REPRESENTATION('',(#28586),#66718);
#66928=SHAPE_REPRESENTATION('',(#28641),#66719);
#66929=SHAPE_REPRESENTATION('',(#28680),#66720);
#66930=PRODUCT_DEFINITION_CONTEXT('part definition',#67052,'design');
#66931=PRODUCT_DEFINITION('BALL SCREW ASSLY SET-UP','TAS-015',#66971,#66930);
#66932=PRODUCT_DEFINITION('Main Plate','Main Plate',#66972,#66930);
#66933=PRODUCT_DEFINITION('Linear Guide Assembly 1',
'Linear Guide Assembly 1',#66973,#66930);
#66934=PRODUCT_DEFINITION('Ball Screw Spacer 2','Ball Screw Spacer 2',#66974,
#66930);
#66935=PRODUCT_DEFINITION('Motor Mount Plate','Motor Mount Plate',#66975,
#66930);
#66936=PRODUCT_DEFINITION('Ball Screw Support Assembly',
'Ball Screw Support Assembly',#66976,#66930);
#66937=PRODUCT_DEFINITION('Ball Screw Support Bracket',
'Ball Screw Support Bracket',#66977,#66930);
#66938=PRODUCT_DEFINITION('Ball Screw Support Plate',
'Ball Screw Support Plate',#66978,#66930);
#66939=PRODUCT_DEFINITION('Ball Screw Support Spacer',
'Ball Screw Support Spacer',#66979,#66930);
#66940=PRODUCT_DEFINITION('Linear Guide Assembly 2',
'Linear Guide Assembly 2',#66980,#66930);
#66941=PRODUCT_DEFINITION('Linear Guide Rail','Linear Guide Rail',#66981,
#66930);
#66942=PRODUCT_DEFINITION('Linear Guide Slider','Linear Guide Slider',#66982,
#66930);
#66943=PRODUCT_DEFINITION('Slider End Cap','Slider End Cap',#66983,#66930);
#66944=PRODUCT_DEFINITION('Ball Screw Assembly','Ball Screw Assembly',#66984,
#66930);
#66945=PRODUCT_DEFINITION('Ball Screw Shaft','Ball Screw Shaft',#66985,
#66930);
#66946=PRODUCT_DEFINITION('Ball Screw Nut','Ball Screw Nut',#66986,#66930);
#66947=PRODUCT_DEFINITION('Fixed Bearing Support Assembly',
'Fixed Bearing Support Assembly',#66987,#66930);
#66948=PRODUCT_DEFINITION('Fixed Bearing Housing',
'Fixed Bearing Housing',#66988,#66930);
#66949=PRODUCT_DEFINITION('Washer','Washer',#66989,#66930);
#66950=PRODUCT_DEFINITION('Floating Bearing Support Assembly',
'Floating Bearing Support Assembly',#66990,#66930);
#66951=PRODUCT_DEFINITION('Floating Bearing Housing',
'Floating Bearing Housing',#66991,#66930);
#66952=PRODUCT_DEFINITION('Lock Nut','Lock Nut',#66992,#66930);
#66953=PRODUCT_DEFINITION('Collar','Collar',#66993,#66930);
#66954=PRODUCT_DEFINITION('Ball Screw Spacer 1','Ball Screw Spacer 1',#66994,
#66930);
#66955=PRODUCT_DEFINITION('Coupling Assembly','Coupling Assembly',#66995,
#66930);
#66956=PRODUCT_DEFINITION('Coupling Components','Coupling Components',#66996,
#66930);
#66957=PRODUCT_DEFINITION('Coupling Spider','Coupling Spider',#66997,#66930);
#66958=PRODUCT_DEFINITION('Coupling Set Screw','Coupling Set Screw',#66998,
#66930);
#66959=PRODUCT_DEFINITION('Coupling Clamp Screw 1',
'Coupling Clamp Screw 1',#66999,#66930);
#66960=PRODUCT_DEFINITION('Coupling Clamp Screw 2',
'Coupling Clamp Screw 2',#67000,#66930);
#66961=PRODUCT_DEFINITION('Coupling Hub 2','Coupling Hub 2',#67001,#66930);
#66962=PRODUCT_DEFINITION('Coupling Washer','Coupling Washer',#67002,#66930);
#66963=PRODUCT_DEFINITION('Coupling Clamp Ring 1',
'Coupling Clamp Ring 1',#67003,#66930);
#66964=PRODUCT_DEFINITION('Coupling Clamp Ring 2',
'Coupling Clamp Ring 2',#67004,#66930);
#66965=PRODUCT_DEFINITION('Coupling Hub 1','Coupling Hub 1',#67005,#66930);
#66966=PRODUCT_DEFINITION('Linear Guide Spacer','Linear Guide Spacer',#67006,
#66930);
#66967=PRODUCT_DEFINITION('Socket head cap screw M6x20',
'Socket Head Cap Screw M6x20',#67007,#66930);
#66968=PRODUCT_DEFINITION('Low Head Cap Screw M6x25',
'Low Head Cap Screw M6x25',#67008,#66930);
#66969=PRODUCT_DEFINITION('Linear Slider Spacer','Linear Slider Spacer',
#67009,#66930);
#66970=PRODUCT_DEFINITION('Socket head cap screw M6x25',
'Socket Head Cap Screw M6x25',#67010,#66930);
#66971=PRODUCT_DEFINITION_FORMATION('',$,#67054);
#66972=PRODUCT_DEFINITION_FORMATION('',$,#67055);
#66973=PRODUCT_DEFINITION_FORMATION('',$,#67056);
#66974=PRODUCT_DEFINITION_FORMATION('',$,#67057);
#66975=PRODUCT_DEFINITION_FORMATION('',$,#67058);
#66976=PRODUCT_DEFINITION_FORMATION('',$,#67059);
#66977=PRODUCT_DEFINITION_FORMATION('',$,#67060);
#66978=PRODUCT_DEFINITION_FORMATION('',$,#67061);
#66979=PRODUCT_DEFINITION_FORMATION('',$,#67062);
#66980=PRODUCT_DEFINITION_FORMATION('',$,#67063);
#66981=PRODUCT_DEFINITION_FORMATION('',$,#67064);
#66982=PRODUCT_DEFINITION_FORMATION('',$,#67065);
#66983=PRODUCT_DEFINITION_FORMATION('',$,#67066);
#66984=PRODUCT_DEFINITION_FORMATION('',$,#67067);
#66985=PRODUCT_DEFINITION_FORMATION('',$,#67068);
#66986=PRODUCT_DEFINITION_FORMATION('',$,#67069);
#66987=PRODUCT_DEFINITION_FORMATION('',$,#67070);
#66988=PRODUCT_DEFINITION_FORMATION('',$,#67071);
#66989=PRODUCT_DEFINITION_FORMATION('',$,#67072);
#66990=PRODUCT_DEFINITION_FORMATION('',$,#67073);
#66991=PRODUCT_DEFINITION_FORMATION('',$,#67074);
#66992=PRODUCT_DEFINITION_FORMATION('',$,#67075);
#66993=PRODUCT_DEFINITION_FORMATION('',$,#67076);
#66994=PRODUCT_DEFINITION_FORMATION('',$,#67077);
#66995=PRODUCT_DEFINITION_FORMATION('',$,#67078);
#66996=PRODUCT_DEFINITION_FORMATION('',$,#67079);
#66997=PRODUCT_DEFINITION_FORMATION('',$,#67080);
#66998=PRODUCT_DEFINITION_FORMATION('',$,#67081);
#66999=PRODUCT_DEFINITION_FORMATION('',$,#67082);
#67000=PRODUCT_DEFINITION_FORMATION('',$,#67083);
#67001=PRODUCT_DEFINITION_FORMATION('',$,#67084);
#67002=PRODUCT_DEFINITION_FORMATION('',$,#67085);
#67003=PRODUCT_DEFINITION_FORMATION('',$,#67086);
#67004=PRODUCT_DEFINITION_FORMATION('',$,#67087);
#67005=PRODUCT_DEFINITION_FORMATION('',$,#67088);
#67006=PRODUCT_DEFINITION_FORMATION('',$,#67089);
#67007=PRODUCT_DEFINITION_FORMATION('',$,#67090);
#67008=PRODUCT_DEFINITION_FORMATION('',$,#67091);
#67009=PRODUCT_DEFINITION_FORMATION('',$,#67092);
#67010=PRODUCT_DEFINITION_FORMATION('',$,#67093);
#67011=PRODUCT_RELATED_PRODUCT_CATEGORY('TAS-015','TAS-015',(#67054));
#67012=PRODUCT_RELATED_PRODUCT_CATEGORY('Main Plate','Main Plate',(#67055));
#67013=PRODUCT_RELATED_PRODUCT_CATEGORY('Linear Guide Assembly 1',
'Linear Guide Assembly 1',(#67056));
#67014=PRODUCT_RELATED_PRODUCT_CATEGORY('Ball Screw Spacer 2',
'Ball Screw Spacer 2',(#67057));
#67015=PRODUCT_RELATED_PRODUCT_CATEGORY('Motor Mount Plate',
'Motor Mount Plate',(#67058));
#67016=PRODUCT_RELATED_PRODUCT_CATEGORY('Ball Screw Support Assembly',
'Ball Screw Support Assembly',(#67059));
#67017=PRODUCT_RELATED_PRODUCT_CATEGORY('Ball Screw Support Bracket',
'Ball Screw Support Bracket',(#67060));
#67018=PRODUCT_RELATED_PRODUCT_CATEGORY('Ball Screw Support Plate',
'Ball Screw Support Plate',(#67061));
#67019=PRODUCT_RELATED_PRODUCT_CATEGORY('Ball Screw Support Spacer',
'Ball Screw Support Spacer',(#67062));
#67020=PRODUCT_RELATED_PRODUCT_CATEGORY('Linear Guide Assembly 2',
'Linear Guide Assembly 2',(#67063));
#67021=PRODUCT_RELATED_PRODUCT_CATEGORY('Linear Guide Rail',
'Linear Guide Rail',(#67064));
#67022=PRODUCT_RELATED_PRODUCT_CATEGORY('Linear Guide Slider',
'Linear Guide Slider',(#67065));
#67023=PRODUCT_RELATED_PRODUCT_CATEGORY('Slider End Cap',
'Slider End Cap',(#67066));
#67024=PRODUCT_RELATED_PRODUCT_CATEGORY('Ball Screw Assembly',
'Ball Screw Assembly',(#67067));
#67025=PRODUCT_RELATED_PRODUCT_CATEGORY('Ball Screw Shaft',
'Ball Screw Shaft',(#67068));
#67026=PRODUCT_RELATED_PRODUCT_CATEGORY('Ball Screw Nut',
'Ball Screw Nut',(#67069));
#67027=PRODUCT_RELATED_PRODUCT_CATEGORY(
'Fixed Bearing Support Assembly','Fixed Bearing Support Assembly',(#67070));
#67028=PRODUCT_RELATED_PRODUCT_CATEGORY('Fixed Bearing Housing',
'Fixed Bearing Housing',(#67071));
#67029=PRODUCT_RELATED_PRODUCT_CATEGORY('Washer','Washer',(#67072));
#67030=PRODUCT_RELATED_PRODUCT_CATEGORY(
'Floating Bearing Support Assembly','Floating Bearing Support Assembly',
(#67073));
#67031=PRODUCT_RELATED_PRODUCT_CATEGORY('Floating Bearing Housing',
'Floating Bearing Housing',(#67074));
#67032=PRODUCT_RELATED_PRODUCT_CATEGORY('Lock Nut','Lock Nut',(#67075));
#67033=PRODUCT_RELATED_PRODUCT_CATEGORY('Collar','Collar',(#67076));
#67034=PRODUCT_RELATED_PRODUCT_CATEGORY('Ball Screw Spacer 1',
'Ball Screw Spacer 1',(#67077));
#67035=PRODUCT_RELATED_PRODUCT_CATEGORY('Coupling Assembly',
'Coupling Assembly',(#67078));
#67036=PRODUCT_RELATED_PRODUCT_CATEGORY('Coupling Components',
'Coupling Components',(#67079));
#67037=PRODUCT_RELATED_PRODUCT_CATEGORY('Coupling Spider',
'Coupling Spider',(#67080));
#67038=PRODUCT_RELATED_PRODUCT_CATEGORY('Coupling Set Screw',
'Coupling Set Screw',(#67081));
#67039=PRODUCT_RELATED_PRODUCT_CATEGORY('Coupling Clamp Screw 1',
'Coupling Clamp Screw 1',(#67082));
#67040=PRODUCT_RELATED_PRODUCT_CATEGORY('Coupling Clamp Screw 2',
'Coupling Clamp Screw 2',(#67083));
#67041=PRODUCT_RELATED_PRODUCT_CATEGORY('Coupling Hub 2',
'Coupling Hub 2',(#67084));
#67042=PRODUCT_RELATED_PRODUCT_CATEGORY('Coupling Washer',
'Coupling Washer',(#67085));
#67043=PRODUCT_RELATED_PRODUCT_CATEGORY('Coupling Clamp Ring 1',
'Coupling Clamp Ring 1',(#67086));
#67044=PRODUCT_RELATED_PRODUCT_CATEGORY('Coupling Clamp Ring 2',
'Coupling Clamp Ring 2',(#67087));
#67045=PRODUCT_RELATED_PRODUCT_CATEGORY('Coupling Hub 1',
'Coupling Hub 1',(#67088));
#67046=PRODUCT_RELATED_PRODUCT_CATEGORY('Linear Guide Spacer',
'Linear Guide Spacer',(#67089));
#67047=PRODUCT_RELATED_PRODUCT_CATEGORY('Socket Head Cap Screw M6x20',
'Socket Head Cap Screw M6x20',(#67090));
#67048=PRODUCT_RELATED_PRODUCT_CATEGORY('Low Head Cap Screw M6x25',
'Low Head Cap Screw M6x25',(#67091));
#67049=PRODUCT_RELATED_PRODUCT_CATEGORY('Linear Slider Spacer',
'Linear Slider Spacer',(#67092));
#67050=PRODUCT_RELATED_PRODUCT_CATEGORY('Socket Head Cap Screw M6x25',
'Socket Head Cap Screw M6x25',(#67093));
#67051=APPLICATION_PROTOCOL_DEFINITION('international standard',
'automotive_design',2009,#67052);
#67052=APPLICATION_CONTEXT(
'Core Data for Automotive Mechanical Design Process');
#67053=PRODUCT_CONTEXT('part definition',#67052,'mechanical');
#67054=PRODUCT('BALL SCREW ASSLY SET-UP','TAS-015','STEP AP214',(#67053));
#67055=PRODUCT('Main Plate','Main Plate',$,(#67053));
#67056=PRODUCT('Linear Guide Assembly 1','Linear Guide Assembly 1',$,(#67053));
#67057=PRODUCT('Ball Screw Spacer 2','Ball Screw Spacer 2',$,(#67053));
#67058=PRODUCT('Motor Mount Plate','Motor Mount Plate',$,(#67053));
#67059=PRODUCT('Ball Screw Support Assembly',
'Ball Screw Support Assembly',$,(#67053));
#67060=PRODUCT('Ball Screw Support Bracket',
'Ball Screw Support Bracket',$,(#67053));
#67061=PRODUCT('Ball Screw Support Plate','Ball Screw Support Plate',$,
(#67053));
#67062=PRODUCT('Ball Screw Support Spacer','Ball Screw Support Spacer',
$,(#67053));
#67063=PRODUCT('Linear Guide Assembly 2','Linear Guide Assembly 2',$,(#67053));
#67064=PRODUCT('Linear Guide Rail','Linear Guide Rail',$,(#67053));
#67065=PRODUCT('Linear Guide Slider','Linear Guide Slider',$,(#67053));
#67066=PRODUCT('Slider End Cap','Slider End Cap',$,(#67053));
#67067=PRODUCT('Ball Screw Assembly','Ball Screw Assembly',$,(#67053));
#67068=PRODUCT('Ball Screw Shaft','Ball Screw Shaft',$,(#67053));
#67069=PRODUCT('Ball Screw Nut','Ball Screw Nut',$,(#67053));
#67070=PRODUCT('Fixed Bearing Support Assembly',
'Fixed Bearing Support Assembly',$,(#67053));
#67071=PRODUCT('Fixed Bearing Housing','Fixed Bearing Housing',$,(#67053));
#67072=PRODUCT('Washer','Washer',$,(#67053));
#67073=PRODUCT('Floating Bearing Support Assembly',
'Floating Bearing Support Assembly',$,(#67053));
#67074=PRODUCT('Floating Bearing Housing','Floating Bearing Housing',$,
(#67053));
#67075=PRODUCT('Lock Nut','Lock Nut',$,(#67053));
#67076=PRODUCT('Collar','Collar',$,(#67053));
#67077=PRODUCT('Ball Screw Spacer 1','Ball Screw Spacer 1',$,(#67053));
#67078=PRODUCT('Coupling Assembly','Coupling Assembly',$,(#67053));
#67079=PRODUCT('Coupling Components','Coupling Components',$,(#67053));
#67080=PRODUCT('Coupling Spider','Coupling Spider',$,(#67053));
#67081=PRODUCT('Coupling Set Screw','Coupling Set Screw',$,(#67053));
#67082=PRODUCT('Coupling Clamp Screw 1','Coupling Clamp Screw 1',$,(#67053));
#67083=PRODUCT('Coupling Clamp Screw 2','Coupling Clamp Screw 2',$,(#67053));
#67084=PRODUCT('Coupling Hub 2','Coupling Hub 2',$,(#67053));
#67085=PRODUCT('Coupling Washer','Coupling Washer',$,(#67053));
#67086=PRODUCT('Coupling Clamp Ring 1','Coupling Clamp Ring 1',$,(#67053));
#67087=PRODUCT('Coupling Clamp Ring 2','Coupling Clamp Ring 2',$,(#67053));
#67088=PRODUCT('Coupling Hub 1','Coupling Hub 1',$,(#67053));
#67089=PRODUCT('Linear Guide Spacer','Linear Guide Spacer',$,(#67053));
#67090=PRODUCT('Socket head cap screw M6x20',
'Socket Head Cap Screw M6x20',$,(#67053));
#67091=PRODUCT('Low Head Cap Screw M6x25','Low Head Cap Screw M6x25',$,
(#67053));
#67092=PRODUCT('Linear Slider Spacer','Linear Slider Spacer',$,(#67053));
#67093=PRODUCT('Socket head cap screw M6x25',
'Socket Head Cap Screw M6x25',$,(#67053));
#67094=PRESENTATION_STYLE_ASSIGNMENT((#67096));
#67095=PRESENTATION_STYLE_ASSIGNMENT((#67097));
#67096=SURFACE_STYLE_USAGE(.BOTH.,#67098);
#67097=SURFACE_STYLE_USAGE(.BOTH.,#67099);
#67098=SURFACE_SIDE_STYLE('',(#67100));
#67099=SURFACE_SIDE_STYLE('',(#67101));
#67100=SURFACE_STYLE_FILL_AREA(#67102);
#67101=SURFACE_STYLE_FILL_AREA(#67103);
#67102=FILL_AREA_STYLE('Steel - Satin',(#67104));
#67103=FILL_AREA_STYLE('Opaque(202,209,238)',(#67105));
#67104=FILL_AREA_STYLE_COLOUR('Steel - Satin',#67106);
#67105=FILL_AREA_STYLE_COLOUR('Opaque(202,209,238)',#67107);
#67106=COLOUR_RGB('Steel - Satin',0.627450980392157,0.627450980392157,0.627450980392157);
#67107=COLOUR_RGB('Opaque(202,209,238)',0.792156862745098,0.819607843137255,
0.933333333333333);
ENDSEC;
END-ISO-10303-21;
